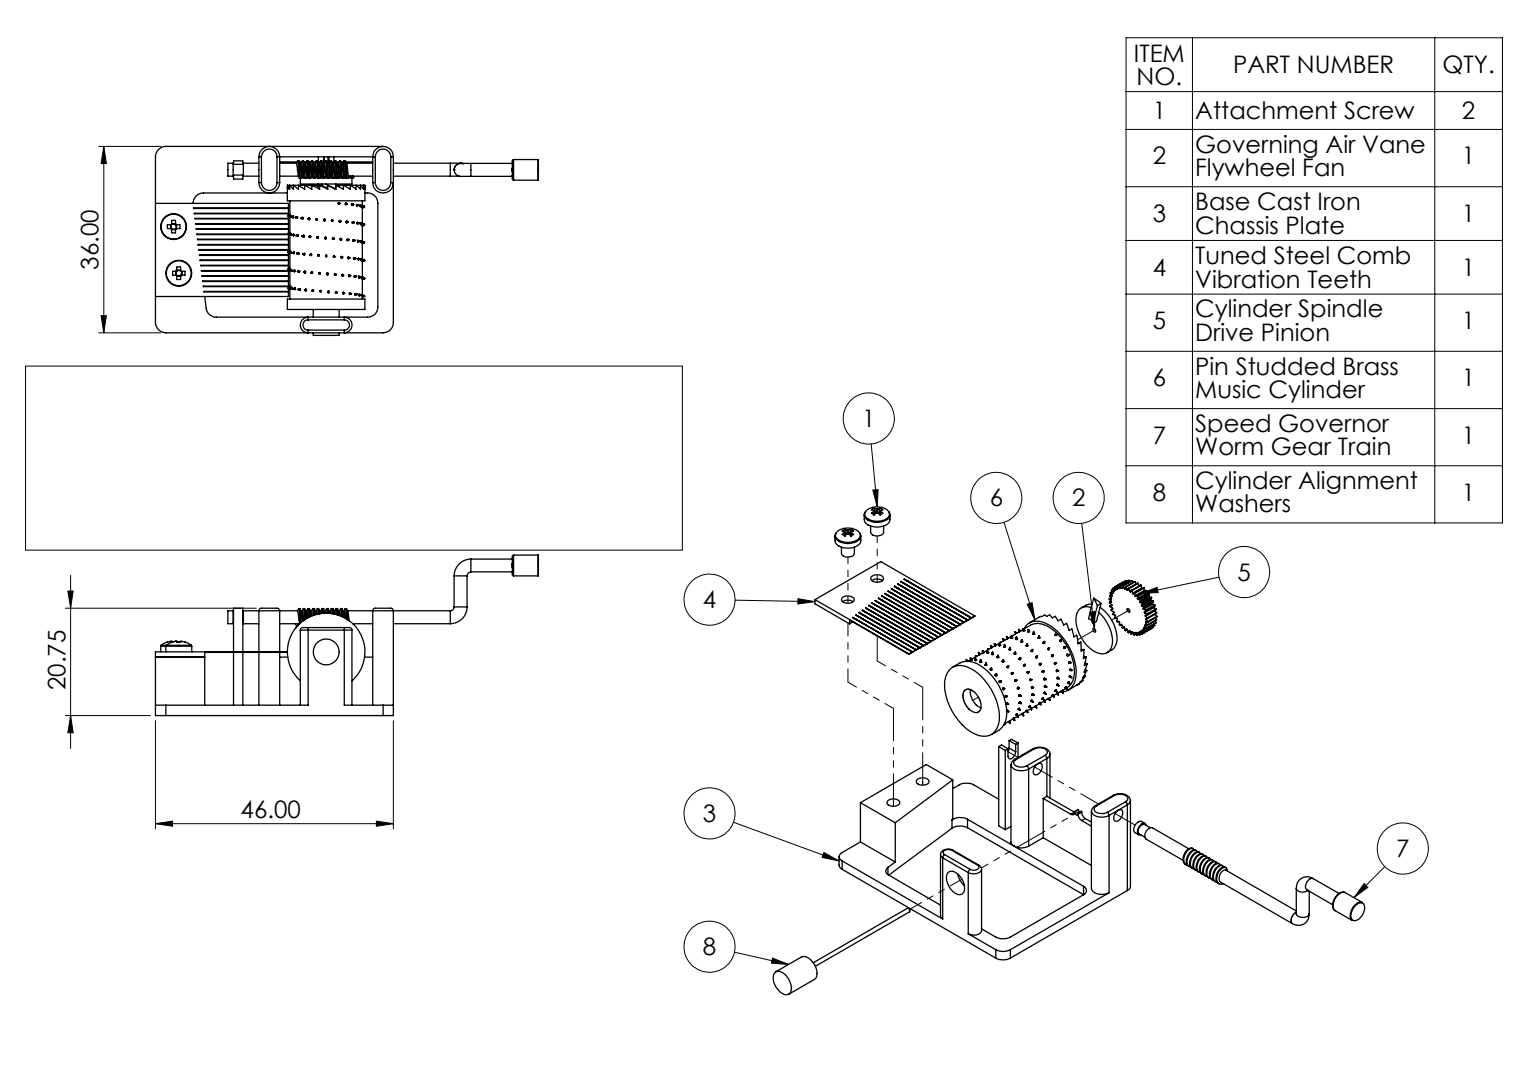
ISO-10303-21;
HEADER;
FILE_DESCRIPTION (('STEP AP214'),
    '1' );
FILE_NAME ('MAS-175',
    '2026-10-09T09:51:18',
    ( '' ),
    ( '' ),
    'SwSTEP 2.0',
    'SolidWorks 2026',
    '' );
FILE_SCHEMA (( 'AUTOMOTIVE_DESIGN' ));
ENDSEC;

DATA;
#1 = SHAPE_REPRESENTATION_RELATIONSHIP ( 'NONE' , 'NONE' ,  #34837, #17929 ) ;
#2 = ADVANCED_FACE ( 'NONE', ( #22899 ), #34188, .F. ) ;
#3 = CARTESIAN_POINT ( 'NONE',  ( -10.03625575236388201, -13.84871804469525891, 57.54850793716612856 ) ) ;
#4 = CARTESIAN_POINT ( 'NONE',  ( -11.98370840013613225, -9.620047919863830899, 54.02312124697528617 ) ) ;
#5 = ADVANCED_FACE ( 'NONE', ( #2758, #44164 ), #246, .T. ) ;
#6 = ORIENTED_EDGE ( 'NONE', *, *, #28225, .T. ) ;
#7 = EDGE_CURVE ( 'NONE', #38833, #36313, #30041, .T. ) ;
#8 = ORIENTED_EDGE ( 'NONE', *, *, #40110, .F. ) ;
#9 = CARTESIAN_POINT ( 'NONE',  ( -24.74075724160099554, -16.21284971877490122, 62.77824058731629009 ) ) ;
#10 = CARTESIAN_POINT ( 'NONE',  ( -15.47038646904106685, -21.58309222549749506, 72.34575460768671462 ) ) ;
#11 = CARTESIAN_POINT ( 'NONE',  ( -11.58081676984627073, -10.85831292256293068, 57.30083494179207548 ) ) ;
#12 = CIRCLE ( 'NONE', #29107, 1.999999999999999556 ) ;
#13 = EDGE_CURVE ( 'NONE', #13987, #23723, #5050, .T. ) ;
#14 = VERTEX_POINT ( 'NONE', #21494 ) ;
#15 = AXIS2_PLACEMENT_3D ( 'NONE', #40029, #47896, #25252 ) ;
#16 = PLANE ( 'NONE',  #21145 ) ;
#17 = B_SPLINE_CURVE_WITH_KNOTS ( 'NONE', 3,
 ( #43534, #12980, #31711, #43034, #46503, #38613, #46737, #9313, #19907, #1178 ),
 .UNSPECIFIED., .F., .F.,
 ( 4, 2, 2, 2, 4 ),
 ( 0.1272669073658292960, 0.2522669073463885137, 0.3772669073268680728, 0.5022669073073477986, 0.6272669072878274132 ),
 .UNSPECIFIED. ) ;
#18 = DIRECTION ( 'NONE',  ( 0.9939059412784551073, 0.1102314832132140626, 5.576311685107536405E-08 ) ) ;
#19 = ORIENTED_EDGE ( 'NONE', *, *, #29500, .F. ) ;
#20 = DIRECTION ( 'NONE',  ( -1.927470528863183637E-16, -1.434740771370715221E-29, 1.000000000000000000 ) ) ;
#21 = CARTESIAN_POINT ( 'NONE',  ( -10.31364510401727053, -17.03300888149450998, 57.80265138661536639 ) ) ;
#22 = DIRECTION ( 'NONE',  ( -0.7107718805962432995, -0.7034225854731134264, -7.722840056494082694E-09 ) ) ;
#23 = ORIENTED_EDGE ( 'NONE', *, *, #45455, .T. ) ;
#24 = CARTESIAN_POINT ( 'NONE',  ( -21.68606299684865135, -9.256084799238676553, 66.66150029161380530 ) ) ;
#25 = VERTEX_POINT ( 'NONE', #6474 ) ;
#26 = PLANE ( 'NONE',  #30712 ) ;
#27 = FACE_OUTER_BOUND ( 'NONE', #8967, .T. ) ;
#28 = VERTEX_POINT ( 'NONE', #28867 ) ;
#29 = CARTESIAN_POINT ( 'NONE',  ( 18.07590614458695200, 1.644079634528023526, 49.42952874619304282 ) ) ;
#30 = CARTESIAN_POINT ( 'NONE',  ( -19.85891393954322837, -21.37210614461000091, 75.49999999999994316 ) ) ;
#31 = CARTESIAN_POINT ( 'NONE',  ( -20.58659385650551599, -9.302874398569244363, 51.68646062012417985 ) ) ;
#32 = CARTESIAN_POINT ( 'NONE',  ( -20.17268404433175633, -8.371407854712250796, 70.55100341248845552 ) ) ;
#33 = EDGE_CURVE ( 'NONE', #48317, #41762, #10165, .T. ) ;
#34 = CARTESIAN_POINT ( 'NONE',  ( -10.76587051450098542, -16.97017341121004463, 57.68760522235623966 ) ) ;
#35 = DIRECTION ( 'NONE',  ( -0.000000000000000000, -1.000000000000000000, 0.000000000000000000 ) ) ;
#36 = CARTESIAN_POINT ( 'NONE',  ( -14.44705700679302574, -7.979876293330282699, 63.93978841086359211 ) ) ;
#37 = ORIENTED_EDGE ( 'NONE', *, *, #6492, .T. ) ;
#38 = CARTESIAN_POINT ( 'NONE',  ( -22.35534385541302527, -8.623186033802584305, 49.24843789510462955 ) ) ;
#39 = DIRECTION ( 'NONE',  ( -3.071710424422018668E-17, 6.404604876783312462E-16, 1.000000000000000000 ) ) ;
#40 = LINE ( 'NONE', #15026, #36087 ) ;
#41 = DIRECTION ( 'NONE',  ( -0.9942595023566571655, 0.1069955231469581908, -3.800058679842194246E-08 ) ) ;
#42 = CARTESIAN_POINT ( 'NONE',  ( -45.46395726858714426, -13.72754205882879042, 70.13000000000000966 ) ) ;
#43 = LINE ( 'NONE', #45603, #5826 ) ;
#44 = ORIENTED_EDGE ( 'NONE', *, *, #25310, .F. ) ;
#45 = ORIENTED_EDGE ( 'NONE', *, *, #29252, .T. ) ;
#46 = AXIS2_PLACEMENT_3D ( 'NONE', #24798, #28249, #13682 ) ;
#47 = CARTESIAN_POINT ( 'NONE',  ( -16.84904657224188540, -21.78683024590906925, 72.39373074617707005 ) ) ;
#48 = CARTESIAN_POINT ( 'NONE',  ( -13.27770768808251134, -9.107454094634595876, 63.90946529206384241 ) ) ;
#49 = ORIENTED_EDGE ( 'NONE', *, *, #23162, .T. ) ;
#50 = CARTESIAN_POINT ( 'NONE',  ( -24.00746423591236933, -17.19188279365308603, 73.11165851276361138 ) ) ;
#51 = CARTESIAN_POINT ( 'NONE',  ( -24.18314854330451169, -12.98801962294919932, 66.30246782466414857 ) ) ;
#52 = CARTESIAN_POINT ( 'NONE',  ( -11.64944166978149909, -18.76574910929434736, 64.81995021385422717 ) ) ;
#53 = CARTESIAN_POINT ( 'NONE',  ( -24.72694767484942702, -16.28301260341204326, 62.70833288210281609 ) ) ;
#54 = DIRECTION ( 'NONE',  ( 0.5088156898428700670, 0.8608754809899750171, 5.922709712265242817E-08 ) ) ;
#55 = CARTESIAN_POINT ( 'NONE',  ( -19.57699614054808634, -21.94144247634149281, 62.17999043330664222 ) ) ;
#56 = AXIS2_PLACEMENT_3D ( 'NONE', #16644, #27734, #1141 ) ;
#57 = CARTESIAN_POINT ( 'NONE',  ( -12.74071866071660075, -9.015263582886822391, 70.96429948631303830 ) ) ;
#58 = DIRECTION ( 'NONE',  ( 0.5088156898428700670, 0.8608754809899751281, 5.922709712265243479E-08 ) ) ;
#59 = CARTESIAN_POINT ( 'NONE',  ( -10.02934067034867915, -15.71522136325494579, 61.14450729704604015 ) ) ;
#60 = ORIENTED_EDGE ( 'NONE', *, *, #2656, .T. ) ;
#61 = CARTESIAN_POINT ( 'NONE',  ( -10.21764062494887781, -12.91954801228597915, 67.92327636273336111 ) ) ;
#62 = ADVANCED_FACE ( 'NONE', ( #10414 ), #3672, .F. ) ;
#63 = VECTOR ( 'NONE', #41726, 1000.000000000000114 ) ;
#64 = LINE ( 'NONE', #7461, #9828 ) ;
#65 = DIRECTION ( 'NONE',  ( -3.071710424422018668E-17, 6.404604876783312462E-16, 1.000000000000000000 ) ) ;
#66 = CARTESIAN_POINT ( 'NONE',  ( -21.34284385541298334, -7.587656875400150547, 49.25157356644804452 ) ) ;
#67 = CARTESIAN_POINT ( 'NONE',  ( -11.89176969907138570, -10.51836715134331079, 74.66715118432504994 ) ) ;
#68 = CARTESIAN_POINT ( 'NONE',  ( -45.92409385541305511, -17.80920654474410370, 70.50000000000000000 ) ) ;
#69 = ORIENTED_EDGE ( 'NONE', *, *, #36924, .F. ) ;
#70 = VERTEX_POINT ( 'NONE', #18679 ) ;
#71 = CARTESIAN_POINT ( 'NONE',  ( -14.25534385541304339, -8.623186033802571870, 49.24843789510467218 ) ) ;
#72 = EDGE_CURVE ( 'NONE', #44245, #17093, #1589, .T. ) ;
#73 = VERTEX_POINT ( 'NONE', #14975 ) ;
#74 = FACE_OUTER_BOUND ( 'NONE', #13777, .T. ) ;
#75 = AXIS2_PLACEMENT_3D ( 'NONE', #46607, #16288, #28114 ) ;
#76 = MANIFOLD_SOLID_BREP ( 'Stock-MAS-175-1', #12603 ) ;
#77 = CYLINDRICAL_SURFACE ( 'NONE', #4036, 0.1500000000000066835 ) ;
#78 = ADVANCED_FACE ( 'NONE', ( #20432 ), #5892, .T. ) ;
#79 = B_SPLINE_CURVE_WITH_KNOTS ( 'NONE', 1,
 ( #16390, #46203 ),
 .UNSPECIFIED., .F., .F.,
 ( 2, 2 ),
 ( 0.000000000000000000, 1.000000000000000000 ),
 .UNSPECIFIED. ) ;
#80 = AXIS2_PLACEMENT_3D ( 'NONE', #16934, #39604, #9337 ) ;
#81 = DIRECTION ( 'NONE',  ( 3.549360974555109863E-17, 1.977132801529350715E-16, 1.000000000000000000 ) ) ;
#82 = CARTESIAN_POINT ( 'NONE',  ( -18.31357640787765817, -21.80286941108919763, 68.81514702304139064 ) ) ;
#83 = EDGE_LOOP ( 'NONE', ( #31315, #30572, #42863, #38063 ) ) ;
#84 = VECTOR ( 'NONE', #15701, 1000.000000000000000 ) ;
#85 = PLANE ( 'NONE',  #90 ) ;
#86 = CARTESIAN_POINT ( 'NONE',  ( -24.16097951573440383, -12.71927508598556322, 66.51066513624088827 ) ) ;
#87 = ORIENTED_EDGE ( 'NONE', *, *, #46598, .F. ) ;
#88 = CARTESIAN_POINT ( 'NONE',  ( -22.33685117127641817, -20.40992557423668430, 62.42777465437541196 ) ) ;
#89 = EDGE_CURVE ( 'NONE', #5768, #15899, #14150, .T. ) ;
#90 = AXIS2_PLACEMENT_3D ( 'NONE', #14327, #11160, #7719 ) ;
#91 = CARTESIAN_POINT ( 'NONE',  ( -13.88293259567353743, -20.90532631576516565, 68.45625136994867432 ) ) ;
#92 = EDGE_CURVE ( 'NONE', #20698, #38947, #146, .T. ) ;
#93 = VERTEX_POINT ( 'NONE', #9602 ) ;
#94 = CARTESIAN_POINT ( 'NONE',  ( 10.57590614458695377, 0.6407533398237040823, 50.52649563099625851 ) ) ;
#95 = CARTESIAN_POINT ( 'NONE',  ( -10.02191625022346955, -15.65273779443635327, 61.15293638507743168 ) ) ;
#96 = EDGE_CURVE ( 'NONE', #20442, #47219, #874, .T. ) ;
#97 = ORIENTED_EDGE ( 'NONE', *, *, #12541, .T. ) ;
#98 = CARTESIAN_POINT ( 'NONE',  ( -10.46033444208452501, -13.68630826424936231, 57.74825279763368968 ) ) ;
#99 = LINE ( 'NONE', #37740, #35189 ) ;
#100 =( BOUNDED_CURVE ( )  B_SPLINE_CURVE ( 2, ( #3305, #14589, #15340, #3801, #41715, #30399, #23018, #10693, #7264 ),
 .UNSPECIFIED., .F., .F. ) 
 B_SPLINE_CURVE_WITH_KNOTS ( ( 3, 2, 2, 2, 3 ),
 ( 0.08333333333333348136, 0.09375000000000012490, 0.1041666666666667684, 0.1145833333333334120, 0.1250000000000000555 ),
 .UNSPECIFIED. ) 
 CURVE ( )  GEOMETRIC_REPRESENTATION_ITEM ( )  RATIONAL_B_SPLINE_CURVE ( ( 0.9999999999999988898, 0.9238795325112878487, 1.000000000000000000, 0.9238795325112867385, 1.000000000000000000, 0.9238795325112867385, 1.000000000000000000, 0.9238795325112862944, 1.000000000000000444 ) ) 
 REPRESENTATION_ITEM ( '' )  );
#101 = CARTESIAN_POINT ( 'NONE',  ( -11.81042834955647258, -10.54382735031610174, 74.45357240259568243 ) ) ;
#102 = DIRECTION ( 'NONE',  ( -0.000000000000000000, -0.000000000000000000, 1.000000000000000000 ) ) ;
#103 = EDGE_LOOP ( 'NONE', ( #13179, #38410, #7478, #14746, #26186 ) ) ;
#104 = CARTESIAN_POINT ( 'NONE',  ( -9.980660856333416930, -14.49625842079804272, 68.05788908589504160 ) ) ;
#105 = CYLINDRICAL_SURFACE ( 'NONE', #29747, 1.999999999999999556 ) ;
#106 = CARTESIAN_POINT ( 'NONE',  ( -11.75774202113761113, -19.00384077433692909, 71.83685884782747166 ) ) ;
#107 = CARTESIAN_POINT ( 'NONE',  ( -18.72484419698154667, -9.451406241145487996, 53.88362224778186516 ) ) ;
#108 = CARTESIAN_POINT ( 'NONE',  ( -16.15310590563917970, -7.468295795601643583, 60.37745339520409971 ) ) ;
#109 = CARTESIAN_POINT ( 'NONE',  ( -10.49291302059963193, -15.78914242734984263, 64.80771630040662501 ) ) ;
#110 = CARTESIAN_POINT ( 'NONE',  ( -20.49909385650551741, -8.114302828567740988, 52.18300498402516041 ) ) ;
#111 = AXIS2_PLACEMENT_3D ( 'NONE', #10985, #396, #26489 ) ;
#112 = VERTEX_POINT ( 'NONE', #24372 ) ;
#113 = CARTESIAN_POINT ( 'NONE',  ( -16.59261295876471820, -7.800382739013279831, 60.34461612587266899 ) ) ;
#114 = CARTESIAN_POINT ( 'NONE',  ( -14.54391382047218784, -7.937654553327920581, 63.97634087063163122 ) ) ;
#115 = VERTEX_POINT ( 'NONE', #13251 ) ;
#116 = CARTESIAN_POINT ( 'NONE',  ( -22.09321184435721719, -14.28490438881294189, 52.02966884056656482 ) ) ;
#117 = DIRECTION ( 'NONE',  ( 3.549360974554993999E-17, -6.371834667797928663E-18, -1.000000000000000000 ) ) ;
#118 = DIRECTION ( 'NONE',  ( 0.000000000000000000, 0.000000000000000000, 1.000000000000000000 ) ) ;
#119 =( BOUNDED_CURVE ( )  B_SPLINE_CURVE ( 3, ( #27341, #33989, #3973, #288 ),
 .UNSPECIFIED., .F., .F. ) 
 B_SPLINE_CURVE_WITH_KNOTS ( ( 4, 4 ),
 ( 0.000000000000000000, 0.4074455897393676196 ),
 .UNSPECIFIED. ) 
 CURVE ( )  GEOMETRIC_REPRESENTATION_ITEM ( )  RATIONAL_B_SPLINE_CURVE ( ( 1.000000000000000000, 0.4567392136813337444, 0.3561768502900309330, 0.6983129098260915102 ) ) 
 REPRESENTATION_ITEM ( '' )  );
#120 = ORIENTED_EDGE ( 'NONE', *, *, #48681, .F. ) ;
#121 =( BOUNDED_SURFACE ( )  B_SPLINE_SURFACE ( 3, 1, ( 
 ( #32470, #2427 ),
 ( #20663, #20424 ),
 ( #39116, #24112 ),
 ( #35421, #5884 ),
 ( #1706, #35896 ),
 ( #28292, #43320 ),
 ( #17438, #47493 ) ),
 .UNSPECIFIED., .T., .F., .F. ) 
 B_SPLINE_SURFACE_WITH_KNOTS ( ( 4, 3, 4 ),
 ( 2, 2 ),
 ( 0.000000000000000000, 0.5000000000000000000, 1.000000000000000000 ),
 ( 0.000000000000000000, 1.000000000000000000 ),
 .UNSPECIFIED. ) 
 GEOMETRIC_REPRESENTATION_ITEM ( )  RATIONAL_B_SPLINE_SURFACE ( (
 ( 1.000000000000000000, 1.000000000000000000),
 ( 0.3333333333333335369, 0.3333333333333330373),
 ( 0.3333333333333335369, 0.3333333333333330373),
 ( 1.000000000000000000, 1.000000000000000000),
 ( 0.3333333333333333703, 0.3333333333333333703),
 ( 0.3333333333333333703, 0.3333333333333333703),
 ( 1.000000000000000000, 1.000000000000000000) ) ) 
 REPRESENTATION_ITEM ( '' )  SURFACE ( )  );
#122 = DIRECTION ( 'NONE',  ( 0.06306825763707678278, -0.9980092158285026605, -2.415158932408153704E-08 ) ) ;
#123 = AXIS2_PLACEMENT_3D ( 'NONE', #20425, #35422, #737 ) ;
#124 = CARTESIAN_POINT ( 'NONE',  ( -9.424093855413051557, -25.10920654474410441, 78.99999999999998579 ) ) ;
#125 = EDGE_LOOP ( 'NONE', ( #26058, #18123, #34416, #18514, #29920 ) ) ;
#126 = CARTESIAN_POINT ( 'NONE',  ( -15.38034385650552061, -6.424090610841176385, 49.80797279389977916 ) ) ;
#127 = AXIS2_PLACEMENT_3D ( 'NONE', #27305, #34688, #22905 ) ;
#128 = CARTESIAN_POINT ( 'NONE',  ( -14.34311167289324196, -8.523215816031258996, 71.01341051612104138 ) ) ;
#129 = DIRECTION ( 'NONE',  ( 0.9687793358424823253, -0.2479245821708663811, 0.000000000000000000 ) ) ;
#130 = DIRECTION ( 'NONE',  ( -1.000000000000000000, 0.000000000000000000, 0.000000000000000000 ) ) ;
#131 = DIRECTION ( 'NONE',  ( -0.4461977533475101620, -0.8949343913984054710, 1.541409258166069499E-16 ) ) ;
#132 = AXIS2_PLACEMENT_3D ( 'NONE', #40046, #2613, #47672 ) ;
#133 =( BOUNDED_CURVE ( )  B_SPLINE_CURVE ( 3, ( #21288, #36284, #8992, #43458 ),
 .UNSPECIFIED., .F., .F. ) 
 B_SPLINE_CURVE_WITH_KNOTS ( ( 4, 4 ),
 ( 0.000000000000000000, 0.4074455897393643999 ),
 .UNSPECIFIED. ) 
 CURVE ( )  GEOMETRIC_REPRESENTATION_ITEM ( )  RATIONAL_B_SPLINE_CURVE ( ( 1.000000000000000000, 0.4567392136813379078, 0.3561768502900324873, 0.6983129098260837386 ) ) 
 REPRESENTATION_ITEM ( '' )  );
#134 = ORIENTED_EDGE ( 'NONE', *, *, #4016, .F. ) ;
#135 = ORIENTED_EDGE ( 'NONE', *, *, #41849, .T. ) ;
#136 = CARTESIAN_POINT ( 'NONE',  ( -16.53659385650551528, -6.915538690918075382, 49.31353937987644542 ) ) ;
#137 = ADVANCED_FACE ( 'NONE', ( #48154 ), #33338, .T. ) ;
#138 = B_SPLINE_CURVE_WITH_KNOTS ( 'NONE', 1,
 ( #27125, #38191 ),
 .UNSPECIFIED., .F., .F.,
 ( 2, 2 ),
 ( 0.000000000000000000, 1.000000000000000000 ),
 .UNSPECIFIED. ) ;
#139 = CARTESIAN_POINT ( 'NONE',  ( -10.44538189632046787, -14.26369805489357212, 61.02707267863189600 ) ) ;
#140 = AXIS2_PLACEMENT_3D ( 'NONE', #24664, #2235, #44833 ) ;
#141 = DIRECTION ( 'NONE',  ( -3.071710424422018668E-17, 6.404604876783312462E-16, 1.000000000000000000 ) ) ;
#142 = CARTESIAN_POINT ( 'NONE',  ( -14.45534385650551989, -7.417179338643134834, 52.18511593390279302 ) ) ;
#143 = ORIENTED_EDGE ( 'NONE', *, *, #11819, .T. ) ;
#144 = CARTESIAN_POINT ( 'NONE',  ( -15.46105799208929454, -21.99670631207736449, 72.15920124769014876 ) ) ;
#145 = AXIS2_PLACEMENT_3D ( 'NONE', #27646, #26927, #38474 ) ;
#146 = B_SPLINE_CURVE_WITH_KNOTS ( 'NONE', 3,
 ( #35431, #29443, #1718, #7046, #39128, #9108, #29205, #44244, #25744, #48389 ),
 .UNSPECIFIED., .F., .F.,
 ( 4, 2, 2, 2, 4 ),
 ( 0.000000000000000000, 0.2500000000000000000, 0.5000000000000000000, 0.7500000000000000000, 1.000000000000000000 ),
 .UNSPECIFIED. ) ;
#147 = CARTESIAN_POINT ( 'NONE',  ( -23.80321451250838649, -17.81075939459467961, 59.00378417737415049 ) ) ;
#148 = EDGE_LOOP ( 'NONE', ( #25559, #28549, #5036, #6443 ) ) ;
#149 = DIRECTION ( 'NONE',  ( 0.3478314405900310158, 0.9375570856950865561, -9.567072274253695189E-17 ) ) ;
#150 = EDGE_CURVE ( 'NONE', #31901, #23884, #35863, .T. ) ;
#151 = ORIENTED_EDGE ( 'NONE', *, *, #6962, .F. ) ;
#152 = MECHANICAL_DESIGN_GEOMETRIC_PRESENTATION_REPRESENTATION (  '', ( #21385 ), #4091 ) ;
#153 = CARTESIAN_POINT ( 'NONE',  ( -21.39967327233876304, -20.63170314183283693, 72.80974286114339122 ) ) ;
#154 = CARTESIAN_POINT ( 'NONE',  ( -24.83423444544265379, -14.03910623769390220, 73.31609816701728732 ) ) ;
#155 = EDGE_CURVE ( 'NONE', #5150, #6817, #26237, .T. ) ;
#157 = ADVANCED_FACE ( 'NONE', ( #22300 ), #19091, .T. ) ;
#156 = CARTESIAN_POINT ( 'NONE',  ( -18.50517187854146783, -19.38160480531894692, 49.52966884056656482 ) ) ;
#158 = CARTESIAN_POINT ( 'NONE',  ( -11.08846142298070880, -18.82290330472913098, 53.49999999999994316 ) ) ;
#159 = ADVANCED_FACE ( 'NONE', ( #34099 ), #4325, .T. ) ;
#160 = VECTOR ( 'NONE', #789, 1000.000000000000227 ) ;
#161 = ORIENTED_EDGE ( 'NONE', *, *, #28229, .T. ) ;
#162 = CARTESIAN_POINT ( 'NONE',  ( -10.40121522062585591, -17.29573862802152817, 61.20097198354311274 ) ) ;
#163 = CARTESIAN_POINT ( 'NONE',  ( -24.09124995986085338, -12.51712822272146042, 73.53665784698486618 ) ) ;
#164 = CARTESIAN_POINT ( 'NONE',  ( -23.56138404952065457, -11.33988834032952830, 70.19210750372964469 ) ) ;
#165 = CYLINDRICAL_SURFACE ( 'NONE', #41008, 0.1500000000000034084 ) ;
#166 = VERTEX_POINT ( 'NONE', #48638 ) ;
#167 = CARTESIAN_POINT ( 'NONE',  ( -24.72409385541305582, -14.80920654474425291, 71.08235294117645253 ) ) ;
#168 = CARTESIAN_POINT ( 'NONE',  ( -13.14998806103231566, -9.265559761403904915, 67.67942786032521951 ) ) ;
#169 = DIRECTION ( 'NONE',  ( 1.000000000000000000, -4.164305804376849172E-17, 1.614929280266638808E-16 ) ) ;
#170 = FACE_BOUND ( 'NONE', #41683, .T. ) ;
#171 = ORIENTED_EDGE ( 'NONE', *, *, #31245, .F. ) ;
#172 = DIRECTION ( 'NONE',  ( 1.000000000000000000, 1.669677910507523057E-21, 6.493791346278465266E-22 ) ) ;
#173 = CARTESIAN_POINT ( 'NONE',  ( -15.68784259522275981, -9.576290808195315307, 53.69233794759168887 ) ) ;
#174 = CARTESIAN_POINT ( 'NONE',  ( -9.939267784769082681, -14.33236412611010913, 54.27966884056655061 ) ) ;
#175 = CARTESIAN_POINT ( 'NONE',  ( -21.55884032038934350, -8.611816057827914150, 73.78624026056009200 ) ) ;
#176 = ORIENTED_EDGE ( 'NONE', *, *, #45315, .T. ) ;
#177 = CARTESIAN_POINT ( 'NONE',  ( -13.74654679279883851, -11.90422292133819582, 49.52966884056655772 ) ) ;
#178 = ORIENTED_EDGE ( 'NONE', *, *, #7182, .F. ) ;
#179 = CARTESIAN_POINT ( 'NONE',  ( -12.18170095131842068, -10.17053037870675780, 64.02914326641410980 ) ) ;
#180 = DIRECTION ( 'NONE',  ( -2.866981220435666553E-17, 1.000000000000000000, 1.190614954331866791E-16 ) ) ;
#181 = B_SPLINE_CURVE_WITH_KNOTS ( 'NONE', 1,
 ( #24932, #10158 ),
 .UNSPECIFIED., .F., .F.,
 ( 2, 2 ),
 ( 0.000000000000000000, 1.000000000000000000 ),
 .UNSPECIFIED. ) ;
#182 = LINE ( 'NONE', #415, #745 ) ;
#183 = ORIENTED_EDGE ( 'NONE', *, *, #25838, .F. ) ;
#184 = CARTESIAN_POINT ( 'NONE',  ( -45.92409385541306222, -14.20920654474410760, 70.50000000000000000 ) ) ;
#185 = ORIENTED_EDGE ( 'NONE', *, *, #14224, .F. ) ;
#186 = EDGE_CURVE ( 'NONE', #10333, #39489, #16571, .T. ) ;
#187 = ORIENTED_EDGE ( 'NONE', *, *, #3019, .F. ) ;
#188 = VERTEX_POINT ( 'NONE', #389 ) ;
#189 = CARTESIAN_POINT ( 'NONE',  ( -15.39235221195410652, -21.97689038623625635, 72.08929527613493349 ) ) ;
#190 = FACE_OUTER_BOUND ( 'NONE', #18555, .T. ) ;
#191 = CARTESIAN_POINT ( 'NONE',  ( -24.42668993457695592, -13.99045928592870780, 73.40799407547365263 ) ) ;
#192 = CARTESIAN_POINT ( 'NONE',  ( -11.32469211327616065, -18.34471187850051166, 57.95714594245092854 ) ) ;
#193 = FACE_OUTER_BOUND ( 'NONE', #16201, .T. ) ;
#194 = CARTESIAN_POINT ( 'NONE',  ( -14.55015457993596328, -8.362855509585410019, 70.87390454733632339 ) ) ;
#195 = CARTESIAN_POINT ( 'NONE',  ( -15.34465393633500518, -21.54586957516256263, 68.86120835375241711 ) ) ;
#196 = EDGE_LOOP ( 'NONE', ( #10385, #20529 ) ) ;
#197 = ORIENTED_EDGE ( 'NONE', *, *, #3825, .F. ) ;
#198 = CARTESIAN_POINT ( 'NONE',  ( -16.19792114999740562, -7.866354181730329742, 60.48556343814865954 ) ) ;
#199 = B_SPLINE_CURVE_WITH_KNOTS ( 'NONE', 3,
 ( #36213, #17003, #17258, #47556, #32053, #25388, #10127, #47073, #46828, #2496 ),
 .UNSPECIFIED., .F., .F.,
 ( 4, 2, 2, 2, 4 ),
 ( 0.000000000000000000, 0.2500000000000000000, 0.5000000000000000000, 0.7500000000000000000, 1.000000000000000000 ),
 .UNSPECIFIED. ) ;
#200 = VECTOR ( 'NONE', #37343, 1000.000000000000000 ) ;
#201 = EDGE_CURVE ( 'NONE', #20782, #44291, #26002, .T. ) ;
#202 = CARTESIAN_POINT ( 'NONE',  ( -22.54212894027171643, -20.22308674935842276, 65.88138641420671604 ) ) ;
#203 = DIRECTION ( 'NONE',  ( 1.927470528863184130E-16, 1.434740771370715221E-29, -1.000000000000000000 ) ) ;
#204 = CARTESIAN_POINT ( 'NONE',  ( -21.56183007311343758, -9.162502203718322136, 70.41516033260253948 ) ) ;
#205 = VERTEX_POINT ( 'NONE', #7298 ) ;
#206 = CARTESIAN_POINT ( 'NONE',  ( -15.09909385650551705, -8.114302828567740988, 52.18300498402516041 ) ) ;
#207 = ORIENTED_EDGE ( 'NONE', *, *, #41740, .T. ) ;
#208 = DIRECTION ( 'NONE',  ( -0.9757441136919990932, -0.2189141945955432600, 0.000000000000000000 ) ) ;
#209 = CARTESIAN_POINT ( 'NONE',  ( -13.42364920204782841, -9.064338107659910548, 49.69363550579117117 ) ) ;
#210 = DIRECTION ( 'NONE',  ( 0.2196488028684550897, 0.9755790093059856227, -7.835600157377411709E-08 ) ) ;
#211 =( BOUNDED_SURFACE ( )  B_SPLINE_SURFACE ( 3, 1, ( 
 ( #3331, #29681 ),
 ( #37286, #39375 ),
 ( #13247, #28301 ),
 ( #9599, #24612 ),
 ( #39614, #20905 ),
 ( #29932, #18842 ),
 ( #11449, #11220 ) ),
 .UNSPECIFIED., .T., .F., .F. ) 
 B_SPLINE_SURFACE_WITH_KNOTS ( ( 4, 3, 4 ),
 ( 2, 2 ),
 ( 0.000000000000000000, 0.5000000000000000000, 1.000000000000000000 ),
 ( 0.000000000000000000, 1.000000000000000000 ),
 .UNSPECIFIED. ) 
 GEOMETRIC_REPRESENTATION_ITEM ( )  RATIONAL_B_SPLINE_SURFACE ( (
 ( 1.000000000000000000, 1.000000000000000000),
 ( 0.3333333333333335369, 0.3333333333333330373),
 ( 0.3333333333333335369, 0.3333333333333330373),
 ( 1.000000000000000000, 1.000000000000000000),
 ( 0.3333333333333333703, 0.3333333333333333703),
 ( 0.3333333333333333703, 0.3333333333333333703),
 ( 1.000000000000000000, 1.000000000000000000) ) ) 
 REPRESENTATION_ITEM ( '' )  SURFACE ( )  );
#212 = ORIENTED_EDGE ( 'NONE', *, *, #4432, .T. ) ;
#213 = B_SPLINE_CURVE_WITH_KNOTS ( 'NONE', 1,
 ( #33678, #3925 ),
 .UNSPECIFIED., .F., .F.,
 ( 2, 2 ),
 ( 0.000000000000000000, 1.000000000000000000 ),
 .UNSPECIFIED. ) ;
#214 = CYLINDRICAL_SURFACE ( 'NONE', #2262, 0.1500000000000026867 ) ;
#215 = CARTESIAN_POINT ( 'NONE',  ( -10.49912617938483628, -17.55847672437320028, 64.74084113084838066 ) ) ;
#216 = EDGE_CURVE ( 'NONE', #42645, #18548, #11212, .T. ) ;
#217 = EDGE_CURVE ( 'NONE', #27248, #30011, #26822, .T. ) ;
#218 = EDGE_LOOP ( 'NONE', ( #34553, #46126, #27909, #171, #16080 ) ) ;
#219 = DIRECTION ( 'NONE',  ( -0.03181436478788690625, -0.9994937949748078365, -6.982004198809110323E-09 ) ) ;
#220 = CARTESIAN_POINT ( 'NONE',  ( -10.13411916705081950, -16.34564720852668884, 71.62467237673240561 ) ) ;
#221 = CARTESIAN_POINT ( 'NONE',  ( -9.974215857974789046, -14.86484893678357544, 74.91283499353951925 ) ) ;
#222 = ORIENTED_EDGE ( 'NONE', *, *, #28530, .T. ) ;
#223 = CARTESIAN_POINT ( 'NONE',  ( -24.67958393122153282, -16.50120980550295613, 59.26299101463538221 ) ) ;
#224 = ORIENTED_EDGE ( 'NONE', *, *, #25555, .F. ) ;
#225 = CARTESIAN_POINT ( 'NONE',  ( -10.33531725737393181, -17.10115422170377641, 57.87255955594724810 ) ) ;
#226 = EDGE_CURVE ( 'NONE', #34970, #8191, #23283, .T. ) ;
#227 = EDGE_CURVE ( 'NONE', #31196, #14322, #2991, .T. ) ;
#228 = DIRECTION ( 'NONE',  ( -0.8743548079231423520, -0.4852872034802501178, 5.778319183281970132E-08 ) ) ;
#229 = ORIENTED_EDGE ( 'NONE', *, *, #12454, .F. ) ;
#230 = CARTESIAN_POINT ( 'NONE',  ( -23.84087120742880117, -12.00869232914290841, 59.55405921996587892 ) ) ;
#231 = EDGE_CURVE ( 'NONE', #5198, #11939, #41252, .T. ) ;
#232 = CARTESIAN_POINT ( 'NONE',  ( -20.59081119662036485, -8.510278447070987795, 63.31681297810601450 ) ) ;
#233 = ORIENTED_EDGE ( 'NONE', *, *, #20231, .T. ) ;
#234 = CARTESIAN_POINT ( 'NONE',  ( -17.85728874018076340, -21.84618329174708151, 61.89007996730683203 ) ) ;
#235 = CARTESIAN_POINT ( 'NONE',  ( -22.25933006198147623, -19.87095799428289666, 65.71924198175659626 ) ) ;
#236 = LINE ( 'NONE', #3923, #40839 ) ;
#237 = ORIENTED_EDGE ( 'NONE', *, *, #40366, .T. ) ;
#238 = CARTESIAN_POINT ( 'NONE',  ( -24.03160980685186487, -17.26750534774173929, 69.41339792588560442 ) ) ;
#239 = CARTESIAN_POINT ( 'NONE',  ( -20.81693178527791943, -20.99322608020143477, 65.67634157851000509 ) ) ;
#240 = EDGE_CURVE ( 'NONE', #21614, #9195, #13538, .T. ) ;
#241 = VERTEX_POINT ( 'NONE', #4094 ) ;
#242 = ORIENTED_EDGE ( 'NONE', *, *, #46764, .F. ) ;
#243 = CARTESIAN_POINT ( 'NONE',  ( -10.49020387924836761, -15.76942919235743013, 61.26462351667871076 ) ) ;
#244 = CARTESIAN_POINT ( 'NONE',  ( -19.18034385759799321, -9.360768649639298999, 51.01397948905921709 ) ) ;
#245 = CARTESIAN_POINT ( 'NONE',  ( -19.86569447268030686, -19.73755174630646536, 54.07175714974878389 ) ) ;
#246 = PLANE ( 'NONE',  #37799 ) ;
#247 = CARTESIAN_POINT ( 'NONE',  ( -22.58034385650552167, -6.424090610841174609, 49.80797279389977916 ) ) ;
#248 = CARTESIAN_POINT ( 'NONE',  ( -24.42668993457695592, -13.99045928592870958, 73.40799407547365263 ) ) ;
#249 = CARTESIAN_POINT ( 'NONE',  ( -11.10300703817161327, -10.86615712478015539, 57.39398594787093089 ) ) ;
#250 = CARTESIAN_POINT ( 'NONE',  ( -20.50783493979771421, -8.027295371342848540, 66.96599508560271374 ) ) ;
#251 = CARTESIAN_POINT ( 'NONE',  ( -9.974485213446937948, -14.88680260109476805, 74.89804658166208640 ) ) ;
#252 = ORIENTED_EDGE ( 'NONE', *, *, #29570, .F. ) ;
#253 = B_SPLINE_CURVE_WITH_KNOTS ( 'NONE', 3,
 ( #32293, #44346, #6180, #32750, #21450, #2715, #14493, #36434, #43618, #13547 ),
 .UNSPECIFIED., .F., .F.,
 ( 4, 2, 2, 2, 4 ),
 ( 0.6272669072877669061, 0.7522669073072844048, 0.8772669073268017925, 1.002266907346319291, 1.127266907365836790 ),
 .UNSPECIFIED. ) ;
#254 = DIRECTION ( 'NONE',  ( -0.5022914217388750879, 0.8646984027090224290, 6.766381827299039861E-08 ) ) ;
#255 = VECTOR ( 'NONE', #23047, 1000.000000000000000 ) ;
#256 = CARTESIAN_POINT ( 'NONE',  ( -10.44916039635137039, -15.83526825291551177, 64.50771589744864798 ) ) ;
#257 = FACE_OUTER_BOUND ( 'NONE', #41727, .T. ) ;
#258 =( BOUNDED_SURFACE ( )  B_SPLINE_SURFACE ( 3, 1, ( 
 ( #12645, #30891 ),
 ( #19547, #27669 ),
 ( #35286, #42701 ),
 ( #8965, #19806 ),
 ( #23985, #34558 ),
 ( #34807, #16808 ),
 ( #38986, #27907 ) ),
 .UNSPECIFIED., .T., .F., .F. ) 
 B_SPLINE_SURFACE_WITH_KNOTS ( ( 4, 3, 4 ),
 ( 2, 2 ),
 ( 0.000000000000000000, 0.5000000000000000000, 1.000000000000000000 ),
 ( 0.000000000000000000, 1.000000000000000000 ),
 .UNSPECIFIED. ) 
 GEOMETRIC_REPRESENTATION_ITEM ( )  RATIONAL_B_SPLINE_SURFACE ( (
 ( 1.000000000000000000, 1.000000000000000000),
 ( 0.3333333333333335369, 0.3333333333333330373),
 ( 0.3333333333333335369, 0.3333333333333330373),
 ( 1.000000000000000000, 1.000000000000000000),
 ( 0.3333333333333333703, 0.3333333333333333703),
 ( 0.3333333333333333703, 0.3333333333333333703),
 ( 1.000000000000000000, 1.000000000000000000) ) ) 
 REPRESENTATION_ITEM ( '' )  SURFACE ( )  );
#259 = EDGE_LOOP ( 'NONE', ( #11996, #26220, #36249, #37738, #32112 ) ) ;
#260 = VERTEX_POINT ( 'NONE', #11960 ) ;
#261 = PLANE ( 'NONE',  #46906 ) ;
#262 = DIRECTION ( 'NONE',  ( 1.000000000000000000, 0.000000000000000000, 0.000000000000000000 ) ) ;
#263 = DIRECTION ( 'NONE',  ( 0.8398192074808117358, 0.5428661886195298436, 7.907900705247678986E-08 ) ) ;
#264 = FACE_OUTER_BOUND ( 'NONE', #3313, .T. ) ;
#265 = ADVANCED_FACE ( 'NONE', ( #8266 ), #28714, .T. ) ;
#266 = EDGE_LOOP ( 'NONE', ( #5129, #25117, #30541, #44712, #25689 ) ) ;
#267 =( BOUNDED_SURFACE ( )  B_SPLINE_SURFACE ( 3, 1, ( 
 ( #4799, #23276 ),
 ( #30184, #27440 ),
 ( #41983, #42225 ),
 ( #11696, #4317 ),
 ( #23767, #8256 ),
 ( #38762, #38256 ),
 ( #19824, #20056 ) ),
 .UNSPECIFIED., .T., .F., .F. ) 
 B_SPLINE_SURFACE_WITH_KNOTS ( ( 4, 3, 4 ),
 ( 2, 2 ),
 ( 0.000000000000000000, 0.5000000000000000000, 1.000000000000000000 ),
 ( 0.000000000000000000, 1.000000000000000000 ),
 .UNSPECIFIED. ) 
 GEOMETRIC_REPRESENTATION_ITEM ( )  RATIONAL_B_SPLINE_SURFACE ( (
 ( 1.000000000000000000, 1.000000000000000000),
 ( 0.3333333333333335369, 0.3333333333333330373),
 ( 0.3333333333333335369, 0.3333333333333330373),
 ( 1.000000000000000000, 1.000000000000000000),
 ( 0.3333333333333333703, 0.3333333333333333703),
 ( 0.3333333333333333703, 0.3333333333333333703),
 ( 1.000000000000000000, 1.000000000000000000) ) ) 
 REPRESENTATION_ITEM ( '' )  SURFACE ( )  );
#268 = CARTESIAN_POINT ( 'NONE',  ( -23.54782545260626136, -11.41793123268749532, 66.49502567849339130 ) ) ;
#269 = CARTESIAN_POINT ( 'NONE',  ( -14.16114181629738589, -8.110937519819053421, 67.37319822901852717 ) ) ;
#270 = EDGE_CURVE ( 'NONE', #48679, #8571, #43948, .T. ) ;
#271 = ORIENTED_EDGE ( 'NONE', *, *, #34280, .T. ) ;
#272 = CARTESIAN_POINT ( 'NONE',  ( -22.79960313759534074, -9.650943445293346912, 73.66656413195866548 ) ) ;
#273 = CARTESIAN_POINT ( 'NONE',  ( -10.88209246082447912, -17.29963176008448400, 64.92739380462948873 ) ) ;
#274 = ORIENTED_EDGE ( 'NONE', *, *, #1986, .F. ) ;
#275 = CARTESIAN_POINT ( 'NONE',  ( -17.53144753494939323, -7.808750373834428160, 67.24869371032770005 ) ) ;
#276 = ORIENTED_EDGE ( 'NONE', *, *, #38105, .F. ) ;
#277 = ADVANCED_FACE ( 'NONE', ( #22486 ), #33722, .T. ) ;
#278 = CARTESIAN_POINT ( 'NONE',  ( -22.73317970229575025, -20.03675580610048712, 72.83055794290764595 ) ) ;
#279 = CARTESIAN_POINT ( 'NONE',  ( -11.10386160987148862, -10.86480171160796893, 57.25257256893876701 ) ) ;
#280 = ORIENTED_EDGE ( 'NONE', *, *, #26061, .T. ) ;
#281 = DIRECTION ( 'NONE',  ( -3.071710424422018668E-17, 6.404604876783312462E-16, 1.000000000000000000 ) ) ;
#282 = CARTESIAN_POINT ( 'NONE',  ( -10.40830226666251157, -14.07974499963562920, 64.47983968490285633 ) ) ;
#283 = ADVANCED_FACE ( 'NONE', ( #26188 ), #36999, .T. ) ;
#284 = CARTESIAN_POINT ( 'NONE',  ( -20.98034385650551314, -6.424090610841176385, 49.80797279389978627 ) ) ;
#285 = CARTESIAN_POINT ( 'NONE',  ( -10.37840828709523322, -12.38598989307629061, 60.98508858522948373 ) ) ;
#286 = ADVANCED_FACE ( 'NONE', ( #25686 ), #14968, .F. ) ;
#287 = PLANE ( 'NONE',  #36864 ) ;
#288 = CARTESIAN_POINT ( 'NONE',  ( -10.48067290732983281, -16.03043740265091444, 67.97767830707738312 ) ) ;
#289 = DIRECTION ( 'NONE',  ( 1.224646799147353207E-16, 1.000000000000000000, -1.912410701131276611E-32 ) ) ;
#290 = ORIENTED_EDGE ( 'NONE', *, *, #4920, .T. ) ;
#291 = CARTESIAN_POINT ( 'NONE',  ( -22.18659385541302242, -7.222650657624079429, 49.61879703869474412 ) ) ;
#292 = CARTESIAN_POINT ( 'NONE',  ( -13.12613471901881113, -20.89454346209081947, 58.16154795605982031 ) ) ;
#293 = CARTESIAN_POINT ( 'NONE',  ( -23.48344415125163565, -18.41350569598871090, 73.04896097104848707 ) ) ;
#294 = CARTESIAN_POINT ( 'NONE',  ( -36.42409385541304800, -9.359200813967566646, 50.49621490985803263 ) ) ;
#295 = CARTESIAN_POINT ( 'NONE',  ( -24.20309392561631512, -13.06392267828124432, 63.11798765125330135 ) ) ;
#296 = ORIENTED_EDGE ( 'NONE', *, *, #4735, .T. ) ;
#297 = ORIENTED_EDGE ( 'NONE', *, *, #9751, .F. ) ;
#298 = CARTESIAN_POINT ( 'NONE',  ( -16.94342153774571713, -21.79279417793566154, 72.16543237156788848 ) ) ;
#299 = DIRECTION ( 'NONE',  ( 0.3636930986378153485, 0.9315188296557532777, -1.850371886801397451E-09 ) ) ;
#300 = VERTEX_POINT ( 'NONE', #7486 ) ;
#301 = CARTESIAN_POINT ( 'NONE',  ( -10.40860991809309155, -15.50898095412354571, 57.85320721669017985 ) ) ;
#302 = CARTESIAN_POINT ( 'NONE',  ( -14.96339028783852676, -21.42433367428847291, 68.72025781230657060 ) ) ;
#303 = CARTESIAN_POINT ( 'NONE',  ( -15.53265176333180619, -21.60105060138385014, 72.33103357390284316 ) ) ;
#304 = CARTESIAN_POINT ( 'NONE',  ( -17.20139284005516700, -7.812749994621428051, 70.79035839633094440 ) ) ;
#305 = EDGE_CURVE ( 'NONE', #24134, #2153, #45318, .T. ) ;
#306 = CARTESIAN_POINT ( 'NONE',  ( -21.54495561387301450, -21.01579894740183363, 72.63172296156072605 ) ) ;
#307 = FACE_OUTER_BOUND ( 'NONE', #29969, .T. ) ;
#308 = CARTESIAN_POINT ( 'NONE',  ( -24.64621740481133116, -16.83181165628401033, 53.49999999999994316 ) ) ;
#309 = DIRECTION ( 'NONE',  ( -3.071710424422018668E-17, 6.404604876783312462E-16, 1.000000000000000000 ) ) ;
#310 = FACE_OUTER_BOUND ( 'NONE', #34779, .T. ) ;
#311 = DIRECTION ( 'NONE',  ( 0.9000732436326450703, 0.4357386327795698677, -2.072980810833656879E-08 ) ) ;
#312 = CARTESIAN_POINT ( 'NONE',  ( -50.42609385541305755, -14.80920654474418008, 64.94117647058821774 ) ) ;
#313 = VERTEX_POINT ( 'NONE', #41198 ) ;
#314 = ORIENTED_EDGE ( 'NONE', *, *, #26794, .T. ) ;
#315 = CARTESIAN_POINT ( 'NONE',  ( -13.69284385541304161, -8.630756214087126565, 51.74842643355248129 ) ) ;
#316 = ORIENTED_EDGE ( 'NONE', *, *, #24449, .T. ) ;
#317 = FACE_OUTER_BOUND ( 'NONE', #17345, .T. ) ;
#318 = CIRCLE ( 'NONE', #2655, 2.000000000000002220 ) ;
#319 = CARTESIAN_POINT ( 'NONE',  ( -14.41428173599358331, -7.994163662063686893, 63.97474278339937115 ) ) ;
#320 = EDGE_CURVE ( 'NONE', #35558, #5311, #25190, .T. ) ;
#321 = CARTESIAN_POINT ( 'NONE',  ( -13.54823245630065998, -20.69819609872913801, 61.81646323537676579 ) ) ;
#322 = CARTESIAN_POINT ( 'NONE',  ( -16.10183008998876275, -22.14097689426727911, 58.47923897578370145 ) ) ;
#323 = EDGE_LOOP ( 'NONE', ( #31149, #39606, #41747, #34828, #13815, #44487, #8986, #28396, #6353, #8723, #40195, #13275, #11784, #44102 ) ) ;
#324 = CARTESIAN_POINT ( 'NONE',  ( -15.94298218261998912, -7.507746547262916792, 63.83044349608796608 ) ) ;
#325 = DIRECTION ( 'NONE',  ( -5.255974128148611414E-06, 1.684062796621483993E-06, 0.9999999999847694054 ) ) ;
#326 = ORIENTED_EDGE ( 'NONE', *, *, #4929, .T. ) ;
#327 = CARTESIAN_POINT ( 'NONE',  ( -11.49500183448702906, -10.99442376238782515, 57.22375354680192316 ) ) ;
#328 = CARTESIAN_POINT ( 'NONE',  ( -23.97105477456146261, -17.28687578273886061, 69.41339789080815592 ) ) ;
#329 = EDGE_LOOP ( 'NONE', ( #13838, #9851, #9267, #15936, #24444 ) ) ;
#330 = CARTESIAN_POINT ( 'NONE',  ( -11.12758687547136383, -10.82717111148205547, 57.40914419403284086 ) ) ;
#331 = CARTESIAN_POINT ( 'NONE',  ( -21.30368986256526043, -21.17021271237730318, 69.24105570176159574 ) ) ;
#332 = B_SPLINE_CURVE_WITH_KNOTS ( 'NONE', 3,
 ( #32504, #47759, #36419, #3183, #39890, #36180, #13765, #28808, #48006, #29048 ),
 .UNSPECIFIED., .F., .F.,
 ( 4, 2, 2, 2, 4 ),
 ( 0.1272669073658393157, 0.2522669073463362222, 0.3772669073268331008, 0.5022669073073300350, 0.6272669072878269692 ),
 .UNSPECIFIED. ) ;
#333 = CARTESIAN_POINT ( 'NONE',  ( -18.19284385541303450, -8.630756214087130118, 51.74842643355250260 ) ) ;
#334 = ORIENTED_EDGE ( 'NONE', *, *, #2116, .T. ) ;
#335 = CARTESIAN_POINT ( 'NONE',  ( -19.71243508403738076, -21.42506817177905631, 69.21865898670732520 ) ) ;
#336 = EDGE_CURVE ( 'NONE', #12470, #9257, #14096, .T. ) ;
#337 = CARTESIAN_POINT ( 'NONE',  ( -23.00442008925061899, -19.11762375203660724, 59.18410642057862248 ) ) ;
#338 = ADVANCED_FACE ( 'NONE', ( #40464 ), #45710, .T. ) ;
#339 = PLANE ( 'NONE',  #14810 ) ;
#340 = CARTESIAN_POINT ( 'NONE',  ( -10.93232766038821424, -17.55941949638709687, 68.38249893951126523 ) ) ;
#341 = ORIENTED_EDGE ( 'NONE', *, *, #46783, .F. ) ;
#342 = CARTESIAN_POINT ( 'NONE',  ( -14.78766009005058635, -21.34800739930362568, 58.45145834864037937 ) ) ;
#343 = CARTESIAN_POINT ( 'NONE',  ( 6.575906144586949331, -6.109215713985405749, 50.50605614422795497 ) ) ;
#344 = CARTESIAN_POINT ( 'NONE',  ( -23.52687218415512760, -18.35477548540580273, 69.44938804596051796 ) ) ;
#345 = CARTESIAN_POINT ( 'NONE',  ( -23.93414946104399377, -11.18647762192129314, 70.05357276016361823 ) ) ;
#346 = AXIS2_PLACEMENT_3D ( 'NONE', #48605, #22512, #26210 ) ;
#347 = EDGE_CURVE ( 'NONE', #38066, #30065, #19519, .T. ) ;
#348 = FACE_OUTER_BOUND ( 'NONE', #44342, .T. ) ;
#349 = CARTESIAN_POINT ( 'NONE',  ( -18.19284385650551528, -7.406986770994972602, 48.81910596585309747 ) ) ;
#350 = VECTOR ( 'NONE', #21836, 1000.000000000000000 ) ;
#351 = ORIENTED_EDGE ( 'NONE', *, *, #40500, .T. ) ;
#352 = CARTESIAN_POINT ( 'NONE',  ( -23.66133310609451712, -18.88359296917171903, 69.40876596050124192 ) ) ;
#353 = DIRECTION ( 'NONE',  ( 1.000000000000000000, -4.164305804376849788E-17, 1.614929280266638808E-16 ) ) ;
#354 = ORIENTED_EDGE ( 'NONE', *, *, #17755, .F. ) ;
#355 = CARTESIAN_POINT ( 'NONE',  ( -22.36289160583321944, -19.84024478656301937, 69.17417986619062731 ) ) ;
#356 = CARTESIAN_POINT ( 'NONE',  ( -24.45810293133404656, -14.28236561102681534, 73.42271650780452319 ) ) ;
#357 = CARTESIAN_POINT ( 'NONE',  ( -10.37762151648083808, -12.38827872426728050, 57.44202070861023657 ) ) ;
#358 = ADVANCED_FACE ( 'NONE', ( #45878 ), #45160, .T. ) ;
#359 = ORIENTED_EDGE ( 'NONE', *, *, #35784, .F. ) ;
#360 = ADVANCED_FACE ( 'NONE', ( #45647 ), #22994, .T. ) ;
#361 = CARTESIAN_POINT ( 'NONE',  ( -10.37534642380570027, -14.67419306300129733, 71.32782691282784526 ) ) ;
#362 = CARTESIAN_POINT ( 'NONE',  ( -10.05862335131466700, -15.92885902279982524, 64.69266873560974318 ) ) ;
#363 = CARTESIAN_POINT ( 'NONE',  ( -18.41375667457423759, -22.19335022249702050, 68.97548045702603758 ) ) ;
#364 = EDGE_LOOP ( 'NONE', ( #29959, #8982, #8125, #35145, #33682 ) ) ;
#365 = CARTESIAN_POINT ( 'NONE',  ( -15.09909385650551705, -8.114302828567740988, 52.18300498402516041 ) ) ;
#366 = CARTESIAN_POINT ( 'NONE',  ( -11.64235247690698927, -18.84330696305777764, 68.51689631558762983 ) ) ;
#367 = CARTESIAN_POINT ( 'NONE',  ( -24.80769062643263467, -15.80232089486973557, 69.71802876059763321 ) ) ;
#368 = CARTESIAN_POINT ( 'NONE',  ( -21.95692851765875631, -9.409391401937881483, 60.01611433801762985 ) ) ;
#369 = DIRECTION ( 'NONE',  ( -3.071710424422018668E-17, 6.404604876783312462E-16, 1.000000000000000000 ) ) ;
#370 = ORIENTED_EDGE ( 'NONE', *, *, #6560, .T. ) ;
#371 = EDGE_LOOP ( 'NONE', ( #15592, #28628, #42332, #39991 ) ) ;
#372 = CARTESIAN_POINT ( 'NONE',  ( -13.33034385650551812, -9.794322478646142471, 51.19202720610083901 ) ) ;
#373 = DIRECTION ( 'NONE',  ( 0.9687793358424821033, -0.2479245821708677133, 0.000000000000000000 ) ) ;
#374 = EDGE_CURVE ( 'NONE', #44110, #112, #11065, .T. ) ;
#375 = CARTESIAN_POINT ( 'NONE',  ( -16.25534385650551528, -7.417179338643134834, 52.18511593390279302 ) ) ;
#376 = CIRCLE ( 'NONE', #29497, 4.686499999999999666 ) ;
#377 = LINE ( 'NONE', #48205, #37863 ) ;
#378 = CARTESIAN_POINT ( 'NONE',  ( -10.25416474409032652, -12.78293385988982678, 67.92487701448251869 ) ) ;
#379 = AXIS2_PLACEMENT_3D ( 'NONE', #38542, #5309, #35336 ) ;
#380 = FACE_OUTER_BOUND ( 'NONE', #43337, .T. ) ;
#381 = CARTESIAN_POINT ( 'NONE',  ( -45.92409385541305511, -15.80920654474410725, 70.50000000000000000 ) ) ;
#382 =( BOUNDED_SURFACE ( )  B_SPLINE_SURFACE ( 3, 1, ( 
 ( #13535, #28583 ),
 ( #23695, #17952 ),
 ( #6413, #44567 ),
 ( #40381, #25848 ),
 ( #9867, #14250 ),
 ( #43853, #25598 ),
 ( #24883, #43609 ) ),
 .UNSPECIFIED., .T., .F., .F. ) 
 B_SPLINE_SURFACE_WITH_KNOTS ( ( 4, 3, 4 ),
 ( 2, 2 ),
 ( 0.000000000000000000, 0.5000000000000000000, 1.000000000000000000 ),
 ( 0.000000000000000000, 1.000000000000000000 ),
 .UNSPECIFIED. ) 
 GEOMETRIC_REPRESENTATION_ITEM ( )  RATIONAL_B_SPLINE_SURFACE ( (
 ( 1.000000000000000000, 1.000000000000000000),
 ( 0.3333333333333335369, 0.3333333333333330373),
 ( 0.3333333333333335369, 0.3333333333333330373),
 ( 1.000000000000000000, 1.000000000000000000),
 ( 0.3333333333333333703, 0.3333333333333333703),
 ( 0.3333333333333333703, 0.3333333333333333703),
 ( 1.000000000000000000, 1.000000000000000000) ) ) 
 REPRESENTATION_ITEM ( '' )  SURFACE ( )  );
#383 = VERTEX_POINT ( 'NONE', #19774 ) ;
#384 = CARTESIAN_POINT ( 'NONE',  ( -23.03651728895758666, -18.99332342978600252, 62.63790370423207321 ) ) ;
#385 = EDGE_CURVE ( 'NONE', #1629, #41284, #30866, .T. ) ;
#386 = ORIENTED_EDGE ( 'NONE', *, *, #34512, .T. ) ;
#387 = CARTESIAN_POINT ( 'NONE',  ( -13.33011785382929126, -9.069340661520646663, 63.92418669539090814 ) ) ;
#388 = CARTESIAN_POINT ( 'NONE',  ( -23.42532328873747005, -19.22384396101403681, 62.46911485589509994 ) ) ;
#389 = CARTESIAN_POINT ( 'NONE',  ( -19.22579631480732587, -21.57336711704104104, 58.82507384991394872 ) ) ;
#390 = CARTESIAN_POINT ( 'NONE',  ( -19.92409385541305156, -14.80920654474411080, 47.99999999999997868 ) ) ;
#391 = ORIENTED_EDGE ( 'NONE', *, *, #42461, .T. ) ;
#392 = CARTESIAN_POINT ( 'NONE',  ( -17.98584054083101691, -22.23808389992613499, 62.06031238270200845 ) ) ;
#393 = DIRECTION ( 'NONE',  ( 0.9372362738803844406, 0.3486949482324239735, -5.386914174890154601E-09 ) ) ;
#394 =( BOUNDED_CURVE ( )  B_SPLINE_CURVE ( 3, ( #3848, #18104, #7543, #37546 ),
 .UNSPECIFIED., .F., .F. ) 
 B_SPLINE_CURVE_WITH_KNOTS ( ( 4, 4 ),
 ( 0.9074455897393690629, 1.000000000000000000 ),
 .UNSPECIFIED. ) 
 CURVE ( )  GEOMETRIC_REPRESENTATION_ITEM ( )  RATIONAL_B_SPLINE_CURVE ( ( 0.6983129098260929535, 0.7760317562606982023, 0.8765941196520005141, 1.000000000000000000 ) ) 
 REPRESENTATION_ITEM ( '' )  );
#395 = CARTESIAN_POINT ( 'NONE',  ( -14.09914643654217947, -8.649277595337252933, 74.49954655170296292 ) ) ;
#396 = DIRECTION ( 'NONE',  ( -0.9000732436326450703, -0.4357386327795698677, 2.072980810273451787E-08 ) ) ;
#397 = ORIENTED_EDGE ( 'NONE', *, *, #17162, .F. ) ;
#398 = FACE_OUTER_BOUND ( 'NONE', #46859, .T. ) ;
#399 = CARTESIAN_POINT ( 'NONE',  ( -10.90759844528708911, -17.49952021360972765, 68.24721944423116327 ) ) ;
#400 =( BOUNDED_SURFACE ( )  B_SPLINE_SURFACE ( 3, 1, ( 
 ( #20895, #24356 ),
 ( #27793, #42821 ),
 ( #39365, #5650 ),
 ( #4919, #20658 ),
 ( #35890, #2171 ),
 ( #13488, #43558 ),
 ( #34933, #1199 ) ),
 .UNSPECIFIED., .T., .F., .F. ) 
 B_SPLINE_SURFACE_WITH_KNOTS ( ( 4, 3, 4 ),
 ( 2, 2 ),
 ( 0.000000000000000000, 0.5000000000000000000, 1.000000000000000000 ),
 ( 0.000000000000000000, 1.000000000000000000 ),
 .UNSPECIFIED. ) 
 GEOMETRIC_REPRESENTATION_ITEM ( )  RATIONAL_B_SPLINE_SURFACE ( (
 ( 1.000000000000000000, 1.000000000000000000),
 ( 0.3333333333333335369, 0.3333333333333330373),
 ( 0.3333333333333335369, 0.3333333333333330373),
 ( 1.000000000000000000, 1.000000000000000000),
 ( 0.3333333333333333703, 0.3333333333333333703),
 ( 0.3333333333333333703, 0.3333333333333333703),
 ( 1.000000000000000000, 1.000000000000000000) ) ) 
 REPRESENTATION_ITEM ( '' )  SURFACE ( )  );
#401 = CARTESIAN_POINT ( 'NONE',  ( -23.27571566865760033, -18.75553318983527262, 72.90801392080540211 ) ) ;
#402 = FACE_BOUND ( 'NONE', #15605, .T. ) ;
#403 = APPLICATION_PROTOCOL_DEFINITION ( 'draft international standard', 'automotive_design', 1998, #44189 ) ;
#405 = EDGE_CURVE ( 'NONE', #45877, #29512, #47050, .T. ) ;
#404 = ORIENTED_EDGE ( 'NONE', *, *, #13134, .T. ) ;
#406 = CARTESIAN_POINT ( 'NONE',  ( -10.33531692083374587, -17.10115316349580894, 57.87255846826901262 ) ) ;
#407 = CARTESIAN_POINT ( 'NONE',  ( -18.18338144371267617, -21.81849904615365432, 65.63060065626805795 ) ) ;
#408 = CARTESIAN_POINT ( 'NONE',  ( -23.11971029740161754, -18.96910916387263768, 66.23878312252503520 ) ) ;
#409 = ADVANCED_FACE ( 'NONE', ( #15316 ), #30378, .T. ) ;
#410 = ORIENTED_EDGE ( 'NONE', *, *, #41877, .F. ) ;
#411 = CARTESIAN_POINT ( 'NONE',  ( -11.64902330566212463, -10.02396254413167576, 54.27966884056655061 ) ) ;
#412 = EDGE_LOOP ( 'NONE', ( #31242, #8262, #36518, #17032, #48604 ) ) ;
#413 = DIRECTION ( 'NONE',  ( -0.9687793358424822143, 0.2479245821708672415, 0.000000000000000000 ) ) ;
#414 = CARTESIAN_POINT ( 'NONE',  ( -20.84119928492008000, -20.97572016636869918, 62.41471400470057773 ) ) ;
#415 = CARTESIAN_POINT ( 'NONE',  ( -26.42409385541305511, -6.859206544744110623, 63.99999999999998579 ) ) ;
#416 = ORIENTED_EDGE ( 'NONE', *, *, #43313, .F. ) ;
#417 =( BOUNDED_SURFACE ( )  B_SPLINE_SURFACE ( 3, 1, ( 
 ( #9732, #43708 ),
 ( #24518, #28912 ),
 ( #16610, #13866 ),
 ( #28443, #43468 ),
 ( #32380, #47398 ),
 ( #9963, #10214 ),
 ( #28194, #17083 ) ),
 .UNSPECIFIED., .T., .F., .F. ) 
 B_SPLINE_SURFACE_WITH_KNOTS ( ( 4, 3, 4 ),
 ( 2, 2 ),
 ( 0.000000000000000000, 0.5000000000000000000, 1.000000000000000000 ),
 ( 0.000000000000000000, 1.000000000000000000 ),
 .UNSPECIFIED. ) 
 GEOMETRIC_REPRESENTATION_ITEM ( )  RATIONAL_B_SPLINE_SURFACE ( (
 ( 1.000000000000000000, 1.000000000000000000),
 ( 0.3333333333333335369, 0.3333333333333330373),
 ( 0.3333333333333335369, 0.3333333333333330373),
 ( 1.000000000000000000, 1.000000000000000000),
 ( 0.3333333333333333703, 0.3333333333333333703),
 ( 0.3333333333333333703, 0.3333333333333333703),
 ( 1.000000000000000000, 1.000000000000000000) ) ) 
 REPRESENTATION_ITEM ( '' )  SURFACE ( )  );
#418 = AXIS2_PLACEMENT_3D ( 'NONE', #26156, #2536, #11134 ) ;
#419 = CARTESIAN_POINT ( 'NONE',  ( -13.17364477763805652, -9.395196358873663556, 49.41429196092195042 ) ) ;
#420 = ORIENTED_EDGE ( 'NONE', *, *, #27980, .F. ) ;
#421 = CIRCLE ( 'NONE', #10633, 5.249999999999998224 ) ;
#422 = EDGE_LOOP ( 'NONE', ( #46320, #35435, #35647 ) ) ;
#423 = EDGE_LOOP ( 'NONE', ( #39334, #48242, #40910, #3394 ) ) ;
#424 = CARTESIAN_POINT ( 'NONE',  ( -15.49416032233947504, -8.028509233753512220, 74.07985659018982005 ) ) ;
#425 = CARTESIAN_POINT ( 'NONE',  ( -22.31677934746245384, -19.81551963994498777, 69.17417984703425304 ) ) ;
#426 = CARTESIAN_POINT ( 'NONE',  ( -12.84615363328625826, -20.17103110633857455, 72.09181604382622766 ) ) ;
#427 = CARTESIAN_POINT ( 'NONE',  ( -16.65185932245351808, -21.81708442718849383, 65.51092266128213737 ) ) ;
#428 = CARTESIAN_POINT ( 'NONE',  ( -19.03659385541296345, -8.995762431863310482, 51.38120296130595221 ) ) ;
#429 = EDGE_CURVE ( 'NONE', #3477, #10747, #43455, .T. ) ;
#430 = DIRECTION ( 'NONE',  ( 2.866981220435666553E-17, -1.000000000000000000, -1.190614954331866791E-16 ) ) ;
#431 = CARTESIAN_POINT ( 'NONE',  ( -12.49710231520240988, -20.39756436883700630, 71.96800174581260023 ) ) ;
#432 = EDGE_CURVE ( 'NONE', #1919, #29759, #26919, .T. ) ;
#433 = ORIENTED_EDGE ( 'NONE', *, *, #28932, .T. ) ;
#434 = ORIENTED_EDGE ( 'NONE', *, *, #20231, .F. ) ;
#435 = CARTESIAN_POINT ( 'NONE',  ( -17.70854774853812330, -7.363889232077062807, 63.73712292196469065 ) ) ;
#436 = EDGE_CURVE ( 'NONE', #14770, #31554, #12369, .T. ) ;
#437 = ADVANCED_FACE ( 'NONE', ( #38213 ), #30235, .T. ) ;
#438 = ADVANCED_FACE ( 'NONE', ( #31329 ), #8225, .T. ) ;
#439 = B_SPLINE_CURVE_WITH_KNOTS ( 'NONE', 3,
 ( #35789, #17792, #14089, #39984, #9946, #6255, #13849, #21279, #28423, #32818 ),
 .UNSPECIFIED., .F., .F.,
 ( 4, 2, 2, 2, 4 ),
 ( 0.6272669072782633970, 0.7522669073001574391, 0.8772669073220515923, 1.002266907343945634, 1.127266907365839677 ),
 .UNSPECIFIED. ) ;
#440 = CARTESIAN_POINT ( 'NONE',  ( -11.87789744022826355, -9.834800395276692697, 64.16880944724786673 ) ) ;
#441 = CARTESIAN_POINT ( 'NONE',  ( -13.50285511730657184, -21.14374568559905399, 65.13628878216876217 ) ) ;
#442 = CARTESIAN_POINT ( 'NONE',  ( -23.70015231925135168, -18.82353928378165975, 69.47867257277708575 ) ) ;
#443 = ORIENTED_EDGE ( 'NONE', *, *, #4482, .T. ) ;
#444 = CARTESIAN_POINT ( 'NONE',  ( -15.15534385650552096, -7.417179338643134834, 52.18511593390279302 ) ) ;
#445 = VERTEX_POINT ( 'NONE', #23953 ) ;
#446 = CARTESIAN_POINT ( 'NONE',  ( -14.71758685070772366, -21.32224385381664788, 62.05089037315948275 ) ) ;
#447 = CARTESIAN_POINT ( 'NONE',  ( -16.78411710364782650, -21.83009890335197767, 68.99560651669348488 ) ) ;
#448 = DIRECTION ( 'NONE',  ( 0.6478992145799701285, -0.7617260713318518839, 1.927832152310587152E-08 ) ) ;
#449 = EDGE_LOOP ( 'NONE', ( #43040, #18031 ) ) ;
#450 = B_SPLINE_CURVE_WITH_KNOTS ( 'NONE', 1,
 ( #9421, #42674 ),
 .UNSPECIFIED., .F., .F.,
 ( 2, 2 ),
 ( 0.000000000000000000, 1.000000000000000000 ),
 .UNSPECIFIED. ) ;
#451 = DIRECTION ( 'NONE',  ( 1.927470528863119542E-16, 0.000000000000000000, -1.000000000000000000 ) ) ;
#452 = EDGE_CURVE ( 'NONE', #42348, #36826, #9530, .T. ) ;
#453 = CARTESIAN_POINT ( 'NONE',  ( -24.20884359724224311, -11.73171579724705005, 59.59740298356196320 ) ) ;
#454 = VERTEX_POINT ( 'NONE', #31574 ) ;
#455 = DIRECTION ( 'NONE',  ( 0.9904243694481096316, 0.1380563957348939774, 6.973877024228147881E-08 ) ) ;
#456 = CARTESIAN_POINT ( 'NONE',  ( -10.04844915070208344, -15.85969764522557668, 64.76417530519553623 ) ) ;
#457 = ORIENTED_EDGE ( 'NONE', *, *, #29503, .T. ) ;
#458 = FACE_OUTER_BOUND ( 'NONE', #9913, .T. ) ;
#459 = EDGE_LOOP ( 'NONE', ( #3422, #20688, #46896, #525, #3593 ) ) ;
#460 = CARTESIAN_POINT ( 'NONE',  ( -23.21283044961208830, -10.11939778159179859, 63.25681392212788268 ) ) ;
#461 = DIRECTION ( 'NONE',  ( -1.224646799147353207E-16, -1.000000000000000000, 1.912410701131276611E-32 ) ) ;
#462 = ORIENTED_EDGE ( 'NONE', *, *, #6730, .F. ) ;
#463 = DIRECTION ( 'NONE',  ( -1.404489950266683237E-08, 6.428047446179355909E-07, 0.9999999999997932765 ) ) ;
#464 = CARTESIAN_POINT ( 'NONE',  ( -24.57916482434842820, -12.73107666121563142, 69.95898344571149607 ) ) ;
#465 = CARTESIAN_POINT ( 'NONE',  ( -24.24046553926340408, -13.21446260159300934, 62.84880869836692341 ) ) ;
#466 = EDGE_CURVE ( 'NONE', #32966, #27479, #6623, .T. ) ;
#467 = VERTEX_POINT ( 'NONE', #16535 ) ;
#468 = DIRECTION ( 'NONE',  ( 0.6621635203543606574, 0.7493593746073508033, 2.316976118889566110E-08 ) ) ;
#469 = CARTESIAN_POINT ( 'NONE',  ( -22.20320178312271153, -19.92390373660361291, 65.70421731406698029 ) ) ;
#470 = CARTESIAN_POINT ( 'NONE',  ( -10.95381480682210373, -17.48044017699314523, 68.09721944380058289 ) ) ;
#471 = ORIENTED_EDGE ( 'NONE', *, *, #38149, .T. ) ;
#472 = CARTESIAN_POINT ( 'NONE',  ( -22.42594789675818845, -19.77792426076253918, 69.45945937764655298 ) ) ;
#473 = CARTESIAN_POINT ( 'NONE',  ( -21.35994700726987006, -8.956524206332462157, 70.01643677269403554 ) ) ;
#474 = EDGE_LOOP ( 'NONE', ( #18767, #45773, #10429, #4944, #46509 ) ) ;
#475 = ORIENTED_EDGE ( 'NONE', *, *, #24304, .T. ) ;
#476 = CARTESIAN_POINT ( 'NONE',  ( -23.23616409499837587, -18.79948708312782557, 65.82389430043846801 ) ) ;
#477 = CARTESIAN_POINT ( 'NONE',  ( -10.16749015965427105, -13.12235144340169235, 71.39323866028058774 ) ) ;
#478 = CARTESIAN_POINT ( 'NONE',  ( -23.00190342510993347, -19.12578814502481350, 62.76895730438863552 ) ) ;
#479 = CARTESIAN_POINT ( 'NONE',  ( -17.02409385541305298, -14.80920654474411080, 47.99999999999997868 ) ) ;
#480 = CARTESIAN_POINT ( 'NONE',  ( -22.97409385650551528, -9.792211528768504536, 50.49490371617623197 ) ) ;
#481 = CARTESIAN_POINT ( 'NONE',  ( -24.37683887807358474, -15.97618392648307584, 66.36324926629207255 ) ) ;
#482 = CARTESIAN_POINT ( 'NONE',  ( -12.45682740369385044, -20.36257741321750103, 68.45002181329043367 ) ) ;
#483 = CARTESIAN_POINT ( 'NONE',  ( -17.00835460083030881, -7.370762356853859387, 74.06744117325925458 ) ) ;
#484 = CARTESIAN_POINT ( 'NONE',  ( -19.85891393954322837, -21.37210614461000446, 56.49999999999994316 ) ) ;
#485 = AXIS2_PLACEMENT_3D ( 'NONE', #1699, #42596, #17174 ) ;
#486 = VERTEX_POINT ( 'NONE', #35972 ) ;
#487 = CARTESIAN_POINT ( 'NONE',  ( -8.424093855413060439, -6.859206544744110623, 47.99999999999998579 ) ) ;
#488 = ADVANCED_FACE ( 'NONE', ( #39448 ), #12614, .T. ) ;
#489 = ADVANCED_FACE ( 'NONE', ( #27872 ), #24911, .T. ) ;
#490 = CARTESIAN_POINT ( 'NONE',  ( -10.90759836534377492, -17.49952001658422063, 68.39721944423101263 ) ) ;
#491 = ORIENTED_EDGE ( 'NONE', *, *, #37482, .F. ) ;
#492 = ADVANCED_FACE ( 'NONE', ( #31815, #46833 ), #2013, .F. ) ;
#493 = EDGE_CURVE ( 'NONE', #23300, #44829, #34132, .T. ) ;
#494 = ORIENTED_EDGE ( 'NONE', *, *, #28708, .F. ) ;
#495 = CARTESIAN_POINT ( 'NONE',  ( -19.92081508208725182, -21.34881959396637541, 69.03314256940365112 ) ) ;
#496 = CARTESIAN_POINT ( 'NONE',  ( -11.73260704738458671, -10.00184175524024610, 67.61401452035728710 ) ) ;
#497 = DIRECTION ( 'NONE',  ( 0.04108628546905145756, 0.9991556020692450302, -4.908153721456555400E-18 ) ) ;
#498 = ORIENTED_EDGE ( 'NONE', *, *, #14731, .T. ) ;
#499 = DIRECTION ( 'NONE',  ( -3.071710424422018668E-17, 6.404604876783312462E-16, 1.000000000000000000 ) ) ;
#500 = EDGE_CURVE ( 'NONE', #11264, #34652, #47330, .T. ) ;
#501 = VERTEX_POINT ( 'NONE', #17504 ) ;
#502 = CARTESIAN_POINT ( 'NONE',  ( -17.00708426123225436, -7.821638799215111071, 74.26018273346642218 ) ) ;
#503 = CARTESIAN_POINT ( 'NONE',  ( -24.14992822999210276, -18.01341164000503525, 59.11882993461590274 ) ) ;
#504 = EDGE_LOOP ( 'NONE', ( #46695, #33574, #44849, #33318, #47655 ) ) ;
#505 = CARTESIAN_POINT ( 'NONE',  ( -11.65812116532299036, -18.87225936251257252, 64.74706785490784000 ) ) ;
#506 = AXIS2_PLACEMENT_3D ( 'NONE', #33969, #37910, #7652 ) ;
#507 = VECTOR ( 'NONE', #676, 1000.000000000000000 ) ;
#508 = VERTEX_POINT ( 'NONE', #15199 ) ;
#509 = PLANE ( 'NONE',  #15734 ) ;
#510 = CARTESIAN_POINT ( 'NONE',  ( -14.90981263331598150, -21.39562362703504306, 61.93600440604522817 ) ) ;
#511 = ORIENTED_EDGE ( 'NONE', *, *, #39173, .T. ) ;
#512 = CARTESIAN_POINT ( 'NONE',  ( -10.49862840407593367, -15.82799419795606966, 64.80771590052736997 ) ) ;
#513 = DIRECTION ( 'NONE',  ( 0.9939059412784551073, 0.1102314832132140626, 5.576311685107536405E-08 ) ) ;
#514 = CARTESIAN_POINT ( 'NONE',  ( -22.16159385650551528, -9.295667164867525756, 49.30633214617472504 ) ) ;
#515 = DIRECTION ( 'NONE',  ( 0.7437128929774846631, -0.6684991644116392573, 1.736198598216997869E-08 ) ) ;
#516 = LINE ( 'NONE', #23664, #6426 ) ;
#517 = DIRECTION ( 'NONE',  ( -0.9687793358424819923, 0.2479245821708678243, 0.000000000000000000 ) ) ;
#518 = ORIENTED_EDGE ( 'NONE', *, *, #23883, .T. ) ;
#519 = CARTESIAN_POINT ( 'NONE',  ( -8.185066236809714013, -9.969861568386987116, 54.58422952202461431 ) ) ;
#520 = CARTESIAN_POINT ( 'NONE',  ( -18.15518557434651825, -21.77104687284236917, 65.34532137711126154 ) ) ;
#521 = FACE_BOUND ( 'NONE', #21781, .T. ) ;
#522 = FACE_OUTER_BOUND ( 'NONE', #47386, .T. ) ;
#523 = CARTESIAN_POINT ( 'NONE',  ( -17.12428427367203199, -7.815570071381127804, 70.50538321838570255 ) ) ;
#524 = EDGE_LOOP ( 'NONE', ( #29055, #13582, #18581, #24516, #22203 ) ) ;
#525 = ORIENTED_EDGE ( 'NONE', *, *, #13658, .F. ) ;
#526 = DIRECTION ( 'NONE',  ( 1.770046472388780670E-07, -8.183081107261190203E-08, -0.9999999999999809042 ) ) ;
#527 = CARTESIAN_POINT ( 'NONE',  ( -19.98813031515369332, -21.37641424997302053, 72.70478737316021522 ) ) ;
#528 = ORIENTED_EDGE ( 'NONE', *, *, #23306, .F. ) ;
#529 = CARTESIAN_POINT ( 'NONE',  ( -24.72409385541305582, -14.80920654474428488, 74.99999999999998579 ) ) ;
#530 = CARTESIAN_POINT ( 'NONE',  ( -15.73904783414571362, -7.552099178812579083, 67.27860723075241367 ) ) ;
#531 = CARTESIAN_POINT ( 'NONE',  ( -10.28012408155893986, -12.69583279732615821, 64.36812482108923916 ) ) ;
#532 = CARTESIAN_POINT ( 'NONE',  ( -24.72842049104188433, -16.27552959397571897, 62.70054543384251389 ) ) ;
#533 =( BOUNDED_SURFACE ( )  B_SPLINE_SURFACE ( 3, 1, ( 
 ( #15389, #11243 ),
 ( #34355, #642 ),
 ( #3600, #25764 ),
 ( #3357, #18603 ),
 ( #48657, #29958 ),
 ( #39030, #9249 ),
 ( #1607, #15643 ) ),
 .UNSPECIFIED., .T., .F., .F. ) 
 B_SPLINE_SURFACE_WITH_KNOTS ( ( 4, 3, 4 ),
 ( 2, 2 ),
 ( 0.000000000000000000, 0.5000000000000000000, 1.000000000000000000 ),
 ( 0.000000000000000000, 1.000000000000000000 ),
 .UNSPECIFIED. ) 
 GEOMETRIC_REPRESENTATION_ITEM ( )  RATIONAL_B_SPLINE_SURFACE ( (
 ( 1.000000000000000000, 1.000000000000000000),
 ( 0.3333333333333335369, 0.3333333333333330373),
 ( 0.3333333333333335369, 0.3333333333333330373),
 ( 1.000000000000000000, 1.000000000000000000),
 ( 0.3333333333333333703, 0.3333333333333333703),
 ( 0.3333333333333333703, 0.3333333333333333703),
 ( 1.000000000000000000, 1.000000000000000000) ) ) 
 REPRESENTATION_ITEM ( '' )  SURFACE ( )  );
#534 = CARTESIAN_POINT ( 'NONE',  ( -12.04615335961045908, -19.96505441190284813, 61.53645242954323891 ) ) ;
#535 = CARTESIAN_POINT ( 'NONE',  ( -11.41043474416280823, -19.20696576352171903, 71.80969020189922958 ) ) ;
#536 = CARTESIAN_POINT ( 'NONE',  ( -13.14551704304688684, -16.75068433397604295, 49.52966884056655772 ) ) ;
#537 = CARTESIAN_POINT ( 'NONE',  ( -24.38600087812161377, -15.53966288334215307, 73.00303710413747638 ) ) ;
#538 = EDGE_CURVE ( 'NONE', #30207, #6304, #36209, .T. ) ;
#539 = CARTESIAN_POINT ( 'NONE',  ( -14.48548941065489970, -8.400516866317895293, 67.27447142263336843 ) ) ;
#540 = CARTESIAN_POINT ( 'NONE',  ( -24.17882124642622088, -12.77733483093900091, 73.54225673225543858 ) ) ;
#541 = PLANE ( 'NONE',  #23265 ) ;
#542 = CARTESIAN_POINT ( 'NONE',  ( -12.77099621783261263, -20.03938943333788814, 71.82270288656182800 ) ) ;
#543 = CARTESIAN_POINT ( 'NONE',  ( -17.42409385541300182, -14.80920654474440745, 53.27966884056655061 ) ) ;
#544 =( BOUNDED_CURVE ( )  B_SPLINE_CURVE ( 3, ( #29925, #40748, #21791, #48141 ),
 .UNSPECIFIED., .F., .F. ) 
 B_SPLINE_CURVE_WITH_KNOTS ( ( 4, 4 ),
 ( 0.000000000000000000, 0.4074455897393696180 ),
 .UNSPECIFIED. ) 
 CURVE ( )  GEOMETRIC_REPRESENTATION_ITEM ( )  RATIONAL_B_SPLINE_CURVE ( ( 1.000000000000000000, 0.4567392136813236969, 0.3561768502900272138, 0.6983129098261106060 ) ) 
 REPRESENTATION_ITEM ( '' )  );
#545 = VERTEX_POINT ( 'NONE', #33927 ) ;
#546 = VECTOR ( 'NONE', #17475, 1000.000000000000000 ) ;
#547 = ORIENTED_EDGE ( 'NONE', *, *, #3362, .T. ) ;
#548 = AXIS2_PLACEMENT_3D ( 'NONE', #12878, #27906, #42931 ) ;
#549 = CARTESIAN_POINT ( 'NONE',  ( -22.41159385650551528, -6.922745924619793101, 51.69366785382590024 ) ) ;
#550 = EDGE_CURVE ( 'NONE', #44867, #2342, #18143, .T. ) ;
#551 = ORIENTED_EDGE ( 'NONE', *, *, #1678, .F. ) ;
#552 = CARTESIAN_POINT ( 'NONE',  ( -11.71665266943325534, -18.96132379659194100, 64.90273906658698877 ) ) ;
#553 = EDGE_CURVE ( 'NONE', #43090, #13641, #7363, .T. ) ;
#554 = CARTESIAN_POINT ( 'NONE',  ( -16.53261792465593771, -21.75226837608146369, 61.82856087129801637 ) ) ;
#555 = VECTOR ( 'NONE', #30468, 1000.000000000000000 ) ;
#556 = ADVANCED_FACE ( 'NONE', ( #40403 ), #3646, .T. ) ;
#557 = CARTESIAN_POINT ( 'NONE',  ( -12.84690951644825851, -8.931012861620404308, 67.56438176077992352 ) ) ;
#558 = CARTESIAN_POINT ( 'NONE',  ( -16.15628411965152722, -22.15059256196195037, 58.47859698976697729 ) ) ;
#559 = EDGE_CURVE ( 'NONE', #47460, #43020, #7166, .T. ) ;
#560 = ORIENTED_EDGE ( 'NONE', *, *, #10649, .F. ) ;
#561 = B_SPLINE_CURVE_WITH_KNOTS ( 'NONE', 3,
 ( #45712, #8272, #26976, #30926, #4564, #8764, #34595, #879, #15881, #45938 ),
 .UNSPECIFIED., .F., .F.,
 ( 4, 2, 2, 2, 4 ),
 ( 0.6272669072877743446, 0.7522669073072931756, 0.8772669073268121176, 1.002266907346331060, 1.127266907365849891 ),
 .UNSPECIFIED. ) ;
#562 = CARTESIAN_POINT ( 'NONE',  ( -20.95714566783631483, -8.250050064981410358, 60.00271774409104353 ) ) ;
#563 = CARTESIAN_POINT ( 'NONE',  ( -17.57575749508838925, -7.360700902354934350, 63.65718735946740736 ) ) ;
#564 = EDGE_LOOP ( 'NONE', ( #27318, #12069 ) ) ;
#565 = DIRECTION ( 'NONE',  ( 0.5420872618288284928, 0.8403222004463034578, -7.592316861453148064E-08 ) ) ;
#566 = VERTEX_POINT ( 'NONE', #10386 ) ;
#567 = CARTESIAN_POINT ( 'NONE',  ( -11.14114473067313682, -10.80566704772025233, 57.32407823191172014 ) ) ;
#568 = DIRECTION ( 'NONE',  ( -0.000000000000000000, 0.000000000000000000, 1.000000000000000000 ) ) ;
#569 = CARTESIAN_POINT ( 'NONE',  ( -12.37350074511489595, -12.59798860466149861, 53.69233794759168887 ) ) ;
#570 = EDGE_LOOP ( 'NONE', ( #41024, #28488, #8043, #46149 ) ) ;
#571 = CARTESIAN_POINT ( 'NONE',  ( -19.66015584026798280, -21.44380816191627659, 69.00652708242157019 ) ) ;
#572 = CARTESIAN_POINT ( 'NONE',  ( -11.77150565662344484, -19.02841119382535950, 68.42509345399683696 ) ) ;
#573 = CARTESIAN_POINT ( 'NONE',  ( -14.56525312440409081, -21.68886035253952116, 58.36629080999882291 ) ) ;
#574 = DIRECTION ( 'NONE',  ( -1.000000000000000000, -1.669677910507523057E-21, -6.493791346278465266E-22 ) ) ;
#575 = VERTEX_POINT ( 'NONE', #221 ) ;
#576 = DIRECTION ( 'NONE',  ( -3.071710424422018668E-17, 6.404604876783312462E-16, 1.000000000000000000 ) ) ;
#577 = DIRECTION ( 'NONE',  ( 3.413470714839332458E-33, -1.190614954331866791E-16, 1.000000000000000000 ) ) ;
#578 = AXIS2_PLACEMENT_3D ( 'NONE', #35667, #10320, #47006 ) ;
#579 = FACE_OUTER_BOUND ( 'NONE', #40950, .T. ) ;
#580 = CYLINDRICAL_SURFACE ( 'NONE', #31369, 0.1499999999999984401 ) ;
#581 = DIRECTION ( 'NONE',  ( -1.000000000000000000, -2.866981220435666553E-17, -0.000000000000000000 ) ) ;
#582 = CARTESIAN_POINT ( 'NONE',  ( -21.45534385650551812, -7.417179338643134834, 52.18511593390279302 ) ) ;
#583 = ORIENTED_EDGE ( 'NONE', *, *, #25130, .F. ) ;
#584 = CARTESIAN_POINT ( 'NONE',  ( -15.11195830621016256, -21.41632612911037370, 65.40596681519618016 ) ) ;
#585 = CARTESIAN_POINT ( 'NONE',  ( -24.28035819322802880, -16.22076492358945998, 59.35005677771162880 ) ) ;
#586 = ORIENTED_EDGE ( 'NONE', *, *, #6608, .F. ) ;
#587 = CARTESIAN_POINT ( 'NONE',  ( -17.19980194945414809, -7.762775306501539241, 70.64035839668011363 ) ) ;
#588 = VECTOR ( 'NONE', #14745, 1000.000000000000114 ) ;
#589 = FACE_OUTER_BOUND ( 'NONE', #44283, .T. ) ;
#590 = DIRECTION ( 'NONE',  ( -0.6105870317843966610, -0.7919491628991827126, 6.540688078712155195E-08 ) ) ;
#591 = EDGE_CURVE ( 'NONE', #27215, #5198, #21725, .T. ) ;
#592 = ORIENTED_EDGE ( 'NONE', *, *, #8079, .F. ) ;
#593 = CARTESIAN_POINT ( 'NONE',  ( -10.37857782286507025, -14.46928323978489317, 71.62782678106509593 ) ) ;
#594 = CARTESIAN_POINT ( 'NONE',  ( -10.43972881942000086, -15.77115500203794873, 64.52243715390834211 ) ) ;
#595 = DIRECTION ( 'NONE',  ( -3.071710424422018668E-17, 6.404604876783312462E-16, 1.000000000000000000 ) ) ;
#596 = VERTEX_POINT ( 'NONE', #40174 ) ;
#597 = CARTESIAN_POINT ( 'NONE',  ( -15.49284385650551776, -7.406986770994973490, 48.81910596585309747 ) ) ;
#598 = CARTESIAN_POINT ( 'NONE',  ( -24.14981099001045095, -11.60321323961852258, 59.59580478148293992 ) ) ;
#599 = CARTESIAN_POINT ( 'NONE',  ( -17.42409385541299471, -14.80920654474435771, 49.52966884056655772 ) ) ;
#600 = DIRECTION ( 'NONE',  ( -3.071710424422018668E-17, 6.404604876783312462E-16, 1.000000000000000000 ) ) ;
#601 = CARTESIAN_POINT ( 'NONE',  ( -9.424093855413051557, -27.10920654474410796, 78.99999999999998579 ) ) ;
#602 = ORIENTED_EDGE ( 'NONE', *, *, #29857, .F. ) ;
#603 = EDGE_LOOP ( 'NONE', ( #36733, #18281 ) ) ;
#604 = CARTESIAN_POINT ( 'NONE',  ( -14.34284385650551563, -8.811426318492348031, 52.18089403414752070 ) ) ;
#605 = DIRECTION ( 'NONE',  ( -5.731567514496413899E-31, -1.020425574103664789E-16, -1.000000000000000000 ) ) ;
#606 = ADVANCED_FACE ( 'NONE', ( #47562 ), #26776, .T. ) ;
#607 = CARTESIAN_POINT ( 'NONE',  ( -10.45137630651438698, -14.19109027996143801, 61.20355913676015547 ) ) ;
#608 = LINE ( 'NONE', #7525, #26051 ) ;
#609 = EDGE_CURVE ( 'NONE', #19293, #40234, #36450, .T. ) ;
#610 = AXIS2_PLACEMENT_3D ( 'NONE', #22135, #10795, #30262 ) ;
#611 = CIRCLE ( 'NONE', #9265, 4.686499999999997890 ) ;
#612 = EDGE_CURVE ( 'NONE', #42866, #14276, #37609, .T. ) ;
#613 = CARTESIAN_POINT ( 'NONE',  ( -20.35208293893518672, -8.450992964911224092, 67.08104082230126153 ) ) ;
#614 = DIRECTION ( 'NONE',  ( -1.000000000000000000, 0.000000000000000000, 0.000000000000000000 ) ) ;
#615 =( BOUNDED_CURVE ( )  B_SPLINE_CURVE ( 3, ( #7951, #41907, #8185, #539 ),
 .UNSPECIFIED., .F., .F. ) 
 B_SPLINE_CURVE_WITH_KNOTS ( ( 4, 4 ),
 ( 0.4074455897393645665, 0.5000000000000000000 ),
 .UNSPECIFIED. ) 
 CURVE ( )  GEOMETRIC_REPRESENTATION_ITEM ( )  RATIONAL_B_SPLINE_CURVE ( ( 0.6983129098261017242, 0.7760317562606843245, 0.8765941196519773104, 0.9999999999999659162 ) ) 
 REPRESENTATION_ITEM ( '' )  );
#616 = AXIS2_PLACEMENT_3D ( 'NONE', #41938, #33542, #44666 ) ;
#617 = CYLINDRICAL_SURFACE ( 'NONE', #6832, 0.1500000000000042966 ) ;
#618 = EDGE_CURVE ( 'NONE', #14550, #43562, #17736, .T. ) ;
#619 = EDGE_LOOP ( 'NONE', ( #6254, #15796, #31967, #18011, #32295 ) ) ;
#620 = CARTESIAN_POINT ( 'NONE',  ( -9.927469056236301270, -15.37997598727726611, 54.02312124697527906 ) ) ;
#621 = AXIS2_PLACEMENT_3D ( 'NONE', #36417, #14242, #14973 ) ;
#622 = ORIENTED_EDGE ( 'NONE', *, *, #12533, .F. ) ;
#623 = CARTESIAN_POINT ( 'NONE',  ( -13.22529448846758804, -9.145569705956512863, 64.19474388871357462 ) ) ;
#624 = CARTESIAN_POINT ( 'NONE',  ( -9.975093145215874202, -14.93635225021824198, 74.98274299234972773 ) ) ;
#625 = CARTESIAN_POINT ( 'NONE',  ( -19.11145557798581152, -7.964112677450091660, 63.73089235102099792 ) ) ;
#626 = CARTESIAN_POINT ( 'NONE',  ( -18.11514229927295716, -22.22721396694290164, 65.46815266832128088 ) ) ;
#627 = ORIENTED_EDGE ( 'NONE', *, *, #4548, .T. ) ;
#628 = CARTESIAN_POINT ( 'NONE',  ( -10.78967749848787427, -12.41559940729129785, 61.21342246320382685 ) ) ;
#629 = DIRECTION ( 'NONE',  ( -2.866981220435666553E-17, 1.000000000000000000, 1.190614954331866791E-16 ) ) ;
#630 = CARTESIAN_POINT ( 'NONE',  ( -22.09908899289463591, -14.48102562737866528, 52.02966884056656482 ) ) ;
#631 = CARTESIAN_POINT ( 'NONE',  ( -19.36518065869528726, -8.031383756764064685, 59.97565108339750850 ) ) ;
#632 = ORIENTED_EDGE ( 'NONE', *, *, #1271, .F. ) ;
#633 = CARTESIAN_POINT ( 'NONE',  ( -18.30602013973305020, -21.80685202924323463, 72.69999788315199396 ) ) ;
#634 = DIRECTION ( 'NONE',  ( -1.927470528863183637E-16, -1.434740771370715221E-29, 1.000000000000000000 ) ) ;
#635 = DIRECTION ( 'NONE',  ( 0.000000000000000000, 0.000000000000000000, 1.000000000000000000 ) ) ;
#636 = DIRECTION ( 'NONE',  ( -0.3478314405900309603, -0.9375570856950864451, 0.000000000000000000 ) ) ;
#637 = ORIENTED_EDGE ( 'NONE', *, *, #2970, .F. ) ;
#638 = CARTESIAN_POINT ( 'NONE',  ( -22.15985579531568916, -19.96414753270404674, 62.46112518014844284 ) ) ;
#639 = CARTESIAN_POINT ( 'NONE',  ( -15.32718698399739132, -9.710093178977245998, 53.88362224778187226 ) ) ;
#640 = CARTESIAN_POINT ( 'NONE',  ( -12.27729947935473476, -9.991218615320081042, 60.85918086709605745 ) ) ;
#641 = AXIS2_PLACEMENT_3D ( 'NONE', #12908, #32598, #42958 ) ;
#642 = CARTESIAN_POINT ( 'NONE',  ( -15.88847107554206062, -7.518423027132939751, 63.78355628068795369 ) ) ;
#643 = ORIENTED_EDGE ( 'NONE', *, *, #45775, .F. ) ;
#644 = CARTESIAN_POINT ( 'NONE',  ( -10.53028993777715883, -16.28642212234895226, 71.73278239416407587 ) ) ;
#645 = ORIENTED_EDGE ( 'NONE', *, *, #35314, .F. ) ;
#646 = CIRCLE ( 'NONE', #21865, 5.249999999999998224 ) ;
#647 = CARTESIAN_POINT ( 'NONE',  ( -17.85555652284939043, -7.772123375420258107, 60.09532845646905486 ) ) ;
#648 = CARTESIAN_POINT ( 'NONE',  ( -22.97806213383195484, -10.54588184283626262, 63.18259140678883767 ) ) ;
#649 = EDGE_CURVE ( 'NONE', #8229, #44349, #41798, .T. ) ;
#650 = ORIENTED_EDGE ( 'NONE', *, *, #25310, .T. ) ;
#651 = VECTOR ( 'NONE', #27035, 1000.000000000000000 ) ;
#652 = CIRCLE ( 'NONE', #36779, 1.999999999999994893 ) ;
#653 = LINE ( 'NONE', #19120, #11762 ) ;
#654 = ORIENTED_EDGE ( 'NONE', *, *, #8134, .F. ) ;
#655 = ORIENTED_EDGE ( 'NONE', *, *, #42876, .F. ) ;
#656 = VERTEX_POINT ( 'NONE', #26546 ) ;
#657 = CARTESIAN_POINT ( 'NONE',  ( -17.98584054083101691, -22.23808389992613499, 62.06031238270200845 ) ) ;
#658 = VECTOR ( 'NONE', #26141, 1000.000000000000114 ) ;
#659 = LINE ( 'NONE', #18884, #6970 ) ;
#660 = CARTESIAN_POINT ( 'NONE',  ( -43.16186218120491702, -14.90920654474411577, 57.09785339366514734 ) ) ;
#661 = CARTESIAN_POINT ( 'NONE',  ( -24.13556280029956724, -12.81997495155604483, 66.52920008143310326 ) ) ;
#662 = CARTESIAN_POINT ( 'NONE',  ( -11.81594133544200709, -9.904820009267291780, 64.20631235510137458 ) ) ;
#663 = EDGE_CURVE ( 'NONE', #29482, #47620, #41570, .T. ) ;
#664 = DIRECTION ( 'NONE',  ( 0.8565259173193583431, -0.5161040137028850561, 6.301967848571307172E-08 ) ) ;
#665 = ORIENTED_EDGE ( 'NONE', *, *, #5113, .F. ) ;
#666 = ORIENTED_EDGE ( 'NONE', *, *, #47788, .F. ) ;
#667 = ADVANCED_FACE ( 'NONE', ( #34162 ), #31558, .T. ) ;
#668 = CARTESIAN_POINT ( 'NONE',  ( -12.77013062424865630, -8.927826924028671840, 54.27966884056655061 ) ) ;
#669 = DIRECTION ( 'NONE',  ( -1.000000000000000000, 0.000000000000000000, 0.000000000000000000 ) ) ;
#670 = CARTESIAN_POINT ( 'NONE',  ( -23.62338436797153918, -18.94230004192412409, 69.48027381658378943 ) ) ;
#671 = ORIENTED_EDGE ( 'NONE', *, *, #10542, .F. ) ;
#672 =( BOUNDED_CURVE ( )  B_SPLINE_CURVE ( 3, ( #30748, #35382, #4629, #16422 ),
 .UNSPECIFIED., .F., .F. ) 
 B_SPLINE_CURVE_WITH_KNOTS ( ( 4, 4 ),
 ( 0.000000000000000000, 0.4074455897393622905 ),
 .UNSPECIFIED. ) 
 CURVE ( )  GEOMETRIC_REPRESENTATION_ITEM ( )  RATIONAL_B_SPLINE_CURVE ( ( 1.000000000000000000, 0.4567392136813403503, 0.3561768502900334310, 0.6983129098260791867 ) ) 
 REPRESENTATION_ITEM ( '' )  );
#673 = CARTESIAN_POINT ( 'NONE',  ( -15.83034385650551634, -9.794322478646142471, 51.19202720610083901 ) ) ;
#674 = ORIENTED_EDGE ( 'NONE', *, *, #17450, .F. ) ;
#675 = EDGE_CURVE ( 'NONE', #38177, #26989, #12019, .T. ) ;
#676 = DIRECTION ( 'NONE',  ( -3.071710424422018668E-17, 6.404604876783312462E-16, 1.000000000000000000 ) ) ;
#677 = CARTESIAN_POINT ( 'NONE',  ( -10.47203305924008632, -16.00180800482426235, 71.53930669669551889 ) ) ;
#678 = AXIS2_PLACEMENT_3D ( 'NONE', #4820, #19589, #20074 ) ;
#680 = CARTESIAN_POINT ( 'NONE',  ( -13.43921569888383694, -8.993430976374535035, 60.58950277493168812 ) ) ;
#679 = B_SPLINE_CURVE_WITH_KNOTS ( 'NONE', 3,
 ( #24698, #25641, #33011, #47812, #14293, #21236, #32326, #29343, #28392, #40655 ),
 .UNSPECIFIED., .F., .F.,
 ( 4, 2, 2, 2, 4 ),
 ( 0.000000000000000000, 0.2500000000000000000, 0.5000000000000000000, 0.7500000000000000000, 1.000000000000000000 ),
 .UNSPECIFIED. ) ;
#681 = EDGE_CURVE ( 'NONE', #47374, #501, #32348, .T. ) ;
#682 = PRESENTATION_LAYER_ASSIGNMENT (  '', '', ( #3018 ) ) ;
#683 = ORIENTED_EDGE ( 'NONE', *, *, #38447, .F. ) ;
#684 = CARTESIAN_POINT ( 'NONE',  ( -18.50931870666621037, -21.77518001355031529, 72.28510940651260341 ) ) ;
#685 =( BOUNDED_CURVE ( )  B_SPLINE_CURVE ( 3, ( #11024, #29002, #44052, #44773 ),
 .UNSPECIFIED., .F., .F. ) 
 B_SPLINE_CURVE_WITH_KNOTS ( ( 4, 4 ),
 ( 0.4074455897393601256, 0.5000000000000000000 ),
 .UNSPECIFIED. ) 
 CURVE ( )  GEOMETRIC_REPRESENTATION_ITEM ( )  RATIONAL_B_SPLINE_CURVE ( ( 0.6983129098260726364, 0.7760317562606952047, 0.8765941196520086187, 1.000000000000023093 ) ) 
 REPRESENTATION_ITEM ( '' )  );
#686 = AXIS2_PLACEMENT_3D ( 'NONE', #14516, #18238, #33745 ) ;
#687 = AXIS2_PLACEMENT_3D ( 'NONE', #47065, #9654, #39670 ) ;
#688 = FACE_OUTER_BOUND ( 'NONE', #15519, .T. ) ;
#689 = CARTESIAN_POINT ( 'NONE',  ( -17.02409385541305298, -14.80920654474411080, 47.99999999999997868 ) ) ;
#690 = ORIENTED_EDGE ( 'NONE', *, *, #34751, .F. ) ;
#691 = AXIS2_PLACEMENT_3D ( 'NONE', #27217, #8045, #38779 ) ;
#692 = CARTESIAN_POINT ( 'NONE',  ( -24.87290000513101873, -14.67112934921935974, 62.82801050733710468 ) ) ;
#693 = ADVANCED_FACE ( 'NONE', ( #1401 ), #695, .F. ) ;
#694 = CARTESIAN_POINT ( 'NONE',  ( -22.47468696571113256, -17.02042448482726300, 53.69233794759168887 ) ) ;
#695 = PLANE ( 'NONE',  #46507 ) ;
#696 = ORIENTED_EDGE ( 'NONE', *, *, #27077, .F. ) ;
#697 = CARTESIAN_POINT ( 'NONE',  ( -11.12358174778395714, -11.75903488045733347, 71.38860871064898106 ) ) ;
#698 = EDGE_CURVE ( 'NONE', #20557, #17825, #15830, .T. ) ;
#699 =( BOUNDED_SURFACE ( )  B_SPLINE_SURFACE ( 3, 1, ( 
 ( #9049, #1648 ),
 ( #43268, #35371 ),
 ( #31689, #46714 ),
 ( #27984, #43009 ),
 ( #5601, #26605 ),
 ( #35609, #1886 ),
 ( #31927, #24558 ) ),
 .UNSPECIFIED., .T., .F., .F. ) 
 B_SPLINE_SURFACE_WITH_KNOTS ( ( 4, 3, 4 ),
 ( 2, 2 ),
 ( 0.000000000000000000, 0.5000000000000000000, 1.000000000000000000 ),
 ( 0.000000000000000000, 1.000000000000000000 ),
 .UNSPECIFIED. ) 
 GEOMETRIC_REPRESENTATION_ITEM ( )  RATIONAL_B_SPLINE_SURFACE ( (
 ( 1.000000000000000000, 1.000000000000000000),
 ( 0.3333333333333335369, 0.3333333333333330373),
 ( 0.3333333333333335369, 0.3333333333333330373),
 ( 1.000000000000000000, 1.000000000000000000),
 ( 0.3333333333333333703, 0.3333333333333333703),
 ( 0.3333333333333333703, 0.3333333333333333703),
 ( 1.000000000000000000, 1.000000000000000000) ) ) 
 REPRESENTATION_ITEM ( '' )  SURFACE ( )  );
#700 = VERTEX_POINT ( 'NONE', #42551 ) ;
#701 = CARTESIAN_POINT ( 'NONE',  ( -18.22409385759798894, -9.359200813967568422, 50.49621490985803263 ) ) ;
#702 = ORIENTED_EDGE ( 'NONE', *, *, #13629, .T. ) ;
#703 = ADVANCED_FACE ( 'NONE', ( #935 ), #12739, .T. ) ;
#704 = CARTESIAN_POINT ( 'NONE',  ( -16.59509239138002101, -21.81331869282671221, 61.64079261740195648 ) ) ;
#705 = CARTESIAN_POINT ( 'NONE',  ( -15.18259368501833784, -19.55664553709809539, 52.02966884056656482 ) ) ;
#706 = PLANE ( 'NONE',  #16311 ) ;
#707 = ORIENTED_EDGE ( 'NONE', *, *, #43794, .F. ) ;
#708 = LINE ( 'NONE', #44800, #84 ) ;
#709 = LINE ( 'NONE', #30519, #41682 ) ;
#710 = CARTESIAN_POINT ( 'NONE',  ( -24.69852204723760281, -16.41745771733451775, 59.30827817708741634 ) ) ;
#711 = ORIENTED_EDGE ( 'NONE', *, *, #23137, .T. ) ;
#712 = CARTESIAN_POINT ( 'NONE',  ( -14.97188219925329378, -8.199429090594037461, 56.84999999999995168 ) ) ;
#713 = CARTESIAN_POINT ( 'NONE',  ( -12.76547314785493192, -9.517330534081262172, 74.60450883341005124 ) ) ;
#714 = ORIENTED_EDGE ( 'NONE', *, *, #34422, .F. ) ;
#715 = ORIENTED_EDGE ( 'NONE', *, *, #7569, .F. ) ;
#716 = DIRECTION ( 'NONE',  ( 0.9687793358424819923, -0.2479245821708680464, 0.000000000000000000 ) ) ;
#717 = CARTESIAN_POINT ( 'NONE',  ( -19.34909385759798894, -8.112991634885936776, 51.74999426922421719 ) ) ;
#719 = DIRECTION ( 'NONE',  ( 0.9524241471993249997, 0.0009228828802128017121, -0.3047743298226210928 ) ) ;
#718 = AXIS2_PLACEMENT_3D ( 'NONE', #30330, #289, #34963 ) ;
#720 = CARTESIAN_POINT ( 'NONE',  ( -22.07409385650551670, -9.792211528768504536, 50.49490371617623197 ) ) ;
#721 = CARTESIAN_POINT ( 'NONE',  ( -24.72409385541305582, -14.80920654474417830, 64.04117647058822627 ) ) ;
#722 = ORIENTED_EDGE ( 'NONE', *, *, #23758, .T. ) ;
#723 = CARTESIAN_POINT ( 'NONE',  ( -11.68391713028079515, -10.70246380009546527, 71.12460117624890188 ) ) ;
#724 = CARTESIAN_POINT ( 'NONE',  ( -23.28150499554093500, -18.64225713161144782, 69.29372035757846504 ) ) ;
#725 = AXIS2_PLACEMENT_3D ( 'NONE', #31292, #46326, #12580 ) ;
#726 = VECTOR ( 'NONE', #11983, 1000.000000000000000 ) ;
#727 = CARTESIAN_POINT ( 'NONE',  ( -11.13733870171179596, -11.61806121328042174, 67.90392505421056057 ) ) ;
#728 = ORIENTED_EDGE ( 'NONE', *, *, #17278, .F. ) ;
#729 = CARTESIAN_POINT ( 'NONE',  ( -22.52972399543339677, -9.943266245822872662, 69.89689837695897268 ) ) ;
#730 = VECTOR ( 'NONE', #22079, 1000.000000000000000 ) ;
#731 = CARTESIAN_POINT ( 'NONE',  ( -10.03104929242693544, -13.88935366066504251, 57.55486709734128681 ) ) ;
#732 = CARTESIAN_POINT ( 'NONE',  ( -50.42609385541305755, -14.90920654474416907, 63.03529411764704804 ) ) ;
#733 = VERTEX_POINT ( 'NONE', #8821 ) ;
#734 = ORIENTED_EDGE ( 'NONE', *, *, #46518, .T. ) ;
#735 = EDGE_CURVE ( 'NONE', #35067, #41098, #33494, .T. ) ;
#736 = CARTESIAN_POINT ( 'NONE',  ( -20.54979492810923603, -8.489990406890694175, 63.46121512946601229 ) ) ;
#737 = DIRECTION ( 'NONE',  ( -2.866981220435666553E-17, 1.000000000000000000, 1.190614954331866791E-16 ) ) ;
#738 = CARTESIAN_POINT ( 'NONE',  ( -50.42609385541305755, -14.90920654474420104, 66.95294117647057419 ) ) ;
#739 = CARTESIAN_POINT ( 'NONE',  ( -10.16925234506895670, -13.11493237325164429, 71.40102718425720241 ) ) ;
#740 = ORIENTED_EDGE ( 'NONE', *, *, #28298, .F. ) ;
#741 = CARTESIAN_POINT ( 'NONE',  ( -23.53718313364170456, -11.39868142885006641, 69.89210781356229063 ) ) ;
#742 = CARTESIAN_POINT ( 'NONE',  ( -21.95370832667365235, -13.56094844357179774, 49.52966884056655772 ) ) ;
#743 = DIRECTION ( 'NONE',  ( 0.9687793358424819923, -0.2479245821708680464, 0.000000000000000000 ) ) ;
#744 = VERTEX_POINT ( 'NONE', #45770 ) ;
#745 = VECTOR ( 'NONE', #8958, 1000.000000000000000 ) ;
#746 = CARTESIAN_POINT ( 'NONE',  ( -12.93303430567921808, -20.17867969065821399, 72.03327057247898324 ) ) ;
#747 = CARTESIAN_POINT ( 'NONE',  ( -14.01837044221388595, -8.636059239884618322, 74.48482605064899076 ) ) ;
#748 = VERTEX_POINT ( 'NONE', #46232 ) ;
#749 = CARTESIAN_POINT ( 'NONE',  ( -12.74802523442671465, -20.09592109768945889, 65.02242199588995675 ) ) ;
#750 = AXIS2_PLACEMENT_3D ( 'NONE', #47534, #36184, #14476 ) ;
#751 = AXIS2_PLACEMENT_3D ( 'NONE', #19117, #9016, #23303 ) ;
#752 = EDGE_CURVE ( 'NONE', #21025, #27231, #29425, .T. ) ;
#753 = EDGE_LOOP ( 'NONE', ( #38139, #35733, #34548, #4648, #26737 ) ) ;
#754 = DIRECTION ( 'NONE',  ( 0.4461977533473615032, -0.8949343913984796339, 0.000000000000000000 ) ) ;
#755 = CARTESIAN_POINT ( 'NONE',  ( -11.17842666812006769, -10.74653426074781848, 57.39558607234117460 ) ) ;
#756 = EDGE_LOOP ( 'NONE', ( #42117, #32142, #13196, #23124 ) ) ;
#757 = DIRECTION ( 'NONE',  ( -1.000000000000000000, -2.866981220435666553E-17, 0.000000000000000000 ) ) ;
#758 = ADVANCED_FACE ( 'NONE', ( #8328 ), #38334, .T. ) ;
#759 = EDGE_CURVE ( 'NONE', #33339, #19087, #2389, .T. ) ;
#760 = FACE_OUTER_BOUND ( 'NONE', #17758, .T. ) ;
#761 = CARTESIAN_POINT ( 'NONE',  ( -18.50534385650551528, -8.801233750844183135, 48.81488406609782515 ) ) ;
#762 = CARTESIAN_POINT ( 'NONE',  ( -24.47161816259883338, -14.62087121170030635, 63.01296490870000611 ) ) ;
#763 = CARTESIAN_POINT ( 'NONE',  ( -10.52750029887962491, -17.62704889381915407, 68.29060234424891007 ) ) ;
#764 = CARTESIAN_POINT ( 'NONE',  ( -24.72409385541305582, -14.80920654474425291, 71.98235294117645822 ) ) ;
#765 = ORIENTED_EDGE ( 'NONE', *, *, #18837, .F. ) ;
#766 = CARTESIAN_POINT ( 'NONE',  ( -10.43360882127813838, -14.44320667503941458, 64.46091912948344316 ) ) ;
#767 = CARTESIAN_POINT ( 'NONE',  ( -16.44909385541304303, -8.112991634885936776, 51.74999426922421719 ) ) ;
#768 = CARTESIAN_POINT ( 'NONE',  ( -15.77409385541301035, -6.859212275519753099, 50.50378509014291240 ) ) ;
#769 = DIRECTION ( 'NONE',  ( 2.654446662475610288E-06, -3.134491601460476904E-06, 0.9999999999915645255 ) ) ;
#770 = CARTESIAN_POINT ( 'NONE',  ( -24.76424570620368115, -16.08454870407971882, 66.24137714576976066 ) ) ;
#772 = ORIENTED_EDGE ( 'NONE', *, *, #31833, .F. ) ;
#771 = VECTOR ( 'NONE', #3922, 1000.000000000000000 ) ;
#773 = VERTEX_POINT ( 'NONE', #35134 ) ;
#774 = CARTESIAN_POINT ( 'NONE',  ( -21.40187103850036721, -9.048701367307623755, 73.61745452359328112 ) ) ;
#775 = CARTESIAN_POINT ( 'NONE',  ( -6.424093855413058662, -6.359206544744109735, 54.49999999999999289 ) ) ;
#776 = ORIENTED_EDGE ( 'NONE', *, *, #46959, .F. ) ;
#777 = CARTESIAN_POINT ( 'NONE',  ( -20.99713037368098156, -21.34662133218488833, 62.23754514806859817 ) ) ;
#778 = CARTESIAN_POINT ( 'NONE',  ( -15.08687585379459506, -21.46369733121157708, 68.99081615631787656 ) ) ;
#779 = CARTESIAN_POINT ( 'NONE',  ( -20.98034385759799392, -9.360768649639302552, 51.01397948905921709 ) ) ;
#780 = CARTESIAN_POINT ( 'NONE',  ( -24.73909915436057716, -16.22127400844152234, 62.69990344863494869 ) ) ;
#781 = CARTESIAN_POINT ( 'NONE',  ( -24.38811233016677704, -14.09928486418781901, 73.42271532469474948 ) ) ;
#782 = CARTESIAN_POINT ( 'NONE',  ( -11.19706266256277694, -11.50303319689152914, 67.63336710488009373 ) ) ;
#783 = CARTESIAN_POINT ( 'NONE',  ( -13.96760974046062920, -8.722112190022174971, 74.39057940708781302 ) ) ;
#784 = VERTEX_POINT ( 'NONE', #9055 ) ;
#785 = CARTESIAN_POINT ( 'NONE',  ( -12.23301264461619553, -10.03852782535897958, 60.84446034103241630 ) ) ;
#786 = EDGE_CURVE ( 'NONE', #31226, #12218, #6500, .T. ) ;
#787 = CARTESIAN_POINT ( 'NONE',  ( -17.42409385541299471, -14.80920654474435594, 52.02966884056656482 ) ) ;
#788 = CARTESIAN_POINT ( 'NONE',  ( -13.71338950266841472, -20.80363499509022773, 64.98628881289567971 ) ) ;
#789 = DIRECTION ( 'NONE',  ( 0.5327540375067997269, 0.8462701315302331162, 7.203825861310633201E-08 ) ) ;
#790 = PLANE ( 'NONE',  #17368 ) ;
#791 = VECTOR ( 'NONE', #36841, 1000.000000000000000 ) ;
#792 = ORIENTED_EDGE ( 'NONE', *, *, #5799, .F. ) ;
#793 = EDGE_LOOP ( 'NONE', ( #35327, #32327, #24506, #37244, #18270 ) ) ;
#794 = CARTESIAN_POINT ( 'NONE',  ( -20.10179291524702805, -21.76144317846600629, 72.66124644823618439 ) ) ;
#795 = EDGE_LOOP ( 'NONE', ( #9092, #33098, #976, #11055, #17567 ) ) ;
#796 = CARTESIAN_POINT ( 'NONE',  ( -23.31159385541299756, -8.990409506049253707, 49.61344411288070688 ) ) ;
#797 = EDGE_CURVE ( 'NONE', #30726, #47586, #41867, .T. ) ;
#798 = CARTESIAN_POINT ( 'NONE',  ( -10.47387877723939731, -13.58059689071059495, 57.59258137113961595 ) ) ;
#799 = AXIS2_PLACEMENT_3D ( 'NONE', #38007, #22270, #37510 ) ;
#800 = CARTESIAN_POINT ( 'NONE',  ( -16.23116076413911557, -7.455249184188991407, 60.31533086125586607 ) ) ;
#801 = CARTESIAN_POINT ( 'NONE',  ( -13.38659385759799214, -7.222650657624104298, 49.61879703869476543 ) ) ;
#802 = CARTESIAN_POINT ( 'NONE',  ( -17.91716493482169525, -7.374790294242734134, 60.26716059546817661 ) ) ;
#803 = EDGE_LOOP ( 'NONE', ( #15438, #5843, #2592, #2224 ) ) ;
#804 = DIRECTION ( 'NONE',  ( -3.071710424422018668E-17, 6.404604876783312462E-16, 1.000000000000000000 ) ) ;
#805 = ORIENTED_EDGE ( 'NONE', *, *, #5345, .T. ) ;
#806 = CARTESIAN_POINT ( 'NONE',  ( -18.39951368268757648, -22.19516171751901368, 69.00010101991060196 ) ) ;
#807 = CARTESIAN_POINT ( 'NONE',  ( -13.82689732469268407, -20.87277619789260186, 68.47097268802275494 ) ) ;
#808 = ORIENTED_EDGE ( 'NONE', *, *, #15982, .F. ) ;
#809 = DIRECTION ( 'NONE',  ( 0.9687793358424821033, -0.2479245821708679909, 0.000000000000000000 ) ) ;
#810 = CARTESIAN_POINT ( 'NONE',  ( -16.78181722113097152, -22.23154757984593388, 68.73914717078854153 ) ) ;
#811 = CARTESIAN_POINT ( 'NONE',  ( -17.15134030326023051, -7.364115279526828317, 70.67531275522621570 ) ) ;
#812 = EDGE_LOOP ( 'NONE', ( #12953, #5812, #37264, #19449 ) ) ;
#813 = EDGE_CURVE ( 'NONE', #22280, #24254, #2851, .T. ) ;
#814 = CARTESIAN_POINT ( 'NONE',  ( -24.11099954625066744, -11.52470009423637620, 63.05244027053452527 ) ) ;
#815 = VECTOR ( 'NONE', #1897, 1000.000000000000000 ) ;
#816 = CIRCLE ( 'NONE', #45654, 5.249999999999998224 ) ;
#817 =( BOUNDED_CURVE ( )  B_SPLINE_CURVE ( 3, ( #15565, #572, #29890, #7247 ),
 .UNSPECIFIED., .F., .F. ) 
 B_SPLINE_CURVE_WITH_KNOTS ( ( 4, 4 ),
 ( 0.000000000000000000, 0.4074455897393677306 ),
 .UNSPECIFIED. ) 
 CURVE ( )  GEOMETRIC_REPRESENTATION_ITEM ( )  RATIONAL_B_SPLINE_CURVE ( ( 1.000000000000000000, 0.4567392136813272496, 0.3561768502900285460, 0.6983129098261039447 ) ) 
 REPRESENTATION_ITEM ( '' )  );
#818 = CARTESIAN_POINT ( 'NONE',  ( -14.52870633129714406, -21.67373273928137323, 58.32764366538068401 ) ) ;
#819 = DIRECTION ( 'NONE',  ( 1.000000000000000000, -4.164305804376849172E-17, 1.614929280266638808E-16 ) ) ;
#820 = CARTESIAN_POINT ( 'NONE',  ( -17.43659385759799108, -8.995762431863214559, 51.38120296130585274 ) ) ;
#821 = AXIS2_PLACEMENT_3D ( 'NONE', #16794, #39462, #35026 ) ;
#822 = DIRECTION ( 'NONE',  ( -3.071710424422018668E-17, 6.404604876783312462E-16, 1.000000000000000000 ) ) ;
#823 = DIRECTION ( 'NONE',  ( -0.000000000000000000, -1.000000000000000000, -0.000000000000000000 ) ) ;
#824 = EDGE_CURVE ( 'NONE', #29117, #42781, #29212, .T. ) ;
#825 = ADVANCED_FACE ( 'NONE', ( #25279 ), #2620, .T. ) ;
#826 = CYLINDRICAL_SURFACE ( 'NONE', #44109, 1.949999999999999734 ) ;
#827 = CARTESIAN_POINT ( 'NONE',  ( -19.43034385650552309, -9.794322478646142471, 51.19202720610083190 ) ) ;
#829 = EDGE_CURVE ( 'NONE', #42076, #28542, #17636, .T. ) ;
#828 = VERTEX_POINT ( 'NONE', #14155 ) ;
#830 = FACE_OUTER_BOUND ( 'NONE', #37021, .T. ) ;
#831 = DIRECTION ( 'NONE',  ( 4.924618305738831318E-06, 4.007739938527551184E-06, 0.9999999999798430128 ) ) ;
#832 = ORIENTED_EDGE ( 'NONE', *, *, #19343, .T. ) ;
#833 = DIRECTION ( 'NONE',  ( 2.846534188916127659E-06, 1.189262794724463340E-05, 0.9999999999252312533 ) ) ;
#834 = VECTOR ( 'NONE', #24049, 999.9999999999998863 ) ;
#835 = CARTESIAN_POINT ( 'NONE',  ( -21.51679988820674438, -20.55329806219026523, 72.40957539702174017 ) ) ;
#836 = ADVANCED_FACE ( 'NONE', ( #24317 ), #20622, .T. ) ;
#837 = CARTESIAN_POINT ( 'NONE',  ( -20.92409385541305511, -10.60920654474410618, 80.49999999999998579 ) ) ;
#838 = ORIENTED_EDGE ( 'NONE', *, *, #11852, .F. ) ;
#839 = CARTESIAN_POINT ( 'NONE',  ( -20.50876352152090121, -19.05741946913900620, 50.77966884056655772 ) ) ;
#840 =( BOUNDED_CURVE ( )  B_SPLINE_CURVE ( 3, ( #7888, #8613, #41856, #11814 ),
 .UNSPECIFIED., .F., .F. ) 
 B_SPLINE_CURVE_WITH_KNOTS ( ( 4, 4 ),
 ( 0.5000000000000000000, 0.9074455897393669535 ),
 .UNSPECIFIED. ) 
 CURVE ( )  GEOMETRIC_REPRESENTATION_ITEM ( )  RATIONAL_B_SPLINE_CURVE ( ( 1.000000000000006883, 0.4567392136813371306, 0.3561768502900272693, 0.6983129098260848489 ) ) 
 REPRESENTATION_ITEM ( '' )  );
#841 = CARTESIAN_POINT ( 'NONE',  ( -24.42310880397785411, -14.69177626764110300, 59.43403519634394172 ) ) ;
#842 = CARTESIAN_POINT ( 'NONE',  ( -17.97037870217379307, -19.46375863019785513, 49.52966884056656482 ) ) ;
#843 = ADVANCED_FACE ( 'NONE', ( #17390 ), #6566, .T. ) ;
#844 = ORIENTED_EDGE ( 'NONE', *, *, #40091, .F. ) ;
#845 = AXIS2_PLACEMENT_3D ( 'NONE', #36479, #32795, #13827 ) ;
#846 = FACE_OUTER_BOUND ( 'NONE', #41853, .T. ) ;
#847 = CARTESIAN_POINT ( 'NONE',  ( -24.20817551436923765, -11.73026151181330512, 59.73881638530829008 ) ) ;
#848 = CARTESIAN_POINT ( 'NONE',  ( -20.37299714182666222, -8.405577154986387356, 67.08104082189564110 ) ) ;
#849 = CARTESIAN_POINT ( 'NONE',  ( -16.87409385759798752, -6.859212275519751323, 50.50378509014259265 ) ) ;
#850 = CARTESIAN_POINT ( 'NONE',  ( -23.12753516214766591, -18.86773028979367695, 62.63941477998005780 ) ) ;
#851 = B_SPLINE_CURVE_WITH_KNOTS ( 'NONE', 1,
 ( #38087, #15187 ),
 .UNSPECIFIED., .F., .F.,
 ( 2, 2 ),
 ( 0.000000000000000000, 1.000000000000000000 ),
 .UNSPECIFIED. ) ;
#852 = ORIENTED_EDGE ( 'NONE', *, *, #26295, .F. ) ;
#853 = ORIENTED_EDGE ( 'NONE', *, *, #18315, .F. ) ;
#854 = CARTESIAN_POINT ( 'NONE',  ( -21.56784385541304516, -9.357632978295830739, 49.97845033065684106 ) ) ;
#855 = CARTESIAN_POINT ( 'NONE',  ( -19.13461862846645900, -7.969822530380906933, 63.43089260374607363 ) ) ;
#856 = CIRCLE ( 'NONE', #26795, 3.982850737850967437 ) ;
#857 = DIRECTION ( 'NONE',  ( -3.071710424422018668E-17, 6.404604876783312462E-16, 1.000000000000000000 ) ) ;
#858 = AXIS2_PLACEMENT_3D ( 'NONE', #11219, #22052, #3330 ) ;
#859 = PRODUCT ( 'Cylinder Spindle Drive Pinion', 'Cylinder Spindle Drive Pinion', '', ( #38787 ) ) ;
#860 = CARTESIAN_POINT ( 'NONE',  ( -17.93190708896392493, -21.84390349538901077, 58.29064763788917958 ) ) ;
#861 = CARTESIAN_POINT ( 'NONE',  ( -15.27269024242438533, -21.52607325516635939, 72.46064223565690554 ) ) ;
#862 = CARTESIAN_POINT ( 'NONE',  ( -10.37795889460693033, -14.56696403379599403, 68.14328054657653411 ) ) ;
#863 = AXIS2_PLACEMENT_3D ( 'NONE', #23090, #7832, #22851 ) ;
#864 = DIRECTION ( 'NONE',  ( -2.866981220435666553E-17, 1.000000000000000000, 1.190614954331866791E-16 ) ) ;
#865 = EDGE_CURVE ( 'NONE', #1563, #42690, #28247, .T. ) ;
#866 = ORIENTED_EDGE ( 'NONE', *, *, #5394, .T. ) ;
#867 = CARTESIAN_POINT ( 'NONE',  ( -21.52107272639815960, -9.068161724387254097, 66.54661176836198422 ) ) ;
#868 = CARTESIAN_POINT ( 'NONE',  ( -18.92057448382017526, -7.919863665830077615, 67.20071783788056052 ) ) ;
#869 = ORIENTED_EDGE ( 'NONE', *, *, #30060, .T. ) ;
#870 = PLANE ( 'NONE',  #23720 ) ;
#871 = DIRECTION ( 'NONE',  ( 0.6264825908887947659, -0.7794354131762691873, 3.858680029754496192E-08 ) ) ;
#872 = EDGE_LOOP ( 'NONE', ( #3030, #44945, #18541, #2230, #9303 ) ) ;
#873 = EDGE_CURVE ( 'NONE', #19668, #43006, #40632, .T. ) ;
#874 = CIRCLE ( 'NONE', #39392, 1.500000000000001332 ) ;
#875 = EDGE_LOOP ( 'NONE', ( #46633, #12055, #15072, #2979, #36505 ) ) ;
#876 = FACE_OUTER_BOUND ( 'NONE', #32788, .T. ) ;
#877 = B_SPLINE_CURVE_WITH_KNOTS ( 'NONE', 3,
 ( #3640, #3903, #18909, #33656, #30250, #45269, #11518, #7845, #22865, #4148 ),
 .UNSPECIFIED., .F., .F.,
 ( 4, 2, 2, 2, 4 ),
 ( 0.1272669073657703986, 0.2522669073462747713, 0.3772669073267791440, 0.5022669073072835166, 0.6272669072877878893 ),
 .UNSPECIFIED. ) ;
#878 = CARTESIAN_POINT ( 'NONE',  ( -21.67414471755420635, -8.689506427787394571, 70.24477150985708818 ) ) ;
#879 = CARTESIAN_POINT ( 'NONE',  ( -20.92525905000154296, -8.233149033200417577, 59.94151005296296120 ) ) ;
#880 = EDGE_LOOP ( 'NONE', ( #22050, #8932, #18939, #35498, #20588 ) ) ;
#881 = CARTESIAN_POINT ( 'NONE',  ( -10.32029913342570815, -17.05393162916765348, 57.78786302709333000 ) ) ;
#882 = CARTESIAN_POINT ( 'NONE',  ( -17.70776835051902864, -22.25388969026799657, 58.52057945155585372 ) ) ;
#883 = CARTESIAN_POINT ( 'NONE',  ( -23.84653597794508784, -18.58622903642730151, 72.87712840465626130 ) ) ;
#884 = CYLINDRICAL_SURFACE ( 'NONE', #28170, 7.000000000000000888 ) ;
#885 = CIRCLE ( 'NONE', #32357, 5.249999999999998224 ) ;
#886 = B_SPLINE_CURVE_WITH_KNOTS ( 'NONE', 3,
 ( #32581, #5996, #36496, #32358, #36018, #2778, #5527, #43684, #20547, #16819 ),
 .UNSPECIFIED., .F., .F.,
 ( 4, 2, 2, 2, 4 ),
 ( 0.000000000000000000, 0.2500000000000000000, 0.5000000000000000000, 0.7500000000000000000, 1.000000000000000000 ),
 .UNSPECIFIED. ) ;
#887 = CARTESIAN_POINT ( 'NONE',  ( -22.17083152876919527, -19.95395936491961209, 62.42542368773413131 ) ) ;
#888 = LINE ( 'NONE', #11475, #13733 ) ;
#889 = ADVANCED_FACE ( 'NONE', ( #13916 ), #6318, .T. ) ;
#890 = CARTESIAN_POINT ( 'NONE',  ( 18.51825960693462392, 3.131787348086252365, 50.70169625874538610 ) ) ;
#891 = VERTEX_POINT ( 'NONE', #28962 ) ;
#892 = CARTESIAN_POINT ( 'NONE',  ( -12.91576191806997365, -9.388722997169709927, 71.13453240065665284 ) ) ;
#893 = ADVANCED_FACE ( 'NONE', ( #21099 ), #39805, .T. ) ;
#894 = ORIENTED_EDGE ( 'NONE', *, *, #44461, .T. ) ;
#895 = DIRECTION ( 'NONE',  ( 0.7621627669932625748, -0.6473854467078884456, 3.680865982637999047E-08 ) ) ;
#896 = CARTESIAN_POINT ( 'NONE',  ( -24.72409385541305582, -14.80920654474425291, 71.08235294117645253 ) ) ;
#897 = VERTEX_POINT ( 'NONE', #43756 ) ;
#898 = CIRCLE ( 'NONE', #11896, 7.500000000000000888 ) ;
#899 = CARTESIAN_POINT ( 'NONE',  ( -10.99582121268164414, -11.91441617825094923, 74.70840195586961840 ) ) ;
#900 = CARTESIAN_POINT ( 'NONE',  ( -12.69123082366038702, -9.055659981287114135, 71.04199494340680587 ) ) ;
#901 = EDGE_LOOP ( 'NONE', ( #45786, #21346, #14320, #44685 ) ) ;
#902 = ORIENTED_EDGE ( 'NONE', *, *, #1866, .F. ) ;
#903 = ORIENTED_EDGE ( 'NONE', *, *, #44528, .F. ) ;
#904 = CARTESIAN_POINT ( 'NONE',  ( -10.39906353449755372, -15.43672942677450521, 61.45277822496478848 ) ) ;
#905 = VECTOR ( 'NONE', #30121, 1000.000000000000000 ) ;
#906 = CARTESIAN_POINT ( 'NONE',  ( -22.01784385541265365, -6.860780111193850672, 51.02154966934617164 ) ) ;
#908 = ADVANCED_FACE ( 'NONE', ( #25035 ), #21350, .T. ) ;
#907 = CARTESIAN_POINT ( 'NONE',  ( -16.59183161123116079, -7.337091670555837553, 53.76227901944321985 ) ) ;
#909 = CARTESIAN_POINT ( 'NONE',  ( -17.44602373156464026, -7.359070285474746065, 67.16006197583749326 ) ) ;
#910 = CARTESIAN_POINT ( 'NONE',  ( -10.27345486655506868, -12.71824029969684844, 64.45331411623358520 ) ) ;
#911 = CARTESIAN_POINT ( 'NONE',  ( -19.99284385541303166, -8.630756214087139000, 51.74842643355250971 ) ) ;
#912 = EDGE_LOOP ( 'NONE', ( #31979, #5220, #38589, #31849 ) ) ;
#913 = EDGE_LOOP ( 'NONE', ( #34629, #10370 ) ) ;
#914 = CARTESIAN_POINT ( 'NONE',  ( -21.88034385650551883, -6.424090610841176385, 49.80797279389977916 ) ) ;
#915 = CARTESIAN_POINT ( 'NONE',  ( -11.87343833590673192, -9.839839846620931141, 64.15197417175610894 ) ) ;
#916 = CARTESIAN_POINT ( 'NONE',  ( -21.02300714775091706, -21.33228198917356977, 62.21497154950080954 ) ) ;
#917 = FACE_OUTER_BOUND ( 'NONE', #9999, .T. ) ;
#918 = VERTEX_POINT ( 'NONE', #21585 ) ;
#919 = CARTESIAN_POINT ( 'NONE',  ( -15.49284385650551776, -7.406986770994973490, 48.81910596585309747 ) ) ;
#920 = ORIENTED_EDGE ( 'NONE', *, *, #12268, .T. ) ;
#921 = COLOUR_RGB ( '', 0.08235294, 0.09019608, 0.10196078) ;
#922 = CARTESIAN_POINT ( 'NONE',  ( -16.07504053214564976, -21.67928428602438018, 58.35755945890704766 ) ) ;
#923 = CARTESIAN_POINT ( 'NONE',  ( -19.08829560879351206, -7.958403603969639306, 63.73089209831277202 ) ) ;
#924 = AXIS2_PLACEMENT_3D ( 'NONE', #9917, #31839, #5505 ) ;
#925 = CARTESIAN_POINT ( 'NONE',  ( -24.64621740481133116, -16.83181165628401033, 54.27966884056654351 ) ) ;
#926 = ADVANCED_FACE ( 'NONE', ( #44984 ), #7796, .T. ) ;
#927 = ORIENTED_EDGE ( 'NONE', *, *, #45982, .T. ) ;
#928 = CARTESIAN_POINT ( 'NONE',  ( -14.36817892824948473, -8.455618309860652104, 67.54503025475186462 ) ) ;
#929 = CARTESIAN_POINT ( 'NONE',  ( -10.60176812795113932, -13.01736012961602817, 64.26835978638996494 ) ) ;
#930 = CARTESIAN_POINT ( 'NONE',  ( -24.17299910500858928, -11.65368927744445315, 59.64269123915968152 ) ) ;
#931 = ORIENTED_EDGE ( 'NONE', *, *, #15875, .F. ) ;
#932 = VECTOR ( 'NONE', #39496, 1000.000000000000114 ) ;
#933 = CARTESIAN_POINT ( 'NONE',  ( -13.16616306552584525, -16.76709000361798729, 52.02966884056656482 ) ) ;
#934 = CARTESIAN_POINT ( 'NONE',  ( -17.43166475307565122, -7.359124600834268115, 67.13544264266099049 ) ) ;
#935 = FACE_OUTER_BOUND ( 'NONE', #23114, .T. ) ;
#936 = VERTEX_POINT ( 'NONE', #44482 ) ;
#937 = CARTESIAN_POINT ( 'NONE',  ( -18.92057448382017526, -7.919863665830077615, 67.20071783788056052 ) ) ;
#938 = ORIENTED_EDGE ( 'NONE', *, *, #45364, .F. ) ;
#939 = CARTESIAN_POINT ( 'NONE',  ( -22.10931616815485512, -14.45671906187057765, 49.52966884056655772 ) ) ;
#940 = CARTESIAN_POINT ( 'NONE',  ( -13.08950423898529891, -12.99622877252704001, 49.52966884056655772 ) ) ;
#941 = ORIENTED_EDGE ( 'NONE', *, *, #5847, .F. ) ;
#942 = CARTESIAN_POINT ( 'NONE',  ( -16.29760782986628342, -22.17363506107604110, 61.87072849596245305 ) ) ;
#943 = CARTESIAN_POINT ( 'NONE',  ( -15.99215991861623110, -7.498114659224332179, 63.82011026836138967 ) ) ;
#944 = CARTESIAN_POINT ( 'NONE',  ( -14.21141923640507443, -8.087321911531361707, 67.42008472022612864 ) ) ;
#945 = ADVANCED_FACE ( 'NONE', ( #22813 ), #37804, .T. ) ;
#946 = VERTEX_POINT ( 'NONE', #25750 ) ;
#947 = CYLINDRICAL_SURFACE ( 'NONE', #43357, 2.000000000000001776 ) ;
#948 = ADVANCED_FACE ( 'NONE', ( #45222 ), #34106, .T. ) ;
#949 = LINE ( 'NONE', #16675, #21144 ) ;
#950 = CARTESIAN_POINT ( 'NONE',  ( -24.72409385541305582, -15.80920654474410725, 65.99999999999998579 ) ) ;
#951 = CARTESIAN_POINT ( 'NONE',  ( -17.42409385541299471, -14.80920654474435771, 49.52966884056655772 ) ) ;
#952 = ORIENTED_EDGE ( 'NONE', *, *, #23272, .T. ) ;
#953 = CARTESIAN_POINT ( 'NONE',  ( -17.42409385541299471, -14.80920654474435771, 49.52966884056655772 ) ) ;
#954 = EDGE_CURVE ( 'NONE', #6612, #48084, #29451, .T. ) ;
#955 = CARTESIAN_POINT ( 'NONE',  ( -11.39216336840796373, -18.45920852072106300, 61.29182966166492719 ) ) ;
#956 = VERTEX_POINT ( 'NONE', #29693 ) ;
#957 = ORIENTED_EDGE ( 'NONE', *, *, #17972, .F. ) ;
#958 = AXIS2_PLACEMENT_3D ( 'NONE', #45857, #23205, #45623 ) ;
#959 = FACE_BOUND ( 'NONE', #40484, .T. ) ;
#960 = LINE ( 'NONE', #19181, #25787 ) ;
#961 = EDGE_CURVE ( 'NONE', #37207, #21586, #14391, .T. ) ;
#962 = CARTESIAN_POINT ( 'NONE',  ( -12.99284385759798965, -8.630756214087126565, 51.74842643355248129 ) ) ;
#963 = CARTESIAN_POINT ( 'NONE',  ( -46.46711114793018282, -12.76354662275040219, 70.13000000000000966 ) ) ;
#964 =( BOUNDED_CURVE ( )  B_SPLINE_CURVE ( 3, ( #31982, #46997, #18156, #19569 ),
 .UNSPECIFIED., .F., .F. ) 
 B_SPLINE_CURVE_WITH_KNOTS ( ( 4, 4 ),
 ( 0.4074455897393637893, 0.5000000000000000000 ),
 .UNSPECIFIED. ) 
 CURVE ( )  GEOMETRIC_REPRESENTATION_ITEM ( )  RATIONAL_B_SPLINE_CURVE ( ( 0.6983129098261027234, 0.7760317562606876551, 0.8765941196519810852, 0.9999999999999698019 ) ) 
 REPRESENTATION_ITEM ( '' )  );
#965 = CARTESIAN_POINT ( 'NONE',  ( -12.16393509928502503, -9.533249887265045075, 57.25082014697580490 ) ) ;
#966 = CARTESIAN_POINT ( 'NONE',  ( -27.42409385541305511, -15.80920654474410725, 56.99999999999999289 ) ) ;
#967 = CARTESIAN_POINT ( 'NONE',  ( -11.39127492490111315, -11.16067319722467843, 60.69357916181100876 ) ) ;
#968 = ORIENTED_EDGE ( 'NONE', *, *, #7075, .F. ) ;
#969 = ORIENTED_EDGE ( 'NONE', *, *, #6552, .T. ) ;
#970 = DIRECTION ( 'NONE',  ( -2.866981220435666553E-17, 1.000000000000000000, 1.190614954331866791E-16 ) ) ;
#971 = CARTESIAN_POINT ( 'NONE',  ( -11.85857808612905195, -10.56289456917895642, 74.72268611605147726 ) ) ;
#972 = CARTESIAN_POINT ( 'NONE',  ( -17.22941483204795432, -7.758281381365547347, 74.05198360041919159 ) ) ;
#973 = CARTESIAN_POINT ( 'NONE',  ( -19.05639634586962572, -7.942579960324152921, 70.51501210008177623 ) ) ;
#974 = ADVANCED_FACE ( 'NONE', ( #10732 ), #37298, .T. ) ;
#975 =( BOUNDED_SURFACE ( )  B_SPLINE_SURFACE ( 3, 1, ( 
 ( #15684, #37861 ),
 ( #45763, #35130 ),
 ( #8324, #12015 ),
 ( #1395, #19394 ),
 ( #42293, #16414 ),
 ( #42050, #15927 ),
 ( #30498, #4874 ) ),
 .UNSPECIFIED., .T., .F., .F. ) 
 B_SPLINE_SURFACE_WITH_KNOTS ( ( 4, 3, 4 ),
 ( 2, 2 ),
 ( 0.000000000000000000, 0.5000000000000000000, 1.000000000000000000 ),
 ( 0.000000000000000000, 1.000000000000000000 ),
 .UNSPECIFIED. ) 
 GEOMETRIC_REPRESENTATION_ITEM ( )  RATIONAL_B_SPLINE_SURFACE ( (
 ( 1.000000000000000000, 1.000000000000000000),
 ( 0.3333333333333335369, 0.3333333333333330373),
 ( 0.3333333333333335369, 0.3333333333333330373),
 ( 1.000000000000000000, 1.000000000000000000),
 ( 0.3333333333333333703, 0.3333333333333333703),
 ( 0.3333333333333333703, 0.3333333333333333703),
 ( 1.000000000000000000, 1.000000000000000000) ) ) 
 REPRESENTATION_ITEM ( '' )  SURFACE ( )  );
#976 = ORIENTED_EDGE ( 'NONE', *, *, #26378, .F. ) ;
#977 = EDGE_CURVE ( 'NONE', #20038, #21955, #394, .T. ) ;
#978 = VERTEX_POINT ( 'NONE', #4100 ) ;
#979 = CARTESIAN_POINT ( 'NONE',  ( -22.10931616815485512, -14.45671906187057765, 49.52966884056655772 ) ) ;
#980 = FACE_OUTER_BOUND ( 'NONE', #44154, .T. ) ;
#981 = CYLINDRICAL_SURFACE ( 'NONE', #44959, 0.1499999999999991063 ) ;
#982 = DIRECTION ( 'NONE',  ( 0.000000000000000000, 0.000000000000000000, 1.000000000000000000 ) ) ;
#983 = B_SPLINE_CURVE_WITH_KNOTS ( 'NONE', 3,
 ( #47931, #10510, #28251, #25516, #40529, #21823, #43277, #9548, #5844, #20858 ),
 .UNSPECIFIED., .F., .F.,
 ( 4, 2, 2, 2, 4 ),
 ( 0.000000000000000000, 0.2500000000000000000, 0.5000000000000000000, 0.7500000000000000000, 1.000000000000000000 ),
 .UNSPECIFIED. ) ;
#984 = ADVANCED_FACE ( 'NONE', ( #19099 ), #165, .T. ) ;
#985 = ORIENTED_EDGE ( 'NONE', *, *, #33172, .T. ) ;
#986 = CARTESIAN_POINT ( 'NONE',  ( -13.11378338524245812, -9.291623327890567552, 71.03852466965894052 ) ) ;
#987 =( BOUNDED_CURVE ( )  B_SPLINE_CURVE ( 3, ( #24182, #17000, #25146, #42894 ),
 .UNSPECIFIED., .F., .F. ) 
 B_SPLINE_CURVE_WITH_KNOTS ( ( 4, 4 ),
 ( 0.5000000000000000000, 0.9074455897393701731 ),
 .UNSPECIFIED. ) 
 CURVE ( )  GEOMETRIC_REPRESENTATION_ITEM ( )  RATIONAL_B_SPLINE_CURVE ( ( 0.9999999999999765743, 0.4567392136813188119, 0.3561768502900417022, 0.6983129098261199319 ) ) 
 REPRESENTATION_ITEM ( '' )  );
#988 = CARTESIAN_POINT ( 'NONE',  ( -18.53667165497532920, -10.24437071140731170, 49.52966884056655772 ) ) ;
#989 = EDGE_LOOP ( 'NONE', ( #28713, #41829, #48612, #29103, #37851 ) ) ;
#990 = CARTESIAN_POINT ( 'NONE',  ( -14.01118748589247964, -10.49619482288619565, 54.07175714974879099 ) ) ;
#991 = CARTESIAN_POINT ( 'NONE',  ( -22.20320197231171733, -19.92390356480266433, 66.00421731406686376 ) ) ;
#992 = ORIENTED_EDGE ( 'NONE', *, *, #27097, .F. ) ;
#993 = LINE ( 'NONE', #12790, #23602 ) ;
#994 = ORIENTED_EDGE ( 'NONE', *, *, #18757, .T. ) ;
#995 = DIRECTION ( 'NONE',  ( 1.069446452691264255E-06, -1.103879811633194674E-06, 0.9999999999988189447 ) ) ;
#996 = CARTESIAN_POINT ( 'NONE',  ( -20.84119837601463487, -20.97572066283330727, 62.26471400470415318 ) ) ;
#997 = VERTEX_POINT ( 'NONE', #15378 ) ;
#998 = CARTESIAN_POINT ( 'NONE',  ( -24.85359104829803911, -14.25571788259268402, 69.76779960783916579 ) ) ;
#999 = DIRECTION ( 'NONE',  ( -1.011289380576387089E-05, 7.260693218591336108E-06, -0.9999999999225059888 ) ) ;
#1000 = CARTESIAN_POINT ( 'NONE',  ( -15.97409385650551705, -9.792211528768504536, 50.49490371617623197 ) ) ;
#1001 = CARTESIAN_POINT ( 'NONE',  ( -17.59048621110443023, -21.80850830133927687, 58.47723572191701891 ) ) ;
#1002 = CARTESIAN_POINT ( 'NONE',  ( -22.26145519751894852, -9.143288655575599222, 59.82196963377553089 ) ) ;
#1003 = CARTESIAN_POINT ( 'NONE',  ( -13.40837994833333546, -8.534074693662999422, 57.16306079917540472 ) ) ;
#1004 = ORIENTED_EDGE ( 'NONE', *, *, #35816, .F. ) ;
#1005 = CARTESIAN_POINT ( 'NONE',  ( -19.15013611399638904, -21.59351999776188080, 58.80890875055925449 ) ) ;
#1006 = CARTESIAN_POINT ( 'NONE',  ( -14.49326647312024896, -18.48150914673672673, 49.52966884056656482 ) ) ;
#1007 = CARTESIAN_POINT ( 'NONE',  ( -15.66159385541290838, -7.228003583437949686, 51.38655588712003208 ) ) ;
#1008 = EDGE_CURVE ( 'NONE', #1447, #6775, #44248, .T. ) ;
#1009 = CARTESIAN_POINT ( 'NONE',  ( -22.47245519635065492, -19.73066437834766873, 72.65872596779033188 ) ) ;
#1010 = CARTESIAN_POINT ( 'NONE',  ( -20.78261395438590853, -20.95102100293006941, 62.11471427793520661 ) ) ;
#1011 = ORIENTED_EDGE ( 'NONE', *, *, #31859, .F. ) ;
#1012 = VERTEX_POINT ( 'NONE', #18856 ) ;
#1013 = EDGE_CURVE ( 'NONE', #39358, #7816, #7643, .T. ) ;
#1014 = DIRECTION ( 'NONE',  ( 1.927470528863184130E-16, 1.434740771370715221E-29, -1.000000000000000000 ) ) ;
#1015 = FACE_OUTER_BOUND ( 'NONE', #21866, .T. ) ;
#1016 = EDGE_LOOP ( 'NONE', ( #44504, #29127 ) ) ;
#1017 = CARTESIAN_POINT ( 'NONE',  ( -10.38423141237398895, -15.23952324640539935, 57.98281521108167880 ) ) ;
#1018 = FACE_OUTER_BOUND ( 'NONE', #3445, .T. ) ;
#1019 = CARTESIAN_POINT ( 'NONE',  ( -22.27409385759798965, -6.859212275519751323, 50.50378509014259265 ) ) ;
#1020 = CARTESIAN_POINT ( 'NONE',  ( -24.73624204583532205, -16.23579025085892269, 62.69305037171274364 ) ) ;
#1021 = CARTESIAN_POINT ( 'NONE',  ( -23.08280660609100110, -10.60377317445056811, 59.61675562601556067 ) ) ;
#1022 = CARTESIAN_POINT ( 'NONE',  ( -12.22219652746809793, -10.12507141233243502, 60.78591508415431832 ) ) ;
#1023 = CARTESIAN_POINT ( 'NONE',  ( -14.09914604623946488, -8.649277798895779412, 74.19954655170327840 ) ) ;
#1024 = ORIENTED_EDGE ( 'NONE', *, *, #31564, .F. ) ;
#1025 = DIRECTION ( 'NONE',  ( -0.1240347345892086200, 1.145860353393066553E-16, -0.9922778767136676281 ) ) ;
#1026 = CARTESIAN_POINT ( 'NONE',  ( -50.42409385541304800, -27.10920654474410796, 79.99999999999998579 ) ) ;
#1027 = CARTESIAN_POINT ( 'NONE',  ( -23.05195072219661512, -10.55808160950470409, 63.48674805708738234 ) ) ;
#1028 = FACE_OUTER_BOUND ( 'NONE', #36065, .T. ) ;
#1029 = CARTESIAN_POINT ( 'NONE',  ( -12.83007325466668114, -20.09077588727113550, 72.10653676829758751 ) ) ;
#1030 = EDGE_CURVE ( 'NONE', #42456, #13644, #12331, .T. ) ;
#1032 = ORIENTED_EDGE ( 'NONE', *, *, #8638, .T. ) ;
#1031 = EDGE_CURVE ( 'NONE', #44193, #26463, #2448, .T. ) ;
#1033 = ORIENTED_EDGE ( 'NONE', *, *, #19899, .F. ) ;
#1034 = CARTESIAN_POINT ( 'NONE',  ( -20.04849592361258104, -21.35284569240296548, 72.69006679631316103 ) ) ;
#1035 = ORIENTED_EDGE ( 'NONE', *, *, #3687, .F. ) ;
#1036 = EDGE_CURVE ( 'NONE', #25854, #1499, #47567, .T. ) ;
#1037 = EDGE_CURVE ( 'NONE', #115, #47219, #27621, .T. ) ;
#1038 = EDGE_CURVE ( 'NONE', #14018, #36826, #27456, .T. ) ;
#1039 = CARTESIAN_POINT ( 'NONE',  ( -11.21695167451617792, -18.92928555840075688, 64.79061121450172323 ) ) ;
#1040 = CARTESIAN_POINT ( 'NONE',  ( -24.09512891293812586, -12.68832253202152671, 70.05777624906316703 ) ) ;
#1041 = ORIENTED_EDGE ( 'NONE', *, *, #14345, .F. ) ;
#1042 = DIRECTION ( 'NONE',  ( -5.731567514496413899E-31, -1.020425574103664789E-16, -1.000000000000000000 ) ) ;
#1043 = VECTOR ( 'NONE', #24003, 1000.000000000000000 ) ;
#1044 = EDGE_LOOP ( 'NONE', ( #8822, #28243, #26604, #26293, #18594 ) ) ;
#1045 = CARTESIAN_POINT ( 'NONE',  ( -17.77205755976807566, -21.85076284820492987, 58.69993615557697098 ) ) ;
#1046 = CARTESIAN_POINT ( 'NONE',  ( -19.17604249790256077, -21.63836284480991878, 58.53979515915469278 ) ) ;
#1047 = ORIENTED_EDGE ( 'NONE', *, *, #28049, .F. ) ;
#1048 = CARTESIAN_POINT ( 'NONE',  ( -20.11870507851999079, -21.33255209822014820, 69.09049654866474555 ) ) ;
#1049 = CARTESIAN_POINT ( 'NONE',  ( -13.38554957454228500, -8.548802447020154460, 57.11967752468037673 ) ) ;
#1050 = ORIENTED_EDGE ( 'NONE', *, *, #3461, .T. ) ;
#1051 = CARTESIAN_POINT ( 'NONE',  ( -11.89179040387956832, -10.43929601004734664, 70.96893105543333036 ) ) ;
#1052 = LINE ( 'NONE', #8439, #21248 ) ;
#1053 = CARTESIAN_POINT ( 'NONE',  ( -18.08034385541301603, -9.360768649639462424, 51.01397948905908919 ) ) ;
#1054 = ORIENTED_EDGE ( 'NONE', *, *, #36056, .T. ) ;
#1055 = CARTESIAN_POINT ( 'NONE',  ( -10.43949455435184603, -13.84896052950683476, 57.46297163929641982 ) ) ;
#1056 = ADVANCED_FACE ( 'NONE', ( #4331 ), #19586, .F. ) ;
#1057 = CARTESIAN_POINT ( 'NONE',  ( -17.76558202972499245, -21.80099470530900163, 58.40553380166819153 ) ) ;
#1058 = CARTESIAN_POINT ( 'NONE',  ( -11.54697730414119228, -10.23050705058286525, 71.10746578893807168 ) ) ;
#1059 = CARTESIAN_POINT ( 'NONE',  ( -21.35673258969865174, -10.96416394607318701, 54.07175714974879099 ) ) ;
#1060 = DIRECTION ( 'NONE',  ( -0.3478314405900308492, -0.9375570856950864451, 0.000000000000000000 ) ) ;
#1061 = CYLINDRICAL_SURFACE ( 'NONE', #12882, 0.1500000000000023259 ) ;
#1062 = DIRECTION ( 'NONE',  ( -3.071710424422018668E-17, 6.404604876783312462E-16, 1.000000000000000000 ) ) ;
#1063 = CARTESIAN_POINT ( 'NONE',  ( -24.31482341358216104, -13.31912415075585088, 59.51267924675325816 ) ) ;
#1064 = CARTESIAN_POINT ( 'NONE',  ( -22.14133254371160930, -20.05921860014851532, 69.31850691956374533 ) ) ;
#1065 = CARTESIAN_POINT ( 'NONE',  ( -14.64909385650551776, -8.104110260919579645, 48.81699501597546487 ) ) ;
#1066 = VERTEX_POINT ( 'NONE', #31148 ) ;
#1067 = EDGE_CURVE ( 'NONE', #31867, #31795, #5431, .T. ) ;
#1068 = CARTESIAN_POINT ( 'NONE',  ( -21.79028809537168243, -9.273590339475653366, 63.47681654923867711 ) ) ;
#1069 = CARTESIAN_POINT ( 'NONE',  ( -24.25171796977671335, -16.35308120058899206, 59.42332432118549690 ) ) ;
#1070 = ORIENTED_EDGE ( 'NONE', *, *, #26487, .T. ) ;
#1071 = CARTESIAN_POINT ( 'NONE',  ( -15.09544296547830022, -21.46351980780830715, 65.25596681500472585 ) ) ;
#1072 = FACE_OUTER_BOUND ( 'NONE', #12499, .T. ) ;
#1073 = CARTESIAN_POINT ( 'NONE',  ( -20.27839375093418184, -21.74978099588899028, 54.02222386812612598 ) ) ;
#1074 = ORIENTED_EDGE ( 'NONE', *, *, #35715, .T. ) ;
#1075 = CARTESIAN_POINT ( 'NONE',  ( -24.41055578522490066, -14.37307875356631648, 66.46827409029781109 ) ) ;
#1076 = CARTESIAN_POINT ( 'NONE',  ( -10.04844915070208344, -15.85969764522557668, 64.76417530519553623 ) ) ;
#1077 = DIRECTION ( 'NONE',  ( -5.731567514496413899E-31, -1.020425574103664789E-16, -1.000000000000000000 ) ) ;
#1078 = ORIENTED_EDGE ( 'NONE', *, *, #40792, .F. ) ;
#1079 = VECTOR ( 'NONE', #1783, 1000.000000000000000 ) ;
#1080 = CARTESIAN_POINT ( 'NONE',  ( -18.53556552080321751, -22.17591605216722428, 72.40015545304112266 ) ) ;
#1081 = CARTESIAN_POINT ( 'NONE',  ( -24.38910862430834570, -17.45374016378893955, 69.57486276871010489 ) ) ;
#1082 = CARTESIAN_POINT ( 'NONE',  ( -10.40245588357037043, -14.17414831712846990, 61.20349182037644198 ) ) ;
#1083 = CARTESIAN_POINT ( 'NONE',  ( -15.61945779041031201, -7.581001026129836617, 70.86635785818099009 ) ) ;
#1084 = B_SPLINE_CURVE_WITH_KNOTS ( 'NONE', 1,
 ( #15887, #15640 ),
 .UNSPECIFIED., .F., .F.,
 ( 2, 2 ),
 ( 0.000000000000000000, 1.000000000000000000 ),
 .UNSPECIFIED. ) ;
#1085 = CARTESIAN_POINT ( 'NONE',  ( -18.67409385759799179, -6.859212275519751323, 50.50378509014259265 ) ) ;
#1086 = VERTEX_POINT ( 'NONE', #42491 ) ;
#1087 = ORIENTED_EDGE ( 'NONE', *, *, #5470, .F. ) ;
#1088 = CARTESIAN_POINT ( 'NONE',  ( -20.94909385541304303, -8.112991634885936776, 51.74999426922421719 ) ) ;
#1089 = EDGE_CURVE ( 'NONE', #566, #12811, #46892, .T. ) ;
#1090 = EDGE_CURVE ( 'NONE', #31795, #26956, #3163, .T. ) ;
#1091 = CARTESIAN_POINT ( 'NONE',  ( -10.73979281777117301, -12.56761926564778875, 60.80413345197664654 ) ) ;
#1092 = CARTESIAN_POINT ( 'NONE',  ( -23.34884119489251475, -11.08117399487719545, 73.58866568711046341 ) ) ;
#1093 = EDGE_CURVE ( 'NONE', #8618, #44086, #38759, .T. ) ;
#1094 = EDGE_CURVE ( 'NONE', #2492, #18208, #561, .T. ) ;
#1095 = CARTESIAN_POINT ( 'NONE',  ( -23.14423626907140985, -18.93653154422199236, 58.88410448318015256 ) ) ;
#1096 = DIRECTION ( 'NONE',  ( 1.000000000000000000, 1.669677910507523057E-21, 6.493791346278465266E-22 ) ) ;
#1097 = DIRECTION ( 'NONE',  ( 1.000000000000000000, -1.224646799147353207E-16, 3.142942573426604379E-15 ) ) ;
#1098 = ORIENTED_EDGE ( 'NONE', *, *, #43731, .F. ) ;
#1099 =( BOUNDED_CURVE ( )  B_SPLINE_CURVE ( 3, ( #48352, #40977, #26204, #14838 ),
 .UNSPECIFIED., .F., .F. ) 
 B_SPLINE_CURVE_WITH_KNOTS ( ( 4, 4 ),
 ( 6.147240100463230661, 6.419130513895940915 ),
 .UNSPECIFIED. ) 
 CURVE ( )  GEOMETRIC_REPRESENTATION_ITEM ( )  RATIONAL_B_SPLINE_CURVE ( ( 1.000000000000000000, 0.9938491152761211866, 0.9938491152761211866, 1.000000000000000000 ) ) 
 REPRESENTATION_ITEM ( '' )  );
#1100 = FACE_OUTER_BOUND ( 'NONE', #23068, .T. ) ;
#1101 = AXIS2_PLACEMENT_3D ( 'NONE', #39404, #35686, #5686 ) ;
#1102 = ORIENTED_EDGE ( 'NONE', *, *, #46888, .F. ) ;
#1103 = CARTESIAN_POINT ( 'NONE',  ( -13.37018359880637064, -21.05987222909415735, 61.67679642377481741 ) ) ;
#1104 = CARTESIAN_POINT ( 'NONE',  ( -50.42609385541305755, -14.90920654474421170, 67.05882352941175384 ) ) ;
#1105 = VERTEX_POINT ( 'NONE', #16362 ) ;
#1106 = DIRECTION ( 'NONE',  ( 0.3124635249310678264, 0.8422251632096484641, -0.4393441931380601684 ) ) ;
#1107 = EDGE_CURVE ( 'NONE', #11974, #16121, #19840, .T. ) ;
#1108 = DIRECTION ( 'NONE',  ( -3.071710424422018668E-17, 6.404604876783312462E-16, 1.000000000000000000 ) ) ;
#1109 = CARTESIAN_POINT ( 'NONE',  ( -23.85820194903862657, -17.69173191509663567, 62.48833042115954584 ) ) ;
#1110 = ORIENTED_EDGE ( 'NONE', *, *, #21877, .F. ) ;
#1111 = CARTESIAN_POINT ( 'NONE',  ( -20.88948204121561503, -21.40431582783964970, 58.82192061885749013 ) ) ;
#1113 =( BOUNDED_CURVE ( )  B_SPLINE_CURVE ( 3, ( #40647, #6685, #32776, #6455 ),
 .UNSPECIFIED., .F., .F. ) 
 B_SPLINE_CURVE_WITH_KNOTS ( ( 4, 4 ),
 ( 0.000000000000000000, 0.4074455897393638448 ),
 .UNSPECIFIED. ) 
 CURVE ( )  GEOMETRIC_REPRESENTATION_ITEM ( )  RATIONAL_B_SPLINE_CURVE ( ( 1.000000000000000000, 0.4567392136813325787, 0.3561768502900305444, 0.6983129098260937306 ) ) 
 REPRESENTATION_ITEM ( '' )  );
#1112 = CARTESIAN_POINT ( 'NONE',  ( -10.88909980223564666, -11.23174460660519713, 64.32598909751834526 ) ) ;
#1114 = FACE_BOUND ( 'NONE', #9980, .T. ) ;
#1115 = APPLICATION_PROTOCOL_DEFINITION ( 'draft international standard', 'automotive_design', 1998, #3598 ) ;
#1116 = CARTESIAN_POINT ( 'NONE',  ( -22.05923734882601295, -20.05472318235705131, 62.53439162613685909 ) ) ;
#1117 = DIRECTION ( 'NONE',  ( -3.071710424422018668E-17, 6.404604876783312462E-16, 1.000000000000000000 ) ) ;
#1118 = LINE ( 'NONE', #16118, #43196 ) ;
#1119 = EDGE_LOOP ( 'NONE', ( #2792, #21677 ) ) ;
#1120 = CARTESIAN_POINT ( 'NONE',  ( -7.112004074929013875, -11.66554931205259749, 54.49999999999995026 ) ) ;
#1121 = EDGE_LOOP ( 'NONE', ( #5972, #21631, #1124, #13446 ) ) ;
#1122 = CARTESIAN_POINT ( 'NONE',  ( -20.08692735517319861, -21.76724714254084248, 72.54445348735094967 ) ) ;
#1123 = CARTESIAN_POINT ( 'NONE',  ( -16.79037046003568179, -22.23232723477725514, 68.81747882983158604 ) ) ;
#1124 = ORIENTED_EDGE ( 'NONE', *, *, #155, .F. ) ;
#1125 = LINE ( 'NONE', #31171, #38141 ) ;
#1126 = FACE_BOUND ( 'NONE', #38167, .T. ) ;
#1127 = ORIENTED_EDGE ( 'NONE', *, *, #22561, .T. ) ;
#1128 = EDGE_LOOP ( 'NONE', ( #17501, #1465, #32847, #25776, #7913, #11061 ) ) ;
#1129 = ORIENTED_EDGE ( 'NONE', *, *, #22650, .F. ) ;
#1130 = DIRECTION ( 'NONE',  ( -0.2189141945955536406, 0.9757441136919965397, 0.000000000000000000 ) ) ;
#1131 = FACE_OUTER_BOUND ( 'NONE', #31473, .T. ) ;
#1132 = CARTESIAN_POINT ( 'NONE',  ( -16.19909385759799036, -8.105421454601382081, 49.25000573077640098 ) ) ;
#1133 = CARTESIAN_POINT ( 'NONE',  ( -21.76676701690912807, -20.36762673175126181, 59.06443059911789106 ) ) ;
#1134 = CARTESIAN_POINT ( 'NONE',  ( -10.31379496977684340, -12.58270390103710668, 64.45491433821949556 ) ) ;
#1135 = CARTESIAN_POINT ( 'NONE',  ( -12.82148049030644366, -13.86501071932494789, 49.52966884056655772 ) ) ;
#1136 = VERTEX_POINT ( 'NONE', #42244 ) ;
#1137 = VERTEX_POINT ( 'NONE', #1109 ) ;
#1138 = AXIS2_PLACEMENT_3D ( 'NONE', #47596, #28869, #48300 ) ;
#1139 = B_SPLINE_CURVE_WITH_KNOTS ( 'NONE', 3,
 ( #28112, #43139, #5725, #9663, #31572, #46605, #12612, #20971, #42669, #35970 ),
 .UNSPECIFIED., .F., .F.,
 ( 4, 2, 2, 2, 4 ),
 ( 0.000000000000000000, 0.2500000000000000000, 0.5000000000000000000, 0.7500000000000000000, 1.000000000000000000 ),
 .UNSPECIFIED. ) ;
#1140 = EDGE_CURVE ( 'NONE', #18330, #38687, #43488, .T. ) ;
#1141 = DIRECTION ( 'NONE',  ( -0.09332174201254904433, -0.9956360040033421788, 0.000000000000000000 ) ) ;
#1142 = CARTESIAN_POINT ( 'NONE',  ( -10.51635438871963579, -15.94466521842666573, 68.26151329549378488 ) ) ;
#1143 = CARTESIAN_POINT ( 'NONE',  ( -19.60046948880987117, -21.46228020301366257, 65.76486213989072382 ) ) ;
#1144 = ORIENTED_EDGE ( 'NONE', *, *, #15305, .F. ) ;
#1145 = CARTESIAN_POINT ( 'NONE',  ( -13.80534385650551776, -8.801233750844183135, 48.81488406609782515 ) ) ;
#1146 = B_SPLINE_CURVE_WITH_KNOTS ( 'NONE', 3,
 ( #11930, #13594, #21257, #28153, #25427, #9697, #3003, #21500, #17541, #14065 ),
 .UNSPECIFIED., .F., .F.,
 ( 4, 2, 2, 2, 4 ),
 ( 0.1272669073658299899, 0.2522669073463197353, 0.3772669073268094531, 0.5022669073072967283, 0.6272669072877841145 ),
 .UNSPECIFIED. ) ;
#1148 = ORIENTED_EDGE ( 'NONE', *, *, #13070, .T. ) ;
#1147 = EDGE_CURVE ( 'NONE', #22754, #16663, #38134, .T. ) ;
#1149 = CARTESIAN_POINT ( 'NONE',  ( -13.27770768808251134, -9.107454094634597652, 63.90946529206384241 ) ) ;
#1150 = CARTESIAN_POINT ( 'NONE',  ( -12.60165769527841384, -19.96275654529059906, 61.55245915020547898 ) ) ;
#1151 = EDGE_CURVE ( 'NONE', #13240, #35848, #24263, .T. ) ;
#1152 = B_SPLINE_CURVE_WITH_KNOTS ( 'NONE', 3,
 ( #34203, #26107, #3694, #33459, #11566, #14993, #41123, #37398, #3946, #22408 ),
 .UNSPECIFIED., .F., .F.,
 ( 4, 2, 2, 2, 4 ),
 ( 0.000000000000000000, 0.2500000000000000000, 0.5000000000000000000, 0.7500000000000000000, 1.000000000000000000 ),
 .UNSPECIFIED. ) ;
#1153 = CARTESIAN_POINT ( 'NONE',  ( -18.53556552080321751, -22.17591605216722428, 72.40015545304112266 ) ) ;
#1154 = EDGE_CURVE ( 'NONE', #38392, #6133, #13214, .T. ) ;
#1155 = ORIENTED_EDGE ( 'NONE', *, *, #22793, .F. ) ;
#1156 = CARTESIAN_POINT ( 'NONE',  ( -21.06159385541298334, -7.228003583438046498, 51.38655588711993261 ) ) ;
#1157 = CARTESIAN_POINT ( 'NONE',  ( -50.42509385541305988, -6.359206544744109735, 51.54999999999998295 ) ) ;
#1158 = CARTESIAN_POINT ( 'NONE',  ( -18.15831417771707379, -22.22293841580443186, 65.49532158008852889 ) ) ;
#1159 = ORIENTED_EDGE ( 'NONE', *, *, #43377, .F. ) ;
#1160 = LINE ( 'NONE', #26797, #17877 ) ;
#1161 = CARTESIAN_POINT ( 'NONE',  ( -17.43006558257920346, -7.359130651351934560, 67.27685495689534889 ) ) ;
#1162 = CARTESIAN_POINT ( 'NONE',  ( -12.35277332135121675, -20.26681466537264242, 68.45162004874669037 ) ) ;
#1163 = ORIENTED_EDGE ( 'NONE', *, *, #43106, .T. ) ;
#1164 = CARTESIAN_POINT ( 'NONE',  ( -24.72409385541305582, -14.80920654474424225, 70.97647058823527288 ) ) ;
#1165 = VERTEX_POINT ( 'NONE', #31647 ) ;
#1166 = VECTOR ( 'NONE', #3129, 1000.000000000000114 ) ;
#1167 = CARTESIAN_POINT ( 'NONE',  ( -24.30164805153987473, -16.37256343635084477, 63.00817566860099106 ) ) ;
#1168 = VERTEX_POINT ( 'NONE', #5556 ) ;
#1169 = LINE ( 'NONE', #30984, #35251 ) ;
#1170 = DIRECTION ( 'NONE',  ( 5.539632631852608384E-05, 0.6451160323795128715, -0.7640846168443403696 ) ) ;
#1171 = AXIS2_PLACEMENT_3D ( 'NONE', #7204, #36702, #10640 ) ;
#1172 = DIRECTION ( 'NONE',  ( -0.8324837747691418155, -0.5540494244615011832, 1.585791776141941048E-16 ) ) ;
#1173 = DIRECTION ( 'NONE',  ( 0.7841839494287637935, -0.6205284308219133349, 1.653628654373097423E-16 ) ) ;
#1174 = VERTEX_POINT ( 'NONE', #40250 ) ;
#1175 = CARTESIAN_POINT ( 'NONE',  ( -9.992360566757833240, -14.28769768793135242, 64.58792641534920165 ) ) ;
#1176 = CARTESIAN_POINT ( 'NONE',  ( -20.56282556578965881, -8.552218022744439097, 63.61121530278081337 ) ) ;
#1177 = CARTESIAN_POINT ( 'NONE',  ( -20.91306683646873310, -8.226686726328479082, 59.99125248244220643 ) ) ;
#1178 = CARTESIAN_POINT ( 'NONE',  ( -23.46741973463711872, -19.16603908095663655, 62.53902270128352825 ) ) ;
#1179 = VERTEX_POINT ( 'NONE', #43465 ) ;
#1180 = CARTESIAN_POINT ( 'NONE',  ( -13.92409385541305511, -10.60920654474410618, 80.49999999999998579 ) ) ;
#1181 = DIRECTION ( 'NONE',  ( -1.000000000000000000, 0.000000000000000000, 0.000000000000000000 ) ) ;
#1182 = ORIENTED_EDGE ( 'NONE', *, *, #7623, .F. ) ;
#1183 = ORIENTED_EDGE ( 'NONE', *, *, #16284, .T. ) ;
#1184 = FACE_OUTER_BOUND ( 'NONE', #31912, .T. ) ;
#1185 = CARTESIAN_POINT ( 'NONE',  ( -10.69671328391030229, -11.60805651651419446, 71.24894240167931514 ) ) ;
#1186 = LINE ( 'NONE', #15957, #1307 ) ;
#1187 =( BOUNDED_CURVE ( )  B_SPLINE_CURVE ( 3, ( #39103, #5387, #31961, #47229 ),
 .UNSPECIFIED., .F., .F. ) 
 B_SPLINE_CURVE_WITH_KNOTS ( ( 4, 4 ),
 ( 0.000000000000000000, 0.4074455897393669535 ),
 .UNSPECIFIED. ) 
 CURVE ( )  GEOMETRIC_REPRESENTATION_ITEM ( )  RATIONAL_B_SPLINE_CURVE ( ( 1.000000000000000000, 0.4567392136813300807, 0.3561768502900296007, 0.6983129098260987266 ) ) 
 REPRESENTATION_ITEM ( '' )  );
#1188 = CARTESIAN_POINT ( 'NONE',  ( -20.27409385650551599, -9.792211528768504536, 50.49490371617623197 ) ) ;
#1189 = CARTESIAN_POINT ( 'NONE',  ( -14.27319436148695431, -8.558459998996717388, 71.02957628730779049 ) ) ;
#1190 = EDGE_CURVE ( 'NONE', #8240, #40764, #32130, .T. ) ;
#1191 = PLANE ( 'NONE',  #1559 ) ;
#1192 = CARTESIAN_POINT ( 'NONE',  ( -18.64436893707341980, -7.459652816704011258, 73.98031072975879852 ) ) ;
#1193 = CARTESIAN_POINT ( 'NONE',  ( -12.39637281836977145, -9.867031899960309715, 57.38935535270289279 ) ) ;
#1194 = EDGE_LOOP ( 'NONE', ( #42954, #43904 ) ) ;
#1195 = ORIENTED_EDGE ( 'NONE', *, *, #20298, .T. ) ;
#1196 = LINE ( 'NONE', #8854, #39902 ) ;
#1197 = CARTESIAN_POINT ( 'NONE',  ( 0.000000000000000000, 0.000000000000000000, 0.000000000000000000 ) ) ;
#1198 = CARTESIAN_POINT ( 'NONE',  ( -16.89979169948162863, -10.14008855580012636, 49.52966884056655772 ) ) ;
#1199 = CARTESIAN_POINT ( 'NONE',  ( -13.35550522631041837, -8.568183888810063209, 57.15463030501995689 ) ) ;
#1200 = CARTESIAN_POINT ( 'NONE',  ( -23.91010245674826251, -17.57297063409389537, 62.75888927877479517 ) ) ;
#1201 = AXIS2_PLACEMENT_3D ( 'NONE', #10044, #25064, #40081 ) ;
#1202 = ORIENTED_EDGE ( 'NONE', *, *, #29445, .F. ) ;
#1203 = FACE_OUTER_BOUND ( 'NONE', #17281, .T. ) ;
#1204 = AXIS2_PLACEMENT_3D ( 'NONE', #899, #11308, #33434 ) ;
#1205 = CARTESIAN_POINT ( 'NONE',  ( -23.49605051889219709, -11.22618518380361330, 73.37665428612797314 ) ) ;
#1206 = ADVANCED_FACE ( 'NONE', ( #27938 ), #17572, .T. ) ;
#1207 = CARTESIAN_POINT ( 'NONE',  ( -45.38107656289594161, -12.76354662275040219, 70.13000000000000966 ) ) ;
#1208 = CARTESIAN_POINT ( 'NONE',  ( -15.83660554694375477, -7.530134340792297820, 67.27973953361981785 ) ) ;
#1209 = EDGE_CURVE ( 'NONE', #24622, #36187, #40491, .T. ) ;
#1210 = ORIENTED_EDGE ( 'NONE', *, *, #10005, .F. ) ;
#1211 = CARTESIAN_POINT ( 'NONE',  ( -22.22370946352282672, -9.111183370010303761, 59.90666632495347699 ) ) ;
#1212 = EDGE_CURVE ( 'NONE', #47915, #46865, #47396, .T. ) ;
#1213 = CARTESIAN_POINT ( 'NONE',  ( -24.36028583763659583, -16.11466138999042030, 69.67740616536292464 ) ) ;
#1214 = VERTEX_POINT ( 'NONE', #43216 ) ;
#1215 = PLANE ( 'NONE',  #24172 ) ;
#1216 = EDGE_CURVE ( 'NONE', #24840, #28874, #3510, .T. ) ;
#1217 = CARTESIAN_POINT ( 'NONE',  ( -13.85393748347032528, -8.270264590973253505, 74.38449983516251507 ) ) ;
#1218 = EDGE_LOOP ( 'NONE', ( #25656, #20939 ) ) ;
#1219 = CARTESIAN_POINT ( 'NONE',  ( -23.68696726785515949, -18.84393668709636671, 69.49360751211669651 ) ) ;
#1220 = VERTEX_POINT ( 'NONE', #5793 ) ;
#1221 = CYLINDRICAL_SURFACE ( 'NONE', #33799, 0.1500000000000061007 ) ;
#1222 = CARTESIAN_POINT ( 'NONE',  ( -21.55884032038934350, -8.611816057827914150, 73.78624026056009200 ) ) ;
#1223 = VERTEX_POINT ( 'NONE', #13390 ) ;
#1224 = CARTESIAN_POINT ( 'NONE',  ( -24.26499744607890818, -17.75976858747020160, 62.65856309191605789 ) ) ;
#1225 = CARTESIAN_POINT ( 'NONE',  ( -10.29794926819780088, -12.63594297046838477, 64.40802751477502852 ) ) ;
#1226 = CARTESIAN_POINT ( 'NONE',  ( -18.28034385650551741, -6.424090610841176385, 49.80797279389978627 ) ) ;
#1227 = CARTESIAN_POINT ( 'NONE',  ( -11.95536787350534169, -10.43947220190359637, 70.96893134409420156 ) ) ;
#1228 =( BOUNDED_SURFACE ( )  B_SPLINE_SURFACE ( 3, 1, ( 
 ( #16012, #34743 ),
 ( #46073, #12578 ),
 ( #42386, #27354 ),
 ( #8656, #23682 ),
 ( #43101, #4964 ),
 ( #1977, #9632 ),
 ( #35692, #19973 ) ),
 .UNSPECIFIED., .T., .F., .F. ) 
 B_SPLINE_SURFACE_WITH_KNOTS ( ( 4, 3, 4 ),
 ( 2, 2 ),
 ( 0.000000000000000000, 0.5000000000000000000, 1.000000000000000000 ),
 ( 0.000000000000000000, 1.000000000000000000 ),
 .UNSPECIFIED. ) 
 GEOMETRIC_REPRESENTATION_ITEM ( )  RATIONAL_B_SPLINE_SURFACE ( (
 ( 1.000000000000000000, 1.000000000000000000),
 ( 0.3333333333333335369, 0.3333333333333330373),
 ( 0.3333333333333335369, 0.3333333333333330373),
 ( 1.000000000000000000, 1.000000000000000000),
 ( 0.3333333333333333703, 0.3333333333333333703),
 ( 0.3333333333333333703, 0.3333333333333333703),
 ( 1.000000000000000000, 1.000000000000000000) ) ) 
 REPRESENTATION_ITEM ( '' )  SURFACE ( )  );
#1229 = CARTESIAN_POINT ( 'NONE',  ( -23.85748962928175132, -11.92509172808648543, 59.49707787073156595 ) ) ;
#1230 = CARTESIAN_POINT ( 'NONE',  ( -35.42409385541304800, -8.109206544743658540, 50.50000000000030553 ) ) ;
#1231 = ORIENTED_EDGE ( 'NONE', *, *, #27331, .F. ) ;
#1232 = CARTESIAN_POINT ( 'NONE',  ( -23.89706228095030482, -17.47391663821368724, 62.66464254354016106 ) ) ;
#1233 = CARTESIAN_POINT ( 'NONE',  ( -17.13503149044196761, -7.764836982087094164, 70.77563787455143540 ) ) ;
#1234 = VECTOR ( 'NONE', #9390, 1000.000000000000114 ) ;
#1235 = DIRECTION ( 'NONE',  ( 2.842893050599252319E-07, -1.090087279701840163E-07, 0.9999999999999535927 ) ) ;
#1236 = LINE ( 'NONE', #31282, #23232 ) ;
#1237 = EDGE_LOOP ( 'NONE', ( #17891, #42021, #3568, #14310, #27860 ) ) ;
#1238 = ORIENTED_EDGE ( 'NONE', *, *, #42119, .T. ) ;
#1239 = DIRECTION ( 'NONE',  ( -0.9930145540378109148, 0.1179919296777755394, 4.526730167978063816E-08 ) ) ;
#1240 = CARTESIAN_POINT ( 'NONE',  ( -10.36108929241354382, -12.43876823780533947, 60.93820193749152025 ) ) ;
#1241 = ORIENTED_EDGE ( 'NONE', *, *, #1212, .T. ) ;
#1242 = CARTESIAN_POINT ( 'NONE',  ( -24.32752796592761158, -15.96791130369872391, 66.06324927019940674 ) ) ;
#1243 = CARTESIAN_POINT ( 'NONE',  ( -15.73882891167430564, -7.552148466825388873, 67.30040598401383534 ) ) ;
#1244 = CARTESIAN_POINT ( 'NONE',  ( -20.75918756122348441, -8.147305293919229641, 63.42626095967343502 ) ) ;
#1245 = CARTESIAN_POINT ( 'NONE',  ( -43.04835856129541583, -14.80920654474411613, 58.00588235294116402 ) ) ;
#1246 = EDGE_CURVE ( 'NONE', #12395, #24862, #28441, .T. ) ;
#1247 = CARTESIAN_POINT ( 'NONE',  ( -10.60635910294346651, -17.81289749453643978, 71.82364097624930821 ) ) ;
#1248 = DIRECTION ( 'NONE',  ( 1.000000000000000000, 0.000000000000000000, -3.652049423109068320E-16 ) ) ;
#1249 =( BOUNDED_CURVE ( )  B_SPLINE_CURVE ( 3, ( #38551, #45061, #26087, #37376 ),
 .UNSPECIFIED., .F., .F. ) 
 B_SPLINE_CURVE_WITH_KNOTS ( ( 4, 4 ),
 ( 0.000000000000000000, 0.4074455897393611248 ),
 .UNSPECIFIED. ) 
 CURVE ( )  GEOMETRIC_REPRESENTATION_ITEM ( )  RATIONAL_B_SPLINE_CURVE ( ( 1.000000000000000000, 0.4567392136813308023, 0.3561768502900298783, 0.6983129098260971723 ) ) 
 REPRESENTATION_ITEM ( '' )  );
#1250 = CARTESIAN_POINT ( 'NONE',  ( -19.41474593944376537, -21.52019035999878938, 61.99503644832097393 ) ) ;
#1251 = VERTEX_POINT ( 'NONE', #9961 ) ;
#1252 = LINE ( 'NONE', #16256, #44627 ) ;
#1253 = LINE ( 'NONE', #27121, #32144 ) ;
#1254 = CARTESIAN_POINT ( 'NONE',  ( -10.44916082259176093, -15.83527127794237543, 64.80771589743309846 ) ) ;
#1255 = CARTESIAN_POINT ( 'NONE',  ( -13.87409053989354923, -20.84236645762476314, 68.45625181054862196 ) ) ;
#1256 = CARTESIAN_POINT ( 'NONE',  ( -11.86732220369407997, -9.846751984446582284, 64.28560238571537866 ) ) ;
#1258 = ADVANCED_FACE ( 'NONE', ( #24981 ), #10468, .T. ) ;
#1257 = B_SPLINE_CURVE_WITH_KNOTS ( 'NONE', 1,
 ( #34397, #692 ),
 .UNSPECIFIED., .F., .F.,
 ( 2, 2 ),
 ( 0.000000000000000000, 1.000000000000000000 ),
 .UNSPECIFIED. ) ;
#1259 = ORIENTED_EDGE ( 'NONE', *, *, #41275, .F. ) ;
#1260 = VERTEX_POINT ( 'NONE', #26196 ) ;
#1261 = CARTESIAN_POINT ( 'NONE',  ( -21.51159385650551670, -6.922745924619793101, 51.69366785382590024 ) ) ;
#1262 = ORIENTED_EDGE ( 'NONE', *, *, #42956, .T. ) ;
#1263 = DIRECTION ( 'NONE',  ( 0.1675476790616363121, -0.9858639740050647582, 1.006000811662237932E-16 ) ) ;
#1264 = CARTESIAN_POINT ( 'NONE',  ( -10.99225178418778448, -18.56881356696312579, 57.91376274275113900 ) ) ;
#1265 = VERTEX_POINT ( 'NONE', #7739 ) ;
#1266 = DIRECTION ( 'NONE',  ( -3.071710424422018668E-17, 6.404604876783312462E-16, 1.000000000000000000 ) ) ;
#1267 = AXIS2_PLACEMENT_3D ( 'NONE', #12783, #38885, #1708 ) ;
#1268 = EDGE_CURVE ( 'NONE', #978, #24257, #7995, .T. ) ;
#1269 = DIRECTION ( 'NONE',  ( -2.866981220435666553E-17, 1.000000000000000000, 1.190614954331866791E-16 ) ) ;
#1270 = VERTEX_POINT ( 'NONE', #37243 ) ;
#1271 = EDGE_CURVE ( 'NONE', #45644, #6216, #9567, .T. ) ;
#1272 = CARTESIAN_POINT ( 'NONE',  ( -15.96549791049196543, -7.503336649694742455, 63.77672698436073517 ) ) ;
#1273 = EDGE_CURVE ( 'NONE', #48456, #39905, #41114, .T. ) ;
#1274 = CARTESIAN_POINT ( 'NONE',  ( -23.77826927976139970, -17.74977700416402726, 62.58433988291946548 ) ) ;
#1275 = ORIENTED_EDGE ( 'NONE', *, *, #35978, .T. ) ;
#1276 = CARTESIAN_POINT ( 'NONE',  ( -17.42409385541305511, -14.80920654474411080, 47.99999999999997868 ) ) ;
#1277 = CARTESIAN_POINT ( 'NONE',  ( -17.59331747086620368, -7.761237804118462869, 63.85057029381062677 ) ) ;
#1278 = ORIENTED_EDGE ( 'NONE', *, *, #12418, .F. ) ;
#1279 = CARTESIAN_POINT ( 'NONE',  ( -22.17130234749883044, -20.55096496926394778, 58.87947491310501391 ) ) ;
#1280 = CARTESIAN_POINT ( 'NONE',  ( -19.43748438392636402, -21.56872497219108098, 58.41018533341049590 ) ) ;
#1281 = ORIENTED_EDGE ( 'NONE', *, *, #13800, .T. ) ;
#1282 = CARTESIAN_POINT ( 'NONE',  ( -16.31151605585062825, -19.37404237808139484, 49.52966884056656482 ) ) ;
#1283 = CARTESIAN_POINT ( 'NONE',  ( -22.22619359738691003, -20.50513629785891823, 58.94938195453792673 ) ) ;
#1284 = EDGE_CURVE ( 'NONE', #37234, #30602, #37046, .T. ) ;
#1285 = LINE ( 'NONE', #6453, #24285 ) ;
#1286 = DIRECTION ( 'NONE',  ( 0.000000000000000000, -0.9999954153791273948, -0.003028072113819838245 ) ) ;
#1287 = DIRECTION ( 'NONE',  ( -0.000000000000000000, -1.000000000000000000, -0.000000000000000000 ) ) ;
#1288 = CARTESIAN_POINT ( 'NONE',  ( -20.50877865959810364, -8.469702366710405883, 63.60561728082600297 ) ) ;
#1289 = EDGE_CURVE ( 'NONE', #45322, #16774, #44431, .T. ) ;
#1290 = CARTESIAN_POINT ( 'NONE',  ( -14.42683419600289163, -8.428067575814653267, 67.55975083869262221 ) ) ;
#1291 = CARTESIAN_POINT ( 'NONE',  ( -13.15543723850287172, -20.91502918201612005, 58.19650074752242830 ) ) ;
#1292 = DIRECTION ( 'NONE',  ( 0.2573866790907599622, 0.9663084897829603559, 6.714855467380900338E-08 ) ) ;
#1293 = ADVANCED_FACE ( 'NONE', ( #3040 ), #14576, .T. ) ;
#1294 = EDGE_CURVE ( 'NONE', #9944, #13421, #17053, .T. ) ;
#1295 = CARTESIAN_POINT ( 'NONE',  ( -17.57409385650551314, -9.792211528768504536, 50.49490371617623197 ) ) ;
#1296 = EDGE_LOOP ( 'NONE', ( #29061, #23387 ) ) ;
#1297 = CARTESIAN_POINT ( 'NONE',  ( -15.70730708645226237, -24.91091750872855215, 53.49999999999995026 ) ) ;
#1298 = FACE_OUTER_BOUND ( 'NONE', #39040, .T. ) ;
#1299 = EDGE_LOOP ( 'NONE', ( #12670, #21956, #20899, #18516 ) ) ;
#1300 = CARTESIAN_POINT ( 'NONE',  ( -48.42409385541304800, -25.10920654474410441, 45.99999999999998579 ) ) ;
#1301 = CARTESIAN_POINT ( 'NONE',  ( -14.13242279744181573, -8.574497162196568212, 74.21426705364891063 ) ) ;
#1302 = CARTESIAN_POINT ( 'NONE',  ( -21.17484060445739757, -20.78220707328100403, 72.93935319279944451 ) ) ;
#1303 = CARTESIAN_POINT ( 'NONE',  ( -12.68381388925888587, -19.95990997655619381, 68.63657438305759229 ) ) ;
#1304 = LINE ( 'NONE', #23249, #38376 ) ;
#1305 = ORIENTED_EDGE ( 'NONE', *, *, #4285, .F. ) ;
#1306 = CARTESIAN_POINT ( 'NONE',  ( -45.92409385541306222, -14.20920654474410760, 70.50000000000000000 ) ) ;
#1307 = VECTOR ( 'NONE', #19676, 1000.000000000000000 ) ;
#1308 = CARTESIAN_POINT ( 'NONE',  ( -20.66848101912799862, -8.549761622307149977, 60.12653141481577990 ) ) ;
#1309 = CARTESIAN_POINT ( 'NONE',  ( -14.54176566789882585, -21.67913831930545854, 58.28122448549703449 ) ) ;
#1310 = ORIENTED_EDGE ( 'NONE', *, *, #609, .T. ) ;
#1311 = CARTESIAN_POINT ( 'NONE',  ( -18.56068362409587280, -22.17200289566820715, 72.48522146388405929 ) ) ;
#1312 = CARTESIAN_POINT ( 'NONE',  ( -24.56076101444288184, -12.67091080028054684, 69.95055769627768427 ) ) ;
#1313 = CARTESIAN_POINT ( 'NONE',  ( -21.71949691563504459, -8.721965781586035860, 70.26985989995344539 ) ) ;
#1314 = B_SPLINE_CURVE_WITH_KNOTS ( 'NONE', 3,
 ( #34476, #30573, #38411, #45109, #4700, #8645, #15024, #1005, #34732, #4450 ),
 .UNSPECIFIED., .F., .F.,
 ( 4, 2, 2, 2, 4 ),
 ( 0.000000000000000000, 0.2500000000000000000, 0.5000000000000000000, 0.7500000000000000000, 1.000000000000000000 ),
 .UNSPECIFIED. ) ;
#1315 = CARTESIAN_POINT ( 'NONE',  ( -46.29409385541305255, -14.20920654474410760, 70.08498674719956512 ) ) ;
#1316 = ORIENTED_EDGE ( 'NONE', *, *, #11587, .F. ) ;
#1317 = VERTEX_POINT ( 'NONE', #18540 ) ;
#1318 = CARTESIAN_POINT ( 'NONE',  ( -23.42409385541304090, -9.359200813967568422, 50.49621490985803263 ) ) ;
#1319 = EDGE_CURVE ( 'NONE', #38388, #48213, #47870, .T. ) ;
#1320 = LINE ( 'NONE', #16332, #34267 ) ;
#1321 = CARTESIAN_POINT ( 'NONE',  ( -19.02055866782680482, -21.67977764378408878, 58.61687627430667646 ) ) ;
#1322 = ADVANCED_FACE ( 'NONE', ( #14104 ), #48109, .T. ) ;
#1323 = DIRECTION ( 'NONE',  ( 0.6607190350373968180, 0.7506333037770515082, 0.000000000000000000 ) ) ;
#1324 = CARTESIAN_POINT ( 'NONE',  ( -10.21764062494887781, -12.91954801228597915, 67.92327636273336111 ) ) ;
#1325 = CARTESIAN_POINT ( 'NONE',  ( -9.985760891864103428, -14.37924521898145258, 68.04455407903930109 ) ) ;
#1326 = CARTESIAN_POINT ( 'NONE',  ( -24.23356459391621343, -17.83169477672529624, 62.65173719855710033 ) ) ;
#1327 = ORIENTED_EDGE ( 'NONE', *, *, #34215, .T. ) ;
#1328 = CARTESIAN_POINT ( 'NONE',  ( -21.95217610637629946, -9.395202297576263462, 66.80583047767832738 ) ) ;
#1329 = DIRECTION ( 'NONE',  ( -2.866981220435666553E-17, 1.000000000000000000, 1.190614954331866791E-16 ) ) ;
#1330 = CIRCLE ( 'NONE', #8449, 5.000000000000000000 ) ;
#1331 = CIRCLE ( 'NONE', #45403, 1.250000000000001110 ) ;
#1332 = ORIENTED_EDGE ( 'NONE', *, *, #40037, .F. ) ;
#1333 = CARTESIAN_POINT ( 'NONE',  ( -50.42409385541304800, -25.10920654474410441, 79.99999999999998579 ) ) ;
#1334 = DIRECTION ( 'NONE',  ( -0.2479245821708770392, -0.9687793358424796608, -2.626836608334273943E-18 ) ) ;
#1335 = ORIENTED_EDGE ( 'NONE', *, *, #12126, .T. ) ;
#1336 = CARTESIAN_POINT ( 'NONE',  ( -10.90759852523040330, -17.49952041063523467, 68.09721944423131390 ) ) ;
#1337 = DIRECTION ( 'NONE',  ( -0.9687793358424822143, 0.2479245821708672415, 0.000000000000000000 ) ) ;
#1338 = VECTOR ( 'NONE', #13076, 1000.000000000000000 ) ;
#1339 = DIRECTION ( 'NONE',  ( -0.04108628546905146450, -0.9991556020692451412, 1.019563928860402566E-16 ) ) ;
#1340 = CARTESIAN_POINT ( 'NONE',  ( -24.46752114747617313, -17.23684389422572849, 72.99061869212614795 ) ) ;
#1341 = ORIENTED_EDGE ( 'NONE', *, *, #15090, .T. ) ;
#1342 = FACE_OUTER_BOUND ( 'NONE', #17900, .T. ) ;
#1343 = CARTESIAN_POINT ( 'NONE',  ( -20.54031095723443556, -8.042250736733803862, 66.93104081865082833 ) ) ;
#1344 = CARTESIAN_POINT ( 'NONE',  ( -10.92380316157302467, -11.16921865325121388, 64.25607897268513113 ) ) ;
#1345 = ADVANCED_FACE ( 'NONE', ( #6990 ), #22113, .T. ) ;
#1346 = DIRECTION ( 'NONE',  ( 0.9294853595766541243, 0.3688590060343629462, 0.000000000000000000 ) ) ;
#1347 = APPLICATION_PROTOCOL_DEFINITION ( 'draft international standard', 'automotive_design', 1998, #46687 ) ;
#1348 = B_SPLINE_CURVE_WITH_KNOTS ( 'NONE', 3,
 ( #18275, #25673, #13843, #13610, #33280, #2554, #47612, #7228, #6726, #32583 ),
 .UNSPECIFIED., .F., .F.,
 ( 4, 2, 2, 2, 4 ),
 ( 0.000000000000000000, 0.2500000000000000000, 0.5000000000000000000, 0.7500000000000000000, 1.000000000000000000 ),
 .UNSPECIFIED. ) ;
#1349 = EDGE_CURVE ( 'NONE', #33983, #40074, #17412, .T. ) ;
#1350 = ADVANCED_FACE ( 'NONE', ( #23234 ), #45656, .F. ) ;
#1351 = CARTESIAN_POINT ( 'NONE',  ( -12.91230480768039790, -16.07689808402359688, 49.52966884056655772 ) ) ;
#1352 = CARTESIAN_POINT ( 'NONE',  ( -14.21975182572090901, -8.525335417369671376, 67.25975088330713447 ) ) ;
#1353 = LINE ( 'NONE', #27468, #17228 ) ;
#1354 = ORIENTED_EDGE ( 'NONE', *, *, #2508, .T. ) ;
#1355 = DIRECTION ( 'NONE',  ( 0.8788484374452886216, -0.3260506722428096471, 0.3483050145059451985 ) ) ;
#1356 = VERTEX_POINT ( 'NONE', #45397 ) ;
#1357 = CARTESIAN_POINT ( 'NONE',  ( -11.21157628577468657, -11.58358644131346082, 67.61864608155907774 ) ) ;
#1358 = CARTESIAN_POINT ( 'NONE',  ( -14.80624607021532135, -8.317144234858641738, 60.31996281969095719 ) ) ;
#1359 = ORIENTED_EDGE ( 'NONE', *, *, #45101, .T. ) ;
#1360 = CARTESIAN_POINT ( 'NONE',  ( -23.89200480383413350, -11.11192299349349533, 70.07706151945906470 ) ) ;
#1361 = EDGE_CURVE ( 'NONE', #18903, #14963, #11138, .T. ) ;
#1362 = FACE_BOUND ( 'NONE', #14356, .T. ) ;
#1363 = EDGE_LOOP ( 'NONE', ( #16129, #27063 ) ) ;
#1364 = ORIENTED_EDGE ( 'NONE', *, *, #30212, .F. ) ;
#1365 = VERTEX_POINT ( 'NONE', #1059 ) ;
#1366 = CARTESIAN_POINT ( 'NONE',  ( -10.02210521578421520, -15.65432817399831045, 61.29434977362033976 ) ) ;
#1367 = FACE_OUTER_BOUND ( 'NONE', #6278, .T. ) ;
#1368 =( BOUNDED_SURFACE ( )  B_SPLINE_SURFACE ( 3, 1, ( 
 ( #11356, #10627 ),
 ( #29339, #10866 ),
 ( #41388, #7191 ),
 ( #6689, #36689 ),
 ( #22198, #7680 ),
 ( #15025, #14045 ),
 ( #37185, #18481 ) ),
 .UNSPECIFIED., .T., .F., .F. ) 
 B_SPLINE_SURFACE_WITH_KNOTS ( ( 4, 3, 4 ),
 ( 2, 2 ),
 ( 0.000000000000000000, 0.5000000000000000000, 1.000000000000000000 ),
 ( 0.000000000000000000, 1.000000000000000000 ),
 .UNSPECIFIED. ) 
 GEOMETRIC_REPRESENTATION_ITEM ( )  RATIONAL_B_SPLINE_SURFACE ( (
 ( 1.000000000000000000, 1.000000000000000000),
 ( 0.3333333333333335369, 0.3333333333333330373),
 ( 0.3333333333333335369, 0.3333333333333330373),
 ( 1.000000000000000000, 1.000000000000000000),
 ( 0.3333333333333333703, 0.3333333333333333703),
 ( 0.3333333333333333703, 0.3333333333333333703),
 ( 1.000000000000000000, 1.000000000000000000) ) ) 
 REPRESENTATION_ITEM ( '' )  SURFACE ( )  );
#1369 = CARTESIAN_POINT ( 'NONE',  ( -21.30260081908322078, -8.981780046862946065, 73.60128699524366880 ) ) ;
#1370 = CARTESIAN_POINT ( 'NONE',  ( -10.29339667142563819, -12.65123896477911103, 64.52482037846105811 ) ) ;
#1371 = CARTESIAN_POINT ( 'NONE',  ( -29.92409385541305156, -6.859206544744110623, 52.99999999999997158 ) ) ;
#1372 = VECTOR ( 'NONE', #42277, 1000.000000000000000 ) ;
#1373 = VECTOR ( 'NONE', #12491, 1000.000000000000000 ) ;
#1374 = VERTEX_POINT ( 'NONE', #19527 ) ;
#1375 = ORIENTED_EDGE ( 'NONE', *, *, #8206, .T. ) ;
#1376 = CARTESIAN_POINT ( 'NONE',  ( -21.03659385650551528, -6.915538690918074494, 49.31353937987644542 ) ) ;
#1377 = ADVANCED_FACE ( 'NONE', ( #37744 ), #4039, .F. ) ;
#1378 = CARTESIAN_POINT ( 'NONE',  ( -22.73618463404748624, -20.03370227938794912, 69.28762739622011679 ) ) ;
#1379 = CARTESIAN_POINT ( 'NONE',  ( -21.13453391143521287, -20.81317186429504673, 62.27038425631170782 ) ) ;
#1380 = AXIS2_PLACEMENT_3D ( 'NONE', #46005, #19661, #23351 ) ;
#1381 = DIRECTION ( 'NONE',  ( -3.413470714839332458E-33, 1.190614954331866791E-16, -1.000000000000000000 ) ) ;
#1382 =( BOUNDED_CURVE ( )  B_SPLINE_CURVE ( 3, ( #26147, #36954, #36698, #41158 ),
 .UNSPECIFIED., .F., .F. ) 
 B_SPLINE_CURVE_WITH_KNOTS ( ( 4, 4 ),
 ( 1.570796326794896780, 1.780235837034217283 ),
 .UNSPECIFIED. ) 
 CURVE ( )  GEOMETRIC_REPRESENTATION_ITEM ( )  RATIONAL_B_SPLINE_CURVE ( ( 1.000000000000000000, 0.9963479302455154896, 0.9963479302455154896, 1.000000000000000000 ) ) 
 REPRESENTATION_ITEM ( '' )  );
#1383 = CARTESIAN_POINT ( 'NONE',  ( -20.86784385650551954, -6.428312510596451368, 51.20221977374900035 ) ) ;
#1384 =( BOUNDED_CURVE ( )  B_SPLINE_CURVE ( 3, ( #40696, #6976, #39986, #29140 ),
 .UNSPECIFIED., .F., .F. ) 
 B_SPLINE_CURVE_WITH_KNOTS ( ( 4, 4 ),
 ( 0.4074455897393629566, 0.5000000000000000000 ),
 .UNSPECIFIED. ) 
 CURVE ( )  GEOMETRIC_REPRESENTATION_ITEM ( )  RATIONAL_B_SPLINE_CURVE ( ( 0.6983129098260889567, 0.7760317562606786623, 0.8765941196519776435, 0.9999999999999744649 ) ) 
 REPRESENTATION_ITEM ( '' )  );
#1385 = VECTOR ( 'NONE', #24930, 1000.000000000000227 ) ;
#1386 = ORIENTED_EDGE ( 'NONE', *, *, #25635, .F. ) ;
#1387 = CARTESIAN_POINT ( 'NONE',  ( -14.72722737765066725, -21.75407789377580059, 61.81413171700139486 ) ) ;
#1388 = CARTESIAN_POINT ( 'NONE',  ( -12.00744322407076226, -19.92521668911118482, 61.58333889064303435 ) ) ;
#1389 = DIRECTION ( 'NONE',  ( -1.198821490631147214E-05, 1.588017923320057101E-05, -0.9999999998020512315 ) ) ;
#1390 = ORIENTED_EDGE ( 'NONE', *, *, #13785, .F. ) ;
#1391 = CARTESIAN_POINT ( 'NONE',  ( -20.83659385541298548, -8.995762431863285613, 51.38120296130592379 ) ) ;
#1392 =( BOUNDED_CURVE ( )  B_SPLINE_CURVE ( 3, ( #29079, #29560, #17975, #40635 ),
 .UNSPECIFIED., .F., .F. ) 
 B_SPLINE_CURVE_WITH_KNOTS ( ( 4, 4 ),
 ( 0.000000000000000000, 0.4074455897393638448 ),
 .UNSPECIFIED. ) 
 CURVE ( )  GEOMETRIC_REPRESENTATION_ITEM ( )  RATIONAL_B_SPLINE_CURVE ( ( 1.000000000000000000, 0.4567392136813337444, 0.3561768502900309330, 0.6983129098260915102 ) ) 
 REPRESENTATION_ITEM ( '' )  );
#1393 = CARTESIAN_POINT ( 'NONE',  ( -22.75144419618436586, -9.600271701911582412, 73.59505825258622735 ) ) ;
#1394 = CARTESIAN_POINT ( 'NONE',  ( -16.36862302632751209, -10.24310716135927812, 49.52966884056655772 ) ) ;
#1395 = CARTESIAN_POINT ( 'NONE',  ( -12.45873566688478107, -9.804017486950373339, 57.10407583662104258 ) ) ;
#1396 = ORIENTED_EDGE ( 'NONE', *, *, #19094, .T. ) ;
#1397 = VECTOR ( 'NONE', #15816, 1000.000000000000114 ) ;
#1398 = CARTESIAN_POINT ( 'NONE',  ( -10.43905172760979028, -15.29054532034250968, 57.67865882576857928 ) ) ;
#1399 = B_SPLINE_CURVE_WITH_KNOTS ( 'NONE', 1,
 ( #10508, #44486 ),
 .UNSPECIFIED., .F., .F.,
 ( 2, 2 ),
 ( 0.000000000000000000, 1.000000000000000000 ),
 .UNSPECIFIED. ) ;
#1400 = CARTESIAN_POINT ( 'NONE',  ( -17.42409385541299471, -14.80920654474435771, 49.52966884056655772 ) ) ;
#1401 = FACE_OUTER_BOUND ( 'NONE', #33780, .T. ) ;
#1402 = ORIENTED_EDGE ( 'NONE', *, *, #48076, .F. ) ;
#1403 = CARTESIAN_POINT ( 'NONE',  ( -10.40245588357037043, -14.17414831712846990, 61.20349182037644198 ) ) ;
#1404 = VECTOR ( 'NONE', #1062, 1000.000000000000000 ) ;
#1405 = VECTOR ( 'NONE', #20685, 1000.000000000000114 ) ;
#1406 = VERTEX_POINT ( 'NONE', #42678 ) ;
#1407 = CARTESIAN_POINT ( 'NONE',  ( -19.15875595501757545, -7.563798684503558967, 63.56942691188406513 ) ) ;
#1408 = CARTESIAN_POINT ( 'NONE',  ( -16.36003348549149550, -21.72797215718117414, 61.75568179790091961 ) ) ;
#1409 = B_SPLINE_CURVE_WITH_KNOTS ( 'NONE', 3,
 ( #19579, #27449, #16355, #8039, #38033, #31387, #42236, #8264, #34336, #624 ),
 .UNSPECIFIED., .F., .F.,
 ( 4, 2, 2, 2, 4 ),
 ( 0.1272669073658067862, 0.2522669073462858735, 0.3772669073267650441, 0.5022669073072441037, 0.6272669072877232743 ),
 .UNSPECIFIED. ) ;
#1410 = VERTEX_POINT ( 'NONE', #34789 ) ;
#1411 = ADVANCED_FACE ( 'NONE', ( #41942 ), #27138, .T. ) ;
#1412 = CARTESIAN_POINT ( 'NONE',  ( -16.43749525924751964, -22.19434601430465293, 61.86912739712975906 ) ) ;
#1413 = CARTESIAN_POINT ( 'NONE',  ( -24.25757938109993717, -13.28409109838451663, 62.94337370252653585 ) ) ;
#1414 = DIRECTION ( 'NONE',  ( -3.071710424422018668E-17, 6.404604876783312462E-16, 1.000000000000000000 ) ) ;
#1415 = ORIENTED_EDGE ( 'NONE', *, *, #28603, .T. ) ;
#1416 = CARTESIAN_POINT ( 'NONE',  ( -11.06939607882469190, -17.86905163984256006, 71.45229597776977926 ) ) ;
#1417 = AXIS2_PLACEMENT_3D ( 'NONE', #25171, #21234, #33249 ) ;
#1418 = CARTESIAN_POINT ( 'NONE',  ( -4.924093855413050669, -6.859206544744110623, 47.99999999999998579 ) ) ;
#1419 = CARTESIAN_POINT ( 'NONE',  ( -10.46944733747312917, -15.96661384539355133, 67.99239968927004441 ) ) ;
#1420 = VERTEX_POINT ( 'NONE', #4273 ) ;
#1421 = CARTESIAN_POINT ( 'NONE',  ( -23.38410589725464916, -10.33907962427212190, 59.71708035543083071 ) ) ;
#1422 = ADVANCED_FACE ( 'NONE', ( #42435 ), #30630, .T. ) ;
#1423 = EDGE_CURVE ( 'NONE', #36239, #45570, #4083, .T. ) ;
#1424 = CYLINDRICAL_SURFACE ( 'NONE', #27500, 0.5000000000000004441 ) ;
#1425 = ORIENTED_EDGE ( 'NONE', *, *, #13096, .T. ) ;
#1426 = ORIENTED_EDGE ( 'NONE', *, *, #7501, .T. ) ;
#1427 = ADVANCED_FACE ( 'NONE', ( #30872 ), #32174, .T. ) ;
#1428 = CARTESIAN_POINT ( 'NONE',  ( -27.42409385541305511, -25.10920654474410441, 63.99999999999998579 ) ) ;
#1429 = CARTESIAN_POINT ( 'NONE',  ( -19.85889901765038346, -21.37233916515964438, 69.21353063550283480 ) ) ;
#1430 = PLANE ( 'NONE',  #34332 ) ;
#1431 = CARTESIAN_POINT ( 'NONE',  ( -18.24909385650551741, -8.104110260919579645, 48.81699501597546487 ) ) ;
#1432 = EDGE_CURVE ( 'NONE', #39290, #30479, #14258, .T. ) ;
#1433 = CARTESIAN_POINT ( 'NONE',  ( -18.75025350711597483, -7.885019284943789231, 70.37068061249377138 ) ) ;
#1434 = CARTESIAN_POINT ( 'NONE',  ( -23.55661029900229053, -18.29303667177271464, 72.64879359478229048 ) ) ;
#1435 = LINE ( 'NONE', #31729, #4314 ) ;
#1436 = CARTESIAN_POINT ( 'NONE',  ( -11.19706266256277694, -11.50303319689152914, 67.63336710488009373 ) ) ;
#1437 = VERTEX_POINT ( 'NONE', #28614 ) ;
#1438 = ORIENTED_EDGE ( 'NONE', *, *, #37978, .T. ) ;
#1439 = DIRECTION ( 'NONE',  ( -0.9959323210854038599, 0.09010444948746665350, 2.601165157765156148E-08 ) ) ;
#1440 = ADVANCED_FACE ( 'NONE', ( #20254 ), #9182, .T. ) ;
#1441 = DIRECTION ( 'NONE',  ( 0.000000000000000000, 0.000000000000000000, 1.000000000000000000 ) ) ;
#1442 = CARTESIAN_POINT ( 'NONE',  ( -22.02472224376031562, -20.08502103662938865, 58.95546057814475205 ) ) ;
#1443 = CARTESIAN_POINT ( 'NONE',  ( -6.424093855413058662, -6.859206544744110623, 52.99999999999998579 ) ) ;
#1444 = CARTESIAN_POINT ( 'NONE',  ( -18.69688219364054049, -7.467975623574482746, 70.48412626434020467 ) ) ;
#1445 = VECTOR ( 'NONE', #43605, 1000.000000000000000 ) ;
#1446 = AXIS2_PLACEMENT_3D ( 'NONE', #48714, #34408, #463 ) ;
#1447 = VERTEX_POINT ( 'NONE', #24199 ) ;
#1448 = CARTESIAN_POINT ( 'NONE',  ( -12.23301264461619553, -10.03852782535897958, 60.84446034103241630 ) ) ;
#1449 = CARTESIAN_POINT ( 'NONE',  ( -23.78758865751629514, -10.93498413477609255, 73.40547355347567304 ) ) ;
#1450 = CARTESIAN_POINT ( 'NONE',  ( -45.92409385541306222, -13.70421070448076861, 68.24000000000000909 ) ) ;
#1451 = CARTESIAN_POINT ( 'NONE',  ( -13.88719209496301943, -21.36615830865247645, 72.11881843497792488 ) ) ;
#1452 = AXIS2_PLACEMENT_3D ( 'NONE', #39269, #42964, #17079 ) ;
#1453 = ORIENTED_EDGE ( 'NONE', *, *, #1885, .F. ) ;
#1454 = CARTESIAN_POINT ( 'NONE',  ( -24.44689184067228638, -14.18710713894228093, 69.93803194250310185 ) ) ;
#1455 = LINE ( 'NONE', #16465, #14102 ) ;
#1456 = EDGE_LOOP ( 'NONE', ( #20244, #40710 ) ) ;
#1457 = CARTESIAN_POINT ( 'NONE',  ( -22.62555253132729050, -20.14304347834919540, 69.33564472231955733 ) ) ;
#1458 = CARTESIAN_POINT ( 'NONE',  ( -13.91686182480500200, -8.236299899141551251, 74.31459327626868117 ) ) ;
#1459 = EDGE_CURVE ( 'NONE', #35558, #25977, #35780, .T. ) ;
#1460 = VERTEX_POINT ( 'NONE', #47088 ) ;
#1461 = CARTESIAN_POINT ( 'NONE',  ( -10.49786169981450712, -13.78684623552789290, 57.67654978352396000 ) ) ;
#1462 = ORIENTED_EDGE ( 'NONE', *, *, #34088, .F. ) ;
#1463 = CARTESIAN_POINT ( 'NONE',  ( -17.15534385759799108, -8.623186033802570094, 49.24843789510466507 ) ) ;
#1464 = CARTESIAN_POINT ( 'NONE',  ( -10.42407743915653562, -14.83384553516632032, 71.40070817709548123 ) ) ;
#1465 = ORIENTED_EDGE ( 'NONE', *, *, #36181, .F. ) ;
#1466 = CARTESIAN_POINT ( 'NONE',  ( -10.70566809389435647, -16.94585225683366048, 57.68760548748759476 ) ) ;
#1467 = ADVANCED_FACE ( 'NONE', ( #5493 ), #1787, .T. ) ;
#1468 = CARTESIAN_POINT ( 'NONE',  ( -21.79028809537168243, -9.273590339475653366, 63.47681654923867711 ) ) ;
#1469 = CARTESIAN_POINT ( 'NONE',  ( -16.64909385650551599, -8.104110260919579645, 48.81699501597546487 ) ) ;
#1470 = AXIS2_PLACEMENT_3D ( 'NONE', #1230, #23414, #38667 ) ;
#1471 = ORIENTED_EDGE ( 'NONE', *, *, #41370, .T. ) ;
#1472 = DIRECTION ( 'NONE',  ( 0.000000000000000000, 0.000000000000000000, 1.000000000000000000 ) ) ;
#1473 =( BOUNDED_CURVE ( )  B_SPLINE_CURVE ( 3, ( #20747, #32073, #35025, #24694 ),
 .UNSPECIFIED., .F., .F. ) 
 B_SPLINE_CURVE_WITH_KNOTS ( ( 4, 4 ),
 ( 0.5000000000000000000, 0.9074455897393608472 ),
 .UNSPECIFIED. ) 
 CURVE ( )  GEOMETRIC_REPRESENTATION_ITEM ( )  RATIONAL_B_SPLINE_CURVE ( ( 0.9999999999999960032, 0.4567392136813388515, 0.3561768502900354849, 0.6983129098260817402 ) ) 
 REPRESENTATION_ITEM ( '' )  );
#1474 = AXIS2_PLACEMENT_3D ( 'NONE', #30595, #38435, #12586 ) ;
#1475 = CARTESIAN_POINT ( 'NONE',  ( -24.10630238842451689, -12.71861100898961361, 73.35298647045775056 ) ) ;
#1476 = CARTESIAN_POINT ( 'NONE',  ( -14.73375663737576247, -21.75657035701089370, 61.75105113489106401 ) ) ;
#1477 = ORIENTED_EDGE ( 'NONE', *, *, #13657, .F. ) ;
#1478 = CARTESIAN_POINT ( 'NONE',  ( -23.89140331848801679, -17.48778192296385470, 62.70034397296751649 ) ) ;
#1479 = AXIS2_PLACEMENT_3D ( 'NONE', #19965, #27346, #5685 ) ;
#1480 = AXIS2_PLACEMENT_3D ( 'NONE', #39435, #35962, #6664 ) ;
#1481 = CARTESIAN_POINT ( 'NONE',  ( -11.42962537269896117, -10.38539323336976494, 74.62380298385740218 ) ) ;
#1482 = DIRECTION ( 'NONE',  ( 0.9687793358424821033, -0.2479245821708677133, 0.000000000000000000 ) ) ;
#1483 = CARTESIAN_POINT ( 'NONE',  ( -20.52907107024056188, -8.037074714175183487, 66.88080459870857908 ) ) ;
#1484 = CARTESIAN_POINT ( 'NONE',  ( -24.77597654615908240, -16.01465712210608316, 66.25599054112966257 ) ) ;
#1485 = ORIENTED_EDGE ( 'NONE', *, *, #10961, .T. ) ;
#1486 = ORIENTED_EDGE ( 'NONE', *, *, #25832, .T. ) ;
#1487 = EDGE_CURVE ( 'NONE', #15891, #24038, #38965, .T. ) ;
#1488 = CARTESIAN_POINT ( 'NONE',  ( -21.36950980536903444, -9.026885639815656504, 73.60128804931920854 ) ) ;
#1489 = CARTESIAN_POINT ( 'NONE',  ( -24.29232374648589854, -16.16102685949518403, 62.89328677060923667 ) ) ;
#1490 = ORIENTED_EDGE ( 'NONE', *, *, #35013, .F. ) ;
#1491 = CARTESIAN_POINT ( 'NONE',  ( -15.04196850781542594, -10.13074752191075234, 52.02966884056656482 ) ) ;
#1492 = CARTESIAN_POINT ( 'NONE',  ( -21.94242186726961208, -9.397052521110282441, 60.00699132926281010 ) ) ;
#1493 = VECTOR ( 'NONE', #7923, 1000.000000000000000 ) ;
#1494 = CARTESIAN_POINT ( 'NONE',  ( -10.27146132483092522, -12.72493829394020892, 64.39023348442692907 ) ) ;
#1495 = EDGE_CURVE ( 'NONE', #25885, #2066, #44599, .T. ) ;
#1496 = CARTESIAN_POINT ( 'NONE',  ( -23.82727386091907462, -11.00084565854733043, 73.54006079994626077 ) ) ;
#1497 = CARTESIAN_POINT ( 'NONE',  ( -11.01197672498280866, -17.74032467813711378, 71.85246142747085685 ) ) ;
#1498 = CARTESIAN_POINT ( 'NONE',  ( -16.27008412796014625, -7.904986034540439022, 60.20028479263386600 ) ) ;
#1499 = VERTEX_POINT ( 'NONE', #23961 ) ;
#1500 = ADVANCED_FACE ( 'NONE', ( #20981 ), #32543, .T. ) ;
#1501 = CARTESIAN_POINT ( 'NONE',  ( -16.43513463834741728, -22.19403045546258468, 65.41219756188628764 ) ) ;
#1502 = CARTESIAN_POINT ( 'NONE',  ( -19.30978178441422699, -7.601027468210772575, 63.61744607541091767 ) ) ;
#1503 = CARTESIAN_POINT ( 'NONE',  ( -24.34502428176253019, -17.56683243011407924, 66.12852677468319484 ) ) ;
#1504 = CARTESIAN_POINT ( 'NONE',  ( -19.85890256509918572, -21.37233786973231275, 68.95612130754568625 ) ) ;
#1505 = CARTESIAN_POINT ( 'NONE',  ( -12.72909380574049187, -20.00294183919138291, 71.87823903238121659 ) ) ;
#1506 = EDGE_CURVE ( 'NONE', #21704, #39406, #13569, .T. ) ;
#1507 = B_SPLINE_CURVE_WITH_KNOTS ( 'NONE', 3,
 ( #9863, #43104, #32276, #5696, #5922, #46803, #28080, #16977, #1749, #12581 ),
 .UNSPECIFIED., .F., .F.,
 ( 4, 2, 2, 2, 4 ),
 ( 0.000000000000000000, 0.2500000000000000000, 0.5000000000000000000, 0.7500000000000000000, 1.000000000000000000 ),
 .UNSPECIFIED. ) ;
#1508 = ORIENTED_EDGE ( 'NONE', *, *, #17222, .F. ) ;
#1509 = VERTEX_POINT ( 'NONE', #6205 ) ;
#1510 = VERTEX_POINT ( 'NONE', #35983 ) ;
#1511 = B_SPLINE_CURVE_WITH_KNOTS ( 'NONE', 1,
 ( #39387, #24131 ),
 .UNSPECIFIED., .F., .F.,
 ( 2, 2 ),
 ( 0.000000000000000000, 1.000000000000000000 ),
 .UNSPECIFIED. ) ;
#1512 = CARTESIAN_POINT ( 'NONE',  ( -24.47066272824306665, -14.57993217219608795, 62.99824437345093031 ) ) ;
#1513 = CARTESIAN_POINT ( 'NONE',  ( -19.98813031515369332, -21.37641424997302053, 72.70478737316020101 ) ) ;
#1514 = ORIENTED_EDGE ( 'NONE', *, *, #11665, .T. ) ;
#1515 = AXIS2_PLACEMENT_3D ( 'NONE', #48179, #29470, #40541 ) ;
#1516 = CIRCLE ( 'NONE', #751, 5.249999999999998224 ) ;
#1517 = CARTESIAN_POINT ( 'NONE',  ( -22.23733845922741637, -19.96043711175405733, 66.00421731380802726 ) ) ;
#1518 = CARTESIAN_POINT ( 'NONE',  ( -23.65624057141237202, -11.51332318074561911, 66.72214514605293800 ) ) ;
#1519 = ORIENTED_EDGE ( 'NONE', *, *, #553, .F. ) ;
#1520 = CARTESIAN_POINT ( 'NONE',  ( -10.63483715323753565, -17.87674169505483235, 71.75213630217804450 ) ) ;
#1521 = CIRCLE ( 'NONE', #10982, 4.686499999999998778 ) ;
#1522 = CARTESIAN_POINT ( 'NONE',  ( -23.17996796428253603, -10.73203099773195568, 59.69383679455673075 ) ) ;
#1523 = ORIENTED_EDGE ( 'NONE', *, *, #46433, .T. ) ;
#1524 =( BOUNDED_CURVE ( )  B_SPLINE_CURVE ( 3, ( #46875, #31367, #46397, #42710 ),
 .UNSPECIFIED., .F., .F. ) 
 B_SPLINE_CURVE_WITH_KNOTS ( ( 4, 4 ),
 ( 2.926239601924445180E-15, 0.1359452067163722244 ),
 .UNSPECIFIED. ) 
 CURVE ( )  GEOMETRIC_REPRESENTATION_ITEM ( )  RATIONAL_B_SPLINE_CURVE ( ( 1.000000000000000000, 0.9984605012767909793, 0.9984605012767909793, 1.000000000000000000 ) ) 
 REPRESENTATION_ITEM ( '' )  );
#1525 = DIRECTION ( 'NONE',  ( 0.9687793358424821033, -0.2479245821708680464, 0.000000000000000000 ) ) ;
#1526 = EDGE_CURVE ( 'NONE', #35369, #1693, #24644, .T. ) ;
#1527 = CARTESIAN_POINT ( 'NONE',  ( -10.13628521134413774, -13.26287664204559391, 74.78543499488121427 ) ) ;
#1528 = ORIENTED_EDGE ( 'NONE', *, *, #27294, .F. ) ;
#1529 = CARTESIAN_POINT ( 'NONE',  ( -16.02724665508026192, -7.491242618400526077, 63.78515750052793010 ) ) ;
#1530 = CARTESIAN_POINT ( 'NONE',  ( -19.17604249790256077, -21.63836284480991878, 58.53979515915469278 ) ) ;
#1531 = VERTEX_POINT ( 'NONE', #39455 ) ;
#1532 = CARTESIAN_POINT ( 'NONE',  ( -24.24515474721203745, -17.80517362172114559, 62.57386731182483430 ) ) ;
#1533 = CARTESIAN_POINT ( 'NONE',  ( -9.979603215878100286, -14.52052451035377345, 68.04295550616701860 ) ) ;
#1534 = CARTESIAN_POINT ( 'NONE',  ( -19.49109506855409180, -21.54969648977046148, 62.28031529404344013 ) ) ;
#1535 = CARTESIAN_POINT ( 'NONE',  ( -15.45014681279580238, -8.041036458835323586, 74.37425853534905684 ) ) ;
#1536 = CARTESIAN_POINT ( 'NONE',  ( -21.24554520941113367, -21.20453976546471608, 65.76949229983627276 ) ) ;
#1537 = CARTESIAN_POINT ( 'NONE',  ( -20.52513369171654745, -21.08626508430529611, 58.71645414705509580 ) ) ;
#1538 = VERTEX_POINT ( 'NONE', #2021 ) ;
#1540 =( BOUNDED_SURFACE ( )  B_SPLINE_SURFACE ( 3, 1, ( 
 ( #28727, #2623 ),
 ( #39139, #5422 ),
 ( #36344, #4945 ),
 ( #36099, #998 ),
 ( #2381, #17394 ),
 ( #12313, #43760 ),
 ( #46301, #10014 ) ),
 .UNSPECIFIED., .T., .F., .F. ) 
 B_SPLINE_SURFACE_WITH_KNOTS ( ( 4, 3, 4 ),
 ( 2, 2 ),
 ( 0.000000000000000000, 0.5000000000000000000, 1.000000000000000000 ),
 ( 0.000000000000000000, 1.000000000000000000 ),
 .UNSPECIFIED. ) 
 GEOMETRIC_REPRESENTATION_ITEM ( )  RATIONAL_B_SPLINE_SURFACE ( (
 ( 1.000000000000000000, 1.000000000000000000),
 ( 0.3333333333333335369, 0.3333333333333330373),
 ( 0.3333333333333335369, 0.3333333333333330373),
 ( 1.000000000000000000, 1.000000000000000000),
 ( 0.3333333333333333703, 0.3333333333333333703),
 ( 0.3333333333333333703, 0.3333333333333333703),
 ( 1.000000000000000000, 1.000000000000000000) ) ) 
 REPRESENTATION_ITEM ( '' )  SURFACE ( )  );
#1539 = DIRECTION ( 'NONE',  ( -0.6380325334150318550, 0.7700094066334490783, 0.000000000000000000 ) ) ;
#1541 = CARTESIAN_POINT ( 'NONE',  ( -28.42409385541305511, -6.859206544744110623, 47.99999999999997868 ) ) ;
#1542 = CARTESIAN_POINT ( 'NONE',  ( -16.23116076413911557, -7.455249184188991407, 60.31533086125586607 ) ) ;
#1543 = DIRECTION ( 'NONE',  ( -9.637352644315596475E-17, 0.000000000000000000, -1.000000000000000000 ) ) ;
#1544 = CARTESIAN_POINT ( 'NONE',  ( -22.07022430586338402, -11.86582892075562334, 54.07175714974878389 ) ) ;
#1545 = CARTESIAN_POINT ( 'NONE',  ( -15.38034385650552061, -6.424090610841176385, 49.80797279389978627 ) ) ;
#1546 = ORIENTED_EDGE ( 'NONE', *, *, #18949, .F. ) ;
#1547 = ADVANCED_FACE ( 'NONE', ( #5737 ), #42910, .T. ) ;
#1548 = VECTOR ( 'NONE', #1329, 1000.000000000000000 ) ;
#1549 = CARTESIAN_POINT ( 'NONE',  ( -17.90106345612152694, -14.65920654474411045, 47.99999999999998579 ) ) ;
#1550 = CARTESIAN_POINT ( 'NONE',  ( -11.01935386438909426, -11.00369580034137229, 60.87896987096186763 ) ) ;
#1551 = ORIENTED_EDGE ( 'NONE', *, *, #20178, .T. ) ;
#1552 = CARTESIAN_POINT ( 'NONE',  ( -33.52409385541305653, -8.109206544744111511, 51.54999999999998295 ) ) ;
#1553 = DIRECTION ( 'NONE',  ( 0.2189141945955469237, -0.9757441136919980940, 0.000000000000000000 ) ) ;
#1554 = CARTESIAN_POINT ( 'NONE',  ( -17.98584164848810474, -22.23808382151284491, 62.06031347038508983 ) ) ;
#1555 = CARTESIAN_POINT ( 'NONE',  ( -45.46395726858714426, -13.72754205882879042, 70.87000000000000455 ) ) ;
#1556 = CARTESIAN_POINT ( 'NONE',  ( -16.94046182855944949, -22.24350478419641419, 72.26568972578677119 ) ) ;
#1557 = ORIENTED_EDGE ( 'NONE', *, *, #33788, .T. ) ;
#1558 = CARTESIAN_POINT ( 'NONE',  ( -23.73600443614001776, -11.78168025344282555, 63.23601694537735085 ) ) ;
#1559 = AXIS2_PLACEMENT_3D ( 'NONE', #31240, #24098, #39593 ) ;
#1560 = CARTESIAN_POINT ( 'NONE',  ( -16.26183941974026581, -7.855670460422400581, 60.35028478908645155 ) ) ;
#1561 = EDGE_CURVE ( 'NONE', #1863, #1410, #13329, .T. ) ;
#1562 = CYLINDRICAL_SURFACE ( 'NONE', #14930, 0.1499999999999990508 ) ;
#1563 = VERTEX_POINT ( 'NONE', #43644 ) ;
#1564 = DIRECTION ( 'NONE',  ( -3.071710424422018668E-17, 6.404604876783312462E-16, 1.000000000000000000 ) ) ;
#1565 = EDGE_CURVE ( 'NONE', #24279, #997, #4665, .T. ) ;
#1566 = CARTESIAN_POINT ( 'NONE',  ( -23.48885089983262020, -11.31111638938591568, 73.43363640969468520 ) ) ;
#1567 = CARTESIAN_POINT ( 'NONE',  ( -10.39693166811831304, -15.37990016280386740, 57.58264896457095006 ) ) ;
#1568 = CARTESIAN_POINT ( 'NONE',  ( -15.62222905942472018, -7.993050613273783966, 70.89517703929612935 ) ) ;
#1569 = CARTESIAN_POINT ( 'NONE',  ( -10.73729132840935740, -12.73729855581346371, 64.55219560051592964 ) ) ;
#1570 = EDGE_LOOP ( 'NONE', ( #22090, #16579, #22831, #22061 ) ) ;
#1571 = VERTEX_POINT ( 'NONE', #21228 ) ;
#1572 = CARTESIAN_POINT ( 'NONE',  ( -22.91784385541304303, -6.860780111191487229, 51.02154966934377001 ) ) ;
#1573 = CARTESIAN_POINT ( 'NONE',  ( -22.98291842025556164, -9.849094896122194243, 70.20516821032623511 ) ) ;
#1574 = CARTESIAN_POINT ( 'NONE',  ( -13.26872317195175199, -21.05283485551296607, 54.27966884056655061 ) ) ;
#1575 = EDGE_CURVE ( 'NONE', #17990, #7797, #36227, .T. ) ;
#1576 = ADVANCED_FACE ( 'NONE', ( #3229 ), #6684, .T. ) ;
#1577 = CARTESIAN_POINT ( 'NONE',  ( -14.23618716594424960, -8.577114723333041368, 71.02957618500911963 ) ) ;
#1578 = EDGE_CURVE ( 'NONE', #46443, #1741, #15049, .T. ) ;
#1579 = DIRECTION ( 'NONE',  ( -3.652049423109068320E-16, 1.190614954331866791E-16, -1.000000000000000000 ) ) ;
#1580 = B_SPLINE_CURVE_WITH_KNOTS ( 'NONE', 3,
 ( #11793, #26560, #45784, #18930, #12032, #3658, #27044, #30272, #15702, #8340 ),
 .UNSPECIFIED., .F., .F.,
 ( 4, 2, 2, 2, 4 ),
 ( 0.000000000000000000, 0.2500000000000000000, 0.5000000000000000000, 0.7500000000000000000, 1.000000000000000000 ),
 .UNSPECIFIED. ) ;
#1581 = AXIS2_PLACEMENT_3D ( 'NONE', #30557, #11835, #11343 ) ;
#1582 = FACE_OUTER_BOUND ( 'NONE', #1299, .T. ) ;
#1583 = CIRCLE ( 'NONE', #36959, 1.999999999999999556 ) ;
#1584 = CARTESIAN_POINT ( 'NONE',  ( -18.18338144371267617, -21.81849904615365432, 65.63060065626805795 ) ) ;
#1585 = ORIENTED_EDGE ( 'NONE', *, *, #46453, .F. ) ;
#1586 = CARTESIAN_POINT ( 'NONE',  ( -23.94599579101543796, -17.50730996363388314, 59.15945600998260545 ) ) ;
#1587 = VECTOR ( 'NONE', #20656, 1000.000000000000000 ) ;
#1588 = DIRECTION ( 'NONE',  ( 6.493791346278465266E-22, 1.084253996632606248E-42, -1.000000000000000000 ) ) ;
#1590 = VERTEX_POINT ( 'NONE', #47801 ) ;
#1589 =( BOUNDED_CURVE ( )  B_SPLINE_CURVE ( 3, ( #26328, #41341, #26575, #7634 ),
 .UNSPECIFIED., .F., .F. ) 
 B_SPLINE_CURVE_WITH_KNOTS ( ( 4, 4 ),
 ( 0.4074455897393671755, 0.5000000000000000000 ),
 .UNSPECIFIED. ) 
 CURVE ( )  GEOMETRIC_REPRESENTATION_ITEM ( )  RATIONAL_B_SPLINE_CURVE ( ( 0.6983129098261091627, 0.7760317562607096376, 0.8765941196520059542, 0.9999999999999961142 ) ) 
 REPRESENTATION_ITEM ( '' )  );
#1591 = DIRECTION ( 'NONE',  ( 0.9858639740050647582, 0.1675476790616363121, 8.494556375077916271E-17 ) ) ;
#1592 = CARTESIAN_POINT ( 'NONE',  ( -11.30598245021123560, -18.31969919398564528, 61.57711092061642688 ) ) ;
#1593 = ORIENTED_EDGE ( 'NONE', *, *, #25907, .F. ) ;
#1594 = CARTESIAN_POINT ( 'NONE',  ( -35.42409385541304800, -8.109206544743658540, 50.50000000000030553 ) ) ;
#1595 = PLANE ( 'NONE',  #42242 ) ;
#1596 = AXIS2_PLACEMENT_3D ( 'NONE', #28882, #21509, #13601 ) ;
#1597 = LINE ( 'NONE', #38043, #29795 ) ;
#1598 = CARTESIAN_POINT ( 'NONE',  ( -24.47217469005601131, -14.64471752244405067, 62.71296487297676947 ) ) ;
#1599 = EDGE_LOOP ( 'NONE', ( #1789, #47994, #48137, #2642, #27619 ) ) ;
#1600 = B_SPLINE_CURVE_WITH_KNOTS ( 'NONE', 1,
 ( #12862, #38970 ),
 .UNSPECIFIED., .F., .F.,
 ( 2, 2 ),
 ( 0.000000000000000000, 1.000000000000000000 ),
 .UNSPECIFIED. ) ;
#1601 = CARTESIAN_POINT ( 'NONE',  ( -18.53714847821261458, -22.17566945187693506, 72.54156883610106377 ) ) ;
#1602 = CARTESIAN_POINT ( 'NONE',  ( -24.37683822056718697, -15.97618770311995462, 66.06324926631656069 ) ) ;
#1603 = CARTESIAN_POINT ( 'NONE',  ( -16.45566506110110438, -21.79267588865899086, 62.04095995016087528 ) ) ;
#1604 = FACE_BOUND ( 'NONE', #24485, .T. ) ;
#1605 = CYLINDRICAL_SURFACE ( 'NONE', #36816, 1.999999999999999556 ) ;
#1606 = CARTESIAN_POINT ( 'NONE',  ( -17.50157081909136991, -7.358860168393607459, 67.20694839074946003 ) ) ;
#1607 = CARTESIAN_POINT ( 'NONE',  ( -16.00544582274271477, -7.903112417841744453, 63.95538887075813506 ) ) ;
#1608 = EDGE_LOOP ( 'NONE', ( #37377, #5794, #41248, #33507 ) ) ;
#1609 = FACE_OUTER_BOUND ( 'NONE', #22444, .T. ) ;
#1610 = ORIENTED_EDGE ( 'NONE', *, *, #4998, .T. ) ;
#1611 = CARTESIAN_POINT ( 'NONE',  ( -11.45656716003344933, -19.26928393672501727, 71.73039932227760573 ) ) ;
#1612 = CARTESIAN_POINT ( 'NONE',  ( -13.30358910455570332, -20.46953808992088852, 58.27480040995169475 ) ) ;
#1613 = ORIENTED_EDGE ( 'NONE', *, *, #20351, .F. ) ;
#1614 = CARTESIAN_POINT ( 'NONE',  ( -16.84865286310842336, -21.83598151670433296, 68.98088545748413480 ) ) ;
#1615 = CARTESIAN_POINT ( 'NONE',  ( -12.75166747855125493, -9.006326174502946813, 71.01071880285634563 ) ) ;
#1616 = EDGE_CURVE ( 'NONE', #42061, #46061, #37166, .T. ) ;
#1617 = ORIENTED_EDGE ( 'NONE', *, *, #34829, .T. ) ;
#1618 = ORIENTED_EDGE ( 'NONE', *, *, #4581, .F. ) ;
#1619 = ORIENTED_EDGE ( 'NONE', *, *, #3036, .F. ) ;
#1620 = EDGE_CURVE ( 'NONE', #2135, #40793, #37425, .T. ) ;
#1622 = CARTESIAN_POINT ( 'NONE',  ( -17.98657259272421172, -21.83703102787368167, 62.16063850355641307 ) ) ;
#1621 = VECTOR ( 'NONE', #33239, 1000.000000000000000 ) ;
#1623 = CARTESIAN_POINT ( 'NONE',  ( -24.43362379028604536, -14.05489247495133753, 73.12271507725591846 ) ) ;
#1624 = CARTESIAN_POINT ( 'NONE',  ( -21.33694466872984918, -9.004932385753821933, 73.90128753631783809 ) ) ;
#1625 = CARTESIAN_POINT ( 'NONE',  ( -11.85383375607109713, -9.861995938241047810, 64.12940074489686992 ) ) ;
#1626 = CARTESIAN_POINT ( 'NONE',  ( -42.18144679658952612, -14.80920654474417830, 64.94117647058821774 ) ) ;
#1627 = CIRCLE ( 'NONE', #22876, 4.686499999999998778 ) ;
#1628 = VERTEX_POINT ( 'NONE', #29831 ) ;
#1629 = VERTEX_POINT ( 'NONE', #17744 ) ;
#1630 = CYLINDRICAL_SURFACE ( 'NONE', #47769, 2.000000000000001332 ) ;
#1631 = DIRECTION ( 'NONE',  ( -0.5263399769092093061, 0.8502742079512979334, 7.678741024442198749E-08 ) ) ;
#1632 = CARTESIAN_POINT ( 'NONE',  ( -20.89788161767221197, -20.94431024770144489, 62.39999296070408974 ) ) ;
#1633 = CIRCLE ( 'NONE', #34671, 1.250000000000001110 ) ;
#1634 = CARTESIAN_POINT ( 'NONE',  ( -12.64995486802317082, -19.99670083032576429, 68.33657438322859434 ) ) ;
#1635 = CARTESIAN_POINT ( 'NONE',  ( -21.82409385650551670, -6.426201560718813433, 50.50509628382439331 ) ) ;
#1636 = ADVANCED_FACE ( 'NONE', ( #2977 ), #48524, .T. ) ;
#1637 = ORIENTED_EDGE ( 'NONE', *, *, #35530, .F. ) ;
#1638 = ADVANCED_FACE ( 'NONE', ( #48045 ), #14760, .T. ) ;
#1639 = ADVANCED_FACE ( 'NONE', ( #25163 ), #32775, .T. ) ;
#1640 = CARTESIAN_POINT ( 'NONE',  ( -23.02753126890070590, -10.61360989481728367, 59.90203474228974301 ) ) ;
#1641 = EDGE_CURVE ( 'NONE', #46610, #24230, #44142, .T. ) ;
#1642 = CARTESIAN_POINT ( 'NONE',  ( -23.83043773139749888, -11.86620498678314384, 59.78235732590889739 ) ) ;
#1643 = AXIS2_PLACEMENT_3D ( 'NONE', #40956, #37235, #2793 ) ;
#1644 = CARTESIAN_POINT ( 'NONE',  ( -12.43502697965553416, -19.72161038572663472, 64.97747870948867899 ) ) ;
#1645 = VERTEX_POINT ( 'NONE', #44857 ) ;
#1646 = CARTESIAN_POINT ( 'NONE',  ( -11.68335550665270794, -18.81469308649876737, 68.21689631955439381 ) ) ;
#1647 = VECTOR ( 'NONE', #12531, 1000.000000000000000 ) ;
#1648 = CARTESIAN_POINT ( 'NONE',  ( -9.974456290884534226, -14.72748455880875795, 71.51278017970571454 ) ) ;
#1649 = CARTESIAN_POINT ( 'NONE',  ( -21.40283924303304985, -8.989053705293313712, 73.60688577834839919 ) ) ;
#1650 = CARTESIAN_POINT ( 'NONE',  ( -14.40787616456130493, -7.996955972674248514, 63.91166111565177488 ) ) ;
#1651 = CIRCLE ( 'NONE', #4022, 7.500000000000002665 ) ;
#1652 = EDGE_LOOP ( 'NONE', ( #23167, #224 ) ) ;
#1653 = CARTESIAN_POINT ( 'NONE',  ( -14.30855566557790404, -8.484641631233271752, 70.74429704309763167 ) ) ;
#1654 = CARTESIAN_POINT ( 'NONE',  ( -24.82316860084702981, -15.68024280754056576, 73.14270404762098110 ) ) ;
#1655 = DIRECTION ( 'NONE',  ( 0.000000000000000000, -0.9999954153791272837, -0.003028072113821676185 ) ) ;
#1656 = VERTEX_POINT ( 'NONE', #25402 ) ;
#1657 = CARTESIAN_POINT ( 'NONE',  ( -10.00731251637046881, -14.10555026099538978, 61.10316585833331260 ) ) ;
#1658 = AXIS2_PLACEMENT_3D ( 'NONE', #41245, #48147, #22290 ) ;
#1659 = ORIENTED_EDGE ( 'NONE', *, *, #39608, .F. ) ;
#1660 = CARTESIAN_POINT ( 'NONE',  ( -19.16569461048236889, -7.565509106446075549, 63.55276450808027278 ) ) ;
#1661 = PLANE ( 'NONE',  #32724 ) ;
#1662 = VERTEX_POINT ( 'NONE', #29574 ) ;
#1663 = DIRECTION ( 'NONE',  ( -0.1539336739619741878, -0.9880811829098681276, -6.607022904161600477E-08 ) ) ;
#1665 = ADVANCED_FACE ( 'NONE', ( #7187 ), #10860, .T. ) ;
#1664 = CARTESIAN_POINT ( 'NONE',  ( -10.42492065060444872, -12.25670954885047692, 57.58503240040955262 ) ) ;
#1666 = CARTESIAN_POINT ( 'NONE',  ( -13.18362886651731358, -8.683667069837246899, 60.62445550483372614 ) ) ;
#1667 = PLANE ( 'NONE',  #25087 ) ;
#1668 = EDGE_LOOP ( 'NONE', ( #31560, #32124, #35953, #44439 ) ) ;
#1669 = FACE_OUTER_BOUND ( 'NONE', #19095, .T. ) ;
#1670 = AXIS2_PLACEMENT_3D ( 'NONE', #43867, #36919, #25140 ) ;
#1671 = UNCERTAINTY_MEASURE_WITH_UNIT (LENGTH_MEASURE( 1.000000000000000082E-05 ), #47548, 'distance_accuracy_value', 'NONE');
#1672 =( BOUNDED_CURVE ( )  B_SPLINE_CURVE ( 3, ( #30031, #34181, #23127, #7627 ),
 .UNSPECIFIED., .F., .F. ) 
 B_SPLINE_CURVE_WITH_KNOTS ( ( 4, 4 ),
 ( 0.5000000000000000000, 0.9074455897393662873 ),
 .UNSPECIFIED. ) 
 CURVE ( )  GEOMETRIC_REPRESENTATION_ITEM ( )  RATIONAL_B_SPLINE_CURVE ( ( 1.000000000000003553, 0.4567392136813320791, 0.3561768502900277689, 0.6983129098260943968 ) ) 
 REPRESENTATION_ITEM ( '' )  );
#1673 = CARTESIAN_POINT ( 'NONE',  ( -20.48427295952909688, -21.16374346551129548, 59.05963865090804887 ) ) ;
#1674 = CARTESIAN_POINT ( 'NONE',  ( -10.44503168371052837, -15.82779754136115002, 68.39256704124431963 ) ) ;
#1675 = ORIENTED_EDGE ( 'NONE', *, *, #18667, .F. ) ;
#1676 = CARTESIAN_POINT ( 'NONE',  ( -16.20274916913749408, -7.857711080649619539, 67.28440454693885897 ) ) ;
#1677 = CARTESIAN_POINT ( 'NONE',  ( -36.42409385541304800, -6.859212275519750435, 50.50378509014258555 ) ) ;
#1678 = EDGE_CURVE ( 'NONE', #36016, #25288, #21372, .T. ) ;
#1680 = ORIENTED_EDGE ( 'NONE', *, *, #28119, .F. ) ;
#1679 = VECTOR ( 'NONE', #28191, 1000.000000000000000 ) ;
#1681 = ORIENTED_EDGE ( 'NONE', *, *, #24884, .T. ) ;
#1682 = DIRECTION ( 'NONE',  ( -0.09332174201254901658, -0.9956360040033421788, 0.000000000000000000 ) ) ;
#1683 = EDGE_CURVE ( 'NONE', #6741, #11159, #44202, .T. ) ;
#1684 = DIRECTION ( 'NONE',  ( -2.866981220435666553E-17, 1.000000000000000000, 1.190614954331866791E-16 ) ) ;
#1685 = CARTESIAN_POINT ( 'NONE',  ( -19.03659385650551528, -6.915538690918074494, 49.31353937987644542 ) ) ;
#1686 = DIRECTION ( 'NONE',  ( -0.8201047403141396019, 0.5722134347551370848, 7.883065731424289661E-08 ) ) ;
#1687 =( BOUNDED_CURVE ( )  B_SPLINE_CURVE ( 2, ( #33353, #28309, #5415, #43074, #20434, #7049, #13020, #31754, #1720 ),
 .UNSPECIFIED., .F., .F. ) 
 B_SPLINE_CURVE_WITH_KNOTS ( ( 3, 2, 2, 2, 3 ),
 ( 0.000000000000000000, 0.01041666666666664007, 0.02083333333333328014, 0.03124999999999992020, 0.04166666666666656027 ),
 .UNSPECIFIED. ) 
 CURVE ( )  GEOMETRIC_REPRESENTATION_ITEM ( )  RATIONAL_B_SPLINE_CURVE ( ( 1.000000000000000000, 0.9238795325112867385, 1.000000000000000000, 0.9238795325112867385, 1.000000000000000000, 0.9238795325112867385, 1.000000000000000000, 0.9238795325112875156, 0.9999999999999992228 ) ) 
 REPRESENTATION_ITEM ( '' )  );
#1688 = CARTESIAN_POINT ( 'NONE',  ( -20.03282965983824226, -21.84088468745754597, 53.89198173725360874 ) ) ;
#1689 = CARTESIAN_POINT ( 'NONE',  ( -18.63772371551852913, -7.458595371860563539, 73.96347537936300398 ) ) ;
#1690 =( BOUNDED_SURFACE ( )  B_SPLINE_SURFACE ( 3, 1, ( 
 ( #31567, #12129 ),
 ( #24434, #8928 ),
 ( #12843, #32051 ),
 ( #1046, #27146 ),
 ( #31809, #23947 ),
 ( #38949, #16530 ),
 ( #28107, #46601 ) ),
 .UNSPECIFIED., .T., .F., .F. ) 
 B_SPLINE_SURFACE_WITH_KNOTS ( ( 4, 3, 4 ),
 ( 2, 2 ),
 ( 0.000000000000000000, 0.5000000000000000000, 1.000000000000000000 ),
 ( 0.000000000000000000, 1.000000000000000000 ),
 .UNSPECIFIED. ) 
 GEOMETRIC_REPRESENTATION_ITEM ( )  RATIONAL_B_SPLINE_SURFACE ( (
 ( 1.000000000000000000, 1.000000000000000000),
 ( 0.3333333333333335369, 0.3333333333333330373),
 ( 0.3333333333333335369, 0.3333333333333330373),
 ( 1.000000000000000000, 1.000000000000000000),
 ( 0.3333333333333333703, 0.3333333333333333703),
 ( 0.3333333333333333703, 0.3333333333333333703),
 ( 1.000000000000000000, 1.000000000000000000) ) ) 
 REPRESENTATION_ITEM ( '' )  SURFACE ( )  );
#1691 = FACE_OUTER_BOUND ( 'NONE', #46233, .T. ) ;
#1692 = VERTEX_POINT ( 'NONE', #18728 ) ;
#1693 = VERTEX_POINT ( 'NONE', #10623 ) ;
#1695 = FACE_OUTER_BOUND ( 'NONE', #989, .T. ) ;
#1694 = AXIS2_PLACEMENT_3D ( 'NONE', #37655, #18697, #48252 ) ;
#1696 =( NAMED_UNIT ( * ) SI_UNIT ( $, .STERADIAN. ) SOLID_ANGLE_UNIT ( ) );
#1697 = CARTESIAN_POINT ( 'NONE',  ( -36.42409385541304800, -6.859212275519750435, 50.50378509014258555 ) ) ;
#1698 = CARTESIAN_POINT ( 'NONE',  ( -19.81157080418587313, -21.44583120317290081, 65.34997476282926243 ) ) ;
#1699 = CARTESIAN_POINT ( 'NONE',  ( -17.42409385541299471, -14.80920654474435594, 52.02966884056656482 ) ) ;
#1700 = CARTESIAN_POINT ( 'NONE',  ( -11.10553262954647380, -11.79631758389720986, 71.08860856935916672 ) ) ;
#1701 = B_SPLINE_CURVE_WITH_KNOTS ( 'NONE', 3,
 ( #20000, #8923, #5221, #12838, #46822, #42165, #13066, #42415, #31076, #34769 ),
 .UNSPECIFIED., .F., .F.,
 ( 4, 2, 2, 2, 4 ),
 ( 0.000000000000000000, 0.2500000000000000000, 0.5000000000000000000, 0.7500000000000000000, 1.000000000000000000 ),
 .UNSPECIFIED. ) ;
#1702 =( BOUNDED_CURVE ( )  B_SPLINE_CURVE ( 2, ( #32253, #28315, #5669, #24857, #13978, #43581, #20918, #21413, #46778 ),
 .UNSPECIFIED., .F., .F. ) 
 B_SPLINE_CURVE_WITH_KNOTS ( ( 3, 2, 2, 2, 3 ),
 ( 0.7083333333333332593, 0.7187499999999998890, 0.7291666666666665186, 0.7395833333333333703, 0.7500000000000000000 ),
 .UNSPECIFIED. ) 
 CURVE ( )  GEOMETRIC_REPRESENTATION_ITEM ( )  RATIONAL_B_SPLINE_CURVE ( ( 1.000000000000000888, 0.9238795325112859613, 1.000000000000000000, 0.9238795325112867385, 1.000000000000000000, 0.9238795325112867385, 1.000000000000000000, 0.9238795325112867385, 1.000000000000000000 ) ) 
 REPRESENTATION_ITEM ( '' )  );
#1703 = ORIENTED_EDGE ( 'NONE', *, *, #4007, .T. ) ;
#1704 = EDGE_CURVE ( 'NONE', #3004, #2922, #3547, .T. ) ;
#1705 = EDGE_CURVE ( 'NONE', #16276, #23858, #39886, .T. ) ;
#1706 = CARTESIAN_POINT ( 'NONE',  ( -19.67573413203048460, -21.49838315979392789, 72.54911470401957274 ) ) ;
#1707 = DIRECTION ( 'NONE',  ( 0.000000000000000000, 1.000000000000000000, 0.000000000000000000 ) ) ;
#1708 = DIRECTION ( 'NONE',  ( 0.9687793358424819923, -0.2479245821708680464, 0.000000000000000000 ) ) ;
#1709 = AXIS2_PLACEMENT_3D ( 'NONE', #47970, #2666, #17905 ) ;
#1710 = VERTEX_POINT ( 'NONE', #41638 ) ;
#1711 = CARTESIAN_POINT ( 'NONE',  ( -10.55459683810411775, -16.15489166977095437, 68.20441073976071777 ) ) ;
#1712 = EDGE_CURVE ( 'NONE', #28108, #14347, #13600, .T. ) ;
#1713 = EDGE_CURVE ( 'NONE', #32365, #12722, #516, .T. ) ;
#1714 = DIRECTION ( 'NONE',  ( 0.9687793358424819923, -0.2479245821708680464, 0.000000000000000000 ) ) ;
#1715 = AXIS2_PLACEMENT_3D ( 'NONE', #16235, #38165, #8642 ) ;
#1716 = EDGE_CURVE ( 'NONE', #43657, #11090, #15757, .T. ) ;
#1717 = B_SPLINE_CURVE_WITH_KNOTS ( 'NONE', 1,
 ( #29535, #22159 ),
 .UNSPECIFIED., .F., .F.,
 ( 2, 2 ),
 ( 0.000000000000000000, 1.000000000000000000 ),
 .UNSPECIFIED. ) ;
#1718 = CARTESIAN_POINT ( 'NONE',  ( -24.42364818358896272, -14.92042579261047131, 59.25916823501875541 ) ) ;
#1719 = FACE_OUTER_BOUND ( 'NONE', #11856, .T. ) ;
#1720 = CARTESIAN_POINT ( 'NONE',  ( -22.27409385759798965, -6.859212275519751323, 50.50378509014259265 ) ) ;
#1721 = ORIENTED_EDGE ( 'NONE', *, *, #16188, .T. ) ;
#1722 = CARTESIAN_POINT ( 'NONE',  ( -20.30948038729556515, -7.940514767581826838, 70.42817259598375301 ) ) ;
#1723 = ORIENTED_EDGE ( 'NONE', *, *, #13237, .T. ) ;
#1724 = CARTESIAN_POINT ( 'NONE',  ( -19.19606154404358378, -7.572994735369867669, 63.63078005410717708 ) ) ;
#1725 = CARTESIAN_POINT ( 'NONE',  ( -18.66311988809301425, -7.868636481342422329, 70.65595886192740238 ) ) ;
#1726 = EDGE_LOOP ( 'NONE', ( #16385, #30504, #28035, #30614 ) ) ;
#1727 = DIRECTION ( 'NONE',  ( 1.000000000000000000, 2.866981220435666553E-17, 0.000000000000000000 ) ) ;
#1728 = EDGE_CURVE ( 'NONE', #2748, #17620, #30813, .T. ) ;
#1729 = CARTESIAN_POINT ( 'NONE',  ( -16.31159385650551386, -6.922745924619793101, 51.69366785382590024 ) ) ;
#1730 = AXIS2_PLACEMENT_3D ( 'NONE', #10893, #311, #44637 ) ;
#1731 = VERTEX_POINT ( 'NONE', #41886 ) ;
#1732 = CARTESIAN_POINT ( 'NONE',  ( -24.43107140960042756, -14.03117428492017105, 73.42271492810181144 ) ) ;
#1733 = CARTESIAN_POINT ( 'NONE',  ( -24.10630227758727173, -12.71861067290860703, 73.43152628679671068 ) ) ;
#1734 = CARTESIAN_POINT ( 'NONE',  ( -13.62541112515491903, -8.865852518713435160, 60.53130564717850604 ) ) ;
#1735 = ORIENTED_EDGE ( 'NONE', *, *, #9269, .T. ) ;
#1736 = CARTESIAN_POINT ( 'NONE',  ( -23.89679824780917627, -17.47455792287359344, 62.58247085085636030 ) ) ;
#1737 = CARTESIAN_POINT ( 'NONE',  ( -10.42394424466950476, -17.36098423042032124, 64.81394647623933736 ) ) ;
#1738 = CARTESIAN_POINT ( 'NONE',  ( -7.924093855413094190, -6.859206544744110623, 64.00000000000002842 ) ) ;
#1739 = CARTESIAN_POINT ( 'NONE',  ( -23.44980453451080749, -18.46889374286061525, 73.06368236440982855 ) ) ;
#1740 = DIRECTION ( 'NONE',  ( -3.071710424422018668E-17, 6.404604876783312462E-16, 1.000000000000000000 ) ) ;
#1741 = VERTEX_POINT ( 'NONE', #34729 ) ;
#1742 = ORIENTED_EDGE ( 'NONE', *, *, #4645, .T. ) ;
#1743 = CARTESIAN_POINT ( 'NONE',  ( -23.81024829756716343, -18.64597716098235836, 72.94863620959463901 ) ) ;
#1744 = FACE_OUTER_BOUND ( 'NONE', #26665, .T. ) ;
#1745 = ORIENTED_EDGE ( 'NONE', *, *, #45560, .T. ) ;
#1746 = CARTESIAN_POINT ( 'NONE',  ( -24.33988733120284564, -15.89210004164691092, 66.34859510278248251 ) ) ;
#1747 = CARTESIAN_POINT ( 'NONE',  ( -10.66703363856100317, -12.79807828486586629, 64.26836111018113229 ) ) ;
#1748 = CARTESIAN_POINT ( 'NONE',  ( -18.16784385759799392, -9.357632978295830739, 49.97845033065684106 ) ) ;
#1749 = CARTESIAN_POINT ( 'NONE',  ( -10.42512903781134881, -14.93652116780334893, 75.09778865157521466 ) ) ;
#1750 = DIRECTION ( 'NONE',  ( -3.071710424422018668E-17, 6.404604876783312462E-16, 1.000000000000000000 ) ) ;
#1751 = CARTESIAN_POINT ( 'NONE',  ( -19.23866403772855449, -21.62168293227472660, 58.67507384656568092 ) ) ;
#1752 = VERTEX_POINT ( 'NONE', #34962 ) ;
#1753 = CARTESIAN_POINT ( 'NONE',  ( -16.64495962069230117, -22.21910613783234822, 65.33909019606271329 ) ) ;
#1754 = CARTESIAN_POINT ( 'NONE',  ( -10.42334091404133645, -15.64104667191196185, 61.33789045260130024 ) ) ;
#1755 = CARTESIAN_POINT ( 'NONE',  ( 18.46573386768564973, 0.6652513346184721899, 50.77657095919170871 ) ) ;
#1756 = CARTESIAN_POINT ( 'NONE',  ( -22.79960237261627398, -9.650942640399760464, 73.66656521964461035 ) ) ;
#1757 = DIRECTION ( 'NONE',  ( 0.9687793358424821033, -0.2479245821708679909, 0.000000000000000000 ) ) ;
#1758 = EDGE_CURVE ( 'NONE', #11201, #12343, #4218, .T. ) ;
#1759 = EDGE_LOOP ( 'NONE', ( #35753, #14719 ) ) ;
#1760 = ORIENTED_EDGE ( 'NONE', *, *, #5934, .F. ) ;
#1761 = ORIENTED_EDGE ( 'NONE', *, *, #21839, .T. ) ;
#1762 = EDGE_CURVE ( 'NONE', #9814, #25893, #21566, .T. ) ;
#1763 = CARTESIAN_POINT ( 'NONE',  ( -17.63706249495991685, -7.362172851917661909, 63.80702937774674410 ) ) ;
#1764 = FACE_OUTER_BOUND ( 'NONE', #6246, .T. ) ;
#1765 = CARTESIAN_POINT ( 'NONE',  ( -21.70346447568910264, -9.269547348209590254, 63.26441786439349357 ) ) ;
#1766 = ORIENTED_EDGE ( 'NONE', *, *, #35518, .F. ) ;
#1767 = CARTESIAN_POINT ( 'NONE',  ( -21.63336539757928634, -9.153348366551478321, 66.94677872351418557 ) ) ;
#1768 = EDGE_CURVE ( 'NONE', #9708, #19538, #43282, .T. ) ;
#1769 = LINE ( 'NONE', #1518, #6831 ) ;
#1770 = ORIENTED_EDGE ( 'NONE', *, *, #47997, .F. ) ;
#1771 = EDGE_CURVE ( 'NONE', #4886, #36512, #119, .T. ) ;
#1772 =( BOUNDED_SURFACE ( )  B_SPLINE_SURFACE ( 3, 1, ( 
 ( #43639, #33236 ),
 ( #28843, #17509 ),
 ( #2733, #3224 ),
 ( #2506, #9901 ),
 ( #17741, #44598 ),
 ( #29086, #25878 ),
 ( #40892, #10139 ) ),
 .UNSPECIFIED., .T., .F., .F. ) 
 B_SPLINE_SURFACE_WITH_KNOTS ( ( 4, 3, 4 ),
 ( 2, 2 ),
 ( 0.000000000000000000, 0.5000000000000000000, 1.000000000000000000 ),
 ( 0.000000000000000000, 1.000000000000000000 ),
 .UNSPECIFIED. ) 
 GEOMETRIC_REPRESENTATION_ITEM ( )  RATIONAL_B_SPLINE_SURFACE ( (
 ( 1.000000000000000000, 1.000000000000000000),
 ( 0.3333333333333335369, 0.3333333333333330373),
 ( 0.3333333333333335369, 0.3333333333333330373),
 ( 1.000000000000000000, 1.000000000000000000),
 ( 0.3333333333333333703, 0.3333333333333333703),
 ( 0.3333333333333333703, 0.3333333333333333703),
 ( 1.000000000000000000, 1.000000000000000000) ) ) 
 REPRESENTATION_ITEM ( '' )  SURFACE ( )  );
#1773 = CARTESIAN_POINT ( 'NONE',  ( -23.83833621072449560, -17.61232891644574394, 62.47360984984814536 ) ) ;
#1774 = EDGE_CURVE ( 'NONE', #32600, #15426, #22965, .T. ) ;
#1775 = ORIENTED_EDGE ( 'NONE', *, *, #19161, .T. ) ;
#1776 = CARTESIAN_POINT ( 'NONE',  ( -10.81118781404325446, -12.51348630141821339, 57.61392014802877526 ) ) ;
#1777 = ORIENTED_EDGE ( 'NONE', *, *, #43793, .T. ) ;
#1778 = CARTESIAN_POINT ( 'NONE',  ( -10.55941254297143672, -13.20321188299672066, 71.50828559427667130 ) ) ;
#1779 = VERTEX_POINT ( 'NONE', #45340 ) ;
#1780 = CARTESIAN_POINT ( 'NONE',  ( -15.88847107554206062, -7.518423027132939751, 63.78355628068795369 ) ) ;
#1781 = CARTESIAN_POINT ( 'NONE',  ( -13.43921569888383694, -8.993430976374535035, 60.58950277493168812 ) ) ;
#1782 = ORIENTED_EDGE ( 'NONE', *, *, #41587, .T. ) ;
#1783 = DIRECTION ( 'NONE',  ( -3.549360974554993999E-17, 6.371834667797928663E-18, 1.000000000000000000 ) ) ;
#1784 = CARTESIAN_POINT ( 'NONE',  ( -14.62732312719877115, -7.904084895095371266, 60.51985068470025908 ) ) ;
#1785 = CARTESIAN_POINT ( 'NONE',  ( -17.42409385541299471, -14.80920654474434883, 62.02966884056656482 ) ) ;
#1786 = CARTESIAN_POINT ( 'NONE',  ( -12.64995486802316904, -19.99670083032576429, 68.33657438322859434 ) ) ;
#1787 = CYLINDRICAL_SURFACE ( 'NONE', #19009, 1.500000000000001332 ) ;
#1788 = CARTESIAN_POINT ( 'NONE',  ( -11.93522140360746242, -14.45952210441258501, 53.49899999999994549 ) ) ;
#1789 = ORIENTED_EDGE ( 'NONE', *, *, #26530, .F. ) ;
#1790 = CARTESIAN_POINT ( 'NONE',  ( -17.55070634552562581, -7.810229109950414639, 63.55057029484540010 ) ) ;
#1791 = CARTESIAN_POINT ( 'NONE',  ( -11.88868080670210503, -19.09397054066711164, 71.87788967464850032 ) ) ;
#1792 = CARTESIAN_POINT ( 'NONE',  ( -14.09463846823036981, -8.088735815341543400, 54.27966884056655061 ) ) ;
#1793 = CARTESIAN_POINT ( 'NONE',  ( -14.39716994511728387, -8.437976179034702540, 63.78978877716816243 ) ) ;
#1794 = CARTESIAN_POINT ( 'NONE',  ( -16.34301583228449317, -10.23680828416977384, 52.02966884056656482 ) ) ;
#1795 = CARTESIAN_POINT ( 'NONE',  ( -17.51784385650551812, -9.790100578890868377, 49.79778022625163203 ) ) ;
#1796 = ORIENTED_EDGE ( 'NONE', *, *, #30506, .T. ) ;
#1797 = CARTESIAN_POINT ( 'NONE',  ( -21.06702863216100141, -20.84540773593991148, 65.86981821684420879 ) ) ;
#1798 = CARTESIAN_POINT ( 'NONE',  ( -24.43827367352892210, -15.52193379869737377, 73.28831629023289906 ) ) ;
#1799 = ORIENTED_EDGE ( 'NONE', *, *, #28644, .T. ) ;
#1800 = CARTESIAN_POINT ( 'NONE',  ( -11.33476804054750531, -19.10151225439055978, 68.40184904730287485 ) ) ;
#1801 = DIRECTION ( 'NONE',  ( -7.357566627711770083E-06, -1.068273751865974396E-05, 0.9999999999158726283 ) ) ;
#1802 = CARTESIAN_POINT ( 'NONE',  ( -22.93054552543627977, -10.40195957496224644, 66.95671006072360854 ) ) ;
#1803 = CARTESIAN_POINT ( 'NONE',  ( -19.36518065869528726, -8.031383756764064685, 59.97565108339750850 ) ) ;
#1804 = CARTESIAN_POINT ( 'NONE',  ( -15.47038452772150841, -21.58309165278561537, 72.04575460769355288 ) ) ;
#1805 = ORIENTED_EDGE ( 'NONE', *, *, #45521, .F. ) ;
#1806 = CARTESIAN_POINT ( 'NONE',  ( -12.09877737032034872, -9.599088377814357642, 57.21122801541561387 ) ) ;
#1807 = CARTESIAN_POINT ( 'NONE',  ( -17.01596658974409593, -7.370308080546169371, 74.07522964315150205 ) ) ;
#1808 = FACE_OUTER_BOUND ( 'NONE', #20776, .T. ) ;
#1809 = ORIENTED_EDGE ( 'NONE', *, *, #35759, .T. ) ;
#1810 = CARTESIAN_POINT ( 'NONE',  ( -17.26457240846633567, -7.760713630915982542, 70.50507891880883449 ) ) ;
#1811 = CARTESIAN_POINT ( 'NONE',  ( -13.24838165316469052, -8.639299380175261334, 60.61763066408384759 ) ) ;
#1812 = CARTESIAN_POINT ( 'NONE',  ( -10.40277073914389661, -15.44443991871667343, 57.56792809063193772 ) ) ;
#1813 = ADVANCED_FACE ( 'NONE', ( #42371 ), #18634, .T. ) ;
#1814 = CARTESIAN_POINT ( 'NONE',  ( -15.88442554950127139, -7.926310505211968227, 71.02478706424572863 ) ) ;
#1815 = PLANE ( 'NONE',  #25993 ) ;
#1816 = ORIENTED_EDGE ( 'NONE', *, *, #47084, .T. ) ;
#1817 = ORIENTED_EDGE ( 'NONE', *, *, #39548, .T. ) ;
#1818 = B_SPLINE_CURVE_WITH_KNOTS ( 'NONE', 1,
 ( #2349, #36311 ),
 .UNSPECIFIED., .F., .F.,
 ( 2, 2 ),
 ( 0.000000000000000000, 1.000000000000000000 ),
 .UNSPECIFIED. ) ;
#1819 = CARTESIAN_POINT ( 'NONE',  ( -20.61159385541304445, -8.990409506049200417, 49.61344411288074951 ) ) ;
#1820 = CARTESIAN_POINT ( 'NONE',  ( -21.23484681875272528, -20.74088929683185611, 69.33978048267414351 ) ) ;
#1821 = CIRCLE ( 'NONE', #18313, 1.249999999999999334 ) ;
#1822 = CARTESIAN_POINT ( 'NONE',  ( -14.09489777434381530, -8.144396602184544420, 70.92295928270578997 ) ) ;
#1823 =( BOUNDED_CURVE ( )  B_SPLINE_CURVE ( 3, ( #46798, #9378, #24397, #5690 ),
 .UNSPECIFIED., .F., .F. ) 
 B_SPLINE_CURVE_WITH_KNOTS ( ( 4, 4 ),
 ( 0.000000000000000000, 0.4074455897393636228 ),
 .UNSPECIFIED. ) 
 CURVE ( )  GEOMETRIC_REPRESENTATION_ITEM ( )  RATIONAL_B_SPLINE_CURVE ( ( 1.000000000000000000, 0.4567392136813388515, 0.3561768502900328204, 0.6983129098260818513 ) ) 
 REPRESENTATION_ITEM ( '' )  );
#1824 = CARTESIAN_POINT ( 'NONE',  ( -11.59906938467913484, -10.16455840884576389, 71.22539037155303276 ) ) ;
#1825 = DIRECTION ( 'NONE',  ( -3.071710424422018668E-17, 6.404604876783312462E-16, 1.000000000000000000 ) ) ;
#1826 = CARTESIAN_POINT ( 'NONE',  ( -24.34216731694079527, -17.57390378916213436, 66.13631411268475802 ) ) ;
#1827 = ORIENTED_EDGE ( 'NONE', *, *, #39300, .T. ) ;
#1828 = EDGE_CURVE ( 'NONE', #30777, #24975, #38778, .T. ) ;
#1829 = CARTESIAN_POINT ( 'NONE',  ( -14.33701861991839976, -19.05567172067550530, 49.52966884056656482 ) ) ;
#1830 = DIRECTION ( 'NONE',  ( 8.478320013641884810E-07, -8.009068454735622942E-06, 0.9999999999675679430 ) ) ;
#1831 = EDGE_CURVE ( 'NONE', #7816, #31055, #36783, .T. ) ;
#1832 = ORIENTED_EDGE ( 'NONE', *, *, #10446, .F. ) ;
#1833 = CARTESIAN_POINT ( 'NONE',  ( -23.89081516821958218, -17.62458393556817171, 58.88889748697027926 ) ) ;
#1834 =( BOUNDED_CURVE ( )  B_SPLINE_CURVE ( 3, ( #35321, #46422, #13630, #28670 ),
 .UNSPECIFIED., .F., .F. ) 
 B_SPLINE_CURVE_WITH_KNOTS ( ( 4, 4 ),
 ( 0.9074455897393596260, 1.000000000000000000 ),
 .UNSPECIFIED. ) 
 CURVE ( )  GEOMETRIC_REPRESENTATION_ITEM ( )  RATIONAL_B_SPLINE_CURVE ( ( 0.6983129098260900669, 0.7760317562606956487, 0.8765941196519989598, 1.000000000000000000 ) ) 
 REPRESENTATION_ITEM ( '' )  );
#1835 = CARTESIAN_POINT ( 'NONE',  ( -24.87417962317557496, -14.80849170857717567, 59.42795673386487465 ) ) ;
#1836 = VERTEX_POINT ( 'NONE', #39874 ) ;
#1837 = EDGE_CURVE ( 'NONE', #44556, #19371, #43833, .T. ) ;
#1838 = CARTESIAN_POINT ( 'NONE',  ( -20.92409385541305511, -10.10920654474410618, 79.49999999999998579 ) ) ;
#1839 = CARTESIAN_POINT ( 'NONE',  ( -12.21605502382481490, -19.48707594822949218, 58.21065790830979125 ) ) ;
#1840 = ORIENTED_EDGE ( 'NONE', *, *, #42876, .T. ) ;
#1841 = CARTESIAN_POINT ( 'NONE',  ( -17.66159697976433307, -21.85550285805611637, 58.42025434932890704 ) ) ;
#1842 = DIRECTION ( 'NONE',  ( -3.071710424422018668E-17, 6.404604876783312462E-16, 1.000000000000000000 ) ) ;
#1843 = EDGE_CURVE ( 'NONE', #40764, #24808, #28001, .T. ) ;
#1844 = CARTESIAN_POINT ( 'NONE',  ( -15.43182990062313564, -8.046249867383863830, 74.36513541778452918 ) ) ;
#1845 = CARTESIAN_POINT ( 'NONE',  ( -11.09366621811533093, -17.79679521274233167, 71.67604308249768508 ) ) ;
#1846 = VERTEX_POINT ( 'NONE', #13267 ) ;
#1847 = CYLINDRICAL_SURFACE ( 'NONE', #44106, 0.1500000000000072387 ) ;
#1848 = DIRECTION ( 'NONE',  ( 1.000000000000000000, 0.000000000000000000, 0.000000000000000000 ) ) ;
#1849 = ADVANCED_FACE ( 'NONE', ( #6148 ), #39783, .T. ) ;
#1850 = CARTESIAN_POINT ( 'NONE',  ( -12.37908165583508158, -20.29102667443158126, 68.48657438459629532 ) ) ;
#1851 = PLANE ( 'NONE',  #30540 ) ;
#1852 = CARTESIAN_POINT ( 'NONE',  ( -19.28352822169459202, -22.07505156356299381, 54.27966884056655061 ) ) ;
#1853 = CARTESIAN_POINT ( 'NONE',  ( -21.99178464560338497, -9.439038884874848989, 59.87171213140518944 ) ) ;
#1854 = AXIS2_PLACEMENT_3D ( 'NONE', #26248, #169, #29697 ) ;
#1855 = DIRECTION ( 'NONE',  ( -0.000000000000000000, -0.000000000000000000, -1.000000000000000000 ) ) ;
#1856 = ORIENTED_EDGE ( 'NONE', *, *, #41314, .F. ) ;
#1857 = CARTESIAN_POINT ( 'NONE',  ( -14.49326647312024896, -18.48150914673672673, 49.52966884056656482 ) ) ;
#1858 = DIRECTION ( 'NONE',  ( 0.09332174201254166135, 0.9956360040033429559, 0.000000000000000000 ) ) ;
#1859 = DIRECTION ( 'NONE',  ( -3.071710424422018668E-17, 6.404604876783312462E-16, 1.000000000000000000 ) ) ;
#1860 = ORIENTED_EDGE ( 'NONE', *, *, #23584, .T. ) ;
#1861 = ORIENTED_EDGE ( 'NONE', *, *, #24474, .T. ) ;
#1862 = VERTEX_POINT ( 'NONE', #9618 ) ;
#1863 = VERTEX_POINT ( 'NONE', #35927 ) ;
#1864 = CARTESIAN_POINT ( 'NONE',  ( -21.29196722032537537, -20.70380199363842877, 72.53918572867779346 ) ) ;
#1865 = CARTESIAN_POINT ( 'NONE',  ( -23.78500256881436314, -11.88707711785523635, 59.48235732566631384 ) ) ;
#1866 = EDGE_CURVE ( 'NONE', #34062, #1531, #36887, .T. ) ;
#1867 = FACE_OUTER_BOUND ( 'NONE', #22414, .T. ) ;
#1868 = CARTESIAN_POINT ( 'NONE',  ( -14.37682202087475680, -19.38786730597467667, 53.49999999999995026 ) ) ;
#1869 = CARTESIAN_POINT ( 'NONE',  ( -13.35650607536230261, -9.112225995665673040, 60.66623508672251575 ) ) ;
#1870 = ORIENTED_EDGE ( 'NONE', *, *, #11942, .T. ) ;
#1871 = ORIENTED_EDGE ( 'NONE', *, *, #38515, .F. ) ;
#1872 = CARTESIAN_POINT ( 'NONE',  ( -21.59909385650551528, -8.114302828567740988, 52.18300498402516041 ) ) ;
#1873 = CARTESIAN_POINT ( 'NONE',  ( -21.65613231742964473, -20.94137680209911423, 72.63791026777079196 ) ) ;
#1874 = CARTESIAN_POINT ( 'NONE',  ( -16.50258162057404832, -20.23145840177225452, 53.49899999999994549 ) ) ;
#1875 = CARTESIAN_POINT ( 'NONE',  ( -10.37818533259200748, -17.22973363664382873, 61.27247698181179913 ) ) ;
#1876 = CARTESIAN_POINT ( 'NONE',  ( -21.71159385650551599, -6.922745924619793101, 51.69366785382590024 ) ) ;
#1877 = EDGE_CURVE ( 'NONE', #46048, #31463, #48255, .T. ) ;
#1878 = ORIENTED_EDGE ( 'NONE', *, *, #30425, .T. ) ;
#1879 = LINE ( 'NONE', #1149, #36667 ) ;
#1880 = FACE_OUTER_BOUND ( 'NONE', #39765, .T. ) ;
#1881 = VECTOR ( 'NONE', #25166, 1000.000000000000000 ) ;
#1882 = CYLINDRICAL_SURFACE ( 'NONE', #14989, 0.1500000000000043521 ) ;
#1883 = ORIENTED_EDGE ( 'NONE', *, *, #19647, .F. ) ;
#1884 = CARTESIAN_POINT ( 'NONE',  ( -11.66088473761816324, -18.78248764865968568, 68.21689682892682072 ) ) ;
#1885 = EDGE_CURVE ( 'NONE', #48035, #16853, #9368, .T. ) ;
#1886 = CARTESIAN_POINT ( 'NONE',  ( -9.975558569371616002, -14.65758674969880104, 71.58428599250275681 ) ) ;
#1887 = CARTESIAN_POINT ( 'NONE',  ( -10.43128225812950305, -13.88506779950195202, 61.01001469056328119 ) ) ;
#1888 = CYLINDRICAL_SURFACE ( 'NONE', #42878, 2.000000000000003553 ) ;
#1889 = EDGE_CURVE ( 'NONE', #47208, #6712, #40360, .T. ) ;
#1890 = ORIENTED_EDGE ( 'NONE', *, *, #37328, .T. ) ;
#1891 = B_SPLINE_CURVE_WITH_KNOTS ( 'NONE', 3,
 ( #14049, #36693, #2988, #37691, #18738, #30091, #41892, #295, #22951, #26630 ),
 .UNSPECIFIED., .F., .F.,
 ( 4, 2, 2, 2, 4 ),
 ( 0.000000000000000000, 0.2500000000000000000, 0.5000000000000000000, 0.7500000000000000000, 1.000000000000000000 ),
 .UNSPECIFIED. ) ;
#1892 = DIRECTION ( 'NONE',  ( 1.000000000000000000, 2.866981220435666553E-17, 0.000000000000000000 ) ) ;
#1893 = EDGE_CURVE ( 'NONE', #11361, #36726, #22032, .T. ) ;
#1894 = CARTESIAN_POINT ( 'NONE',  ( -11.74434772961222961, -10.63247619797795629, 74.73325195789129793 ) ) ;
#1895 = CARTESIAN_POINT ( 'NONE',  ( -18.11396590982544197, -21.77512906430638040, 65.64532159443497505 ) ) ;
#1896 = EDGE_LOOP ( 'NONE', ( #20916, #20589 ) ) ;
#1897 = DIRECTION ( 'NONE',  ( 3.413470714839332458E-33, -1.190614954331866791E-16, 1.000000000000000000 ) ) ;
#1898 = ORIENTED_EDGE ( 'NONE', *, *, #25020, .T. ) ;
#1899 = CARTESIAN_POINT ( 'NONE',  ( -9.975583804105555785, -14.65598652642324673, 71.44287259100559595 ) ) ;
#1900 = CARTESIAN_POINT ( 'NONE',  ( -16.26649175736496744, -21.71412290693840319, 61.98398093021437916 ) ) ;
#1901 = ORIENTED_EDGE ( 'NONE', *, *, #25081, .T. ) ;
#1902 = CARTESIAN_POINT ( 'NONE',  ( -10.31364544024427410, -17.03300993871772562, 57.80265247535063367 ) ) ;
#1903 = CARTESIAN_POINT ( 'NONE',  ( -21.91034545428830782, -20.18261758176410936, 58.76442899736473180 ) ) ;
#1904 = CARTESIAN_POINT ( 'NONE',  ( -23.44980260057078070, -18.46889688393208573, 72.76368236443251192 ) ) ;
#1905 = VERTEX_POINT ( 'NONE', #43832 ) ;
#1906 = CARTESIAN_POINT ( 'NONE',  ( -9.996749499990320587, -14.22650194697012260, 64.54950375361089243 ) ) ;
#1907 = CARTESIAN_POINT ( 'NONE',  ( -20.66696855643225561, -21.06909979829504209, 58.94475164909855636 ) ) ;
#1909 = ADVANCED_FACE ( 'NONE', ( #18179 ), #38192, .T. ) ;
#1908 = CARTESIAN_POINT ( 'NONE',  ( -15.28303595616968913, -7.672713470548185200, 74.19330299898706471 ) ) ;
#1910 = ORIENTED_EDGE ( 'NONE', *, *, #27558, .F. ) ;
#1911 = CARTESIAN_POINT ( 'NONE',  ( -15.67484944857656082, -7.976566202440097619, 67.02518389757648265 ) ) ;
#1912 = EDGE_CURVE ( 'NONE', #25645, #15953, #40864, .T. ) ;
#1913 = VECTOR ( 'NONE', #46444, 1000.000000000000227 ) ;
#1914 = LINE ( 'NONE', #31953, #16475 ) ;
#1915 = EDGE_CURVE ( 'NONE', #40821, #18743, #40128, .T. ) ;
#1916 = EDGE_CURVE ( 'NONE', #45934, #39678, #17693, .T. ) ;
#1917 = VECTOR ( 'NONE', #12087, 1000.000000000000000 ) ;
#1918 = VERTEX_POINT ( 'NONE', #13985 ) ;
#1919 = VERTEX_POINT ( 'NONE', #2920 ) ;
#1920 = CARTESIAN_POINT ( 'NONE',  ( -14.88579407610268035, -21.33278181836255882, 58.27504001164205505 ) ) ;
#1921 = PLANE ( 'NONE',  #3674 ) ;
#1922 = CARTESIAN_POINT ( 'NONE',  ( -24.87384330133638599, -14.87999890626018384, 59.35804801245023299 ) ) ;
#1923 = CARTESIAN_POINT ( 'NONE',  ( -18.13659385650551670, -6.915538690918074494, 49.31353937987644542 ) ) ;
#1924 = DIRECTION ( 'NONE',  ( -7.357566627711770083E-06, -1.068273751865974396E-05, 0.9999999999158726283 ) ) ;
#1925 = CARTESIAN_POINT ( 'NONE',  ( -19.78726556874234888, -21.93198837902608744, 53.76173960638111993 ) ) ;
#1926 = CARTESIAN_POINT ( 'NONE',  ( -13.14998806103231566, -9.265559761403904915, 67.67942786032521951 ) ) ;
#1927 = CARTESIAN_POINT ( 'NONE',  ( -10.79572441526863180, -11.40795732096215254, 67.80359905390240272 ) ) ;
#1928 = ORIENTED_EDGE ( 'NONE', *, *, #8269, .F. ) ;
#1929 = ORIENTED_EDGE ( 'NONE', *, *, #16604, .T. ) ;
#1930 = CARTESIAN_POINT ( 'NONE',  ( -10.61641629527463770, -11.78277212779517136, 74.74335553404092991 ) ) ;
#1931 = CARTESIAN_POINT ( 'NONE',  ( -21.94216005978649875, -20.15605564530504878, 59.06442870682581514 ) ) ;
#1932 = CARTESIAN_POINT ( 'NONE',  ( -20.60942684424193416, -21.09890871138989965, 58.65947248567252359 ) ) ;
#1933 = CARTESIAN_POINT ( 'NONE',  ( -22.37742512587845312, -19.75764156297556795, 72.75473533163390982 ) ) ;
#1934 = PLANE ( 'NONE',  #7963 ) ;
#1935 = ORIENTED_EDGE ( 'NONE', *, *, #21287, .T. ) ;
#1936 = B_SPLINE_CURVE_WITH_KNOTS ( 'NONE', 3,
 ( #23055, #45715, #19843, #34843, #42002, #16110, #12437, #8275, #23291, #882 ),
 .UNSPECIFIED., .F., .F.,
 ( 4, 2, 2, 2, 4 ),
 ( 0.6272669072877771201, 0.7522669073072866253, 0.8772669073267960194, 1.002266907346305524, 1.127266907365815030 ),
 .UNSPECIFIED. ) ;
#1937 = EDGE_CURVE ( 'NONE', #47219, #16341, #7128, .T. ) ;
#1938 = CARTESIAN_POINT ( 'NONE',  ( -14.96634385547669055, -21.36368446393953846, 61.63600446054231696 ) ) ;
#1939 = PRESENTATION_STYLE_ASSIGNMENT (( #10308 ) ) ;
#1940 = CYLINDRICAL_SURFACE ( 'NONE', #27644, 1.249999999999998668 ) ;
#1941 = CARTESIAN_POINT ( 'NONE',  ( -24.07704370891653767, -17.14264987453632827, 72.89808101046212130 ) ) ;
#1942 = VERTEX_POINT ( 'NONE', #33426 ) ;
#1943 = CARTESIAN_POINT ( 'NONE',  ( -11.86838291625971742, -9.845553222893467904, 64.14418898700822069 ) ) ;
#1944 = VECTOR ( 'NONE', #14922, 1000.000000000000000 ) ;
#1945 = CARTESIAN_POINT ( 'NONE',  ( -43.28566308618228931, -14.90920654474410512, 56.10744615384614065 ) ) ;
#1946 = CARTESIAN_POINT ( 'NONE',  ( 10.57590614458695377, 1.890747609047609190, 50.53028072113853142 ) ) ;
#1947 = AXIS2_PLACEMENT_3D ( 'NONE', #16013, #22706, #31057 ) ;
#1948 = CARTESIAN_POINT ( 'NONE',  ( -18.65633333895540602, -7.917218528759340401, 73.91234765977904431 ) ) ;
#1949 = CARTESIAN_POINT ( 'NONE',  ( -16.77572482835368817, -7.785357162821431309, 73.96018178516708019 ) ) ;
#1950 =( BOUNDED_SURFACE ( )  B_SPLINE_SURFACE ( 1, 2, ( 
 ( #27373, #35892, #12115, #19260, #8675, #8915, #4480, #19990, #42406, #34262, #549, #38696, #8193, #42159, #8422, #23448, #38443, #46339, #4733, #23704, #13491, #42655, #4980, #34995, #2174, #28536, #1261, #39605, #24607, #17177, #32229, #47244, #43560, #14675, #14199, #40099, #28766, #7096, #36612, #3146, #44054, #17436, #2893, #32924, #21858, #6114, #29741, #10305, #36379, #24838, #25550, #39847, #2662, #21143, #32467, #36140, #33163, #2425, #13722, #48439, #48201, #47491, #29255, #40812, #44776, #43801, #25797, #10056, #25078, #10777, #6361, #21394, #17668, #44290, #32693, #47718, #22114, #17899, #18150, #25322, #13957, #47965, #10543, #36854, #29005, #40333, #6605, #21626, #37104, #40563, #14431, #6842, #29491, #3384, #44521, #18395, #33400, #26532, #33647, #29990, #4142, #26784, #34386, #45263, #27017, #7348, #33913, #19140, #11507, #11760, #12003, #18902, #45502, #22855, #34147, #4364, #3892, #45024, #19380, #11275, #26048, #23323, #41803, #37850, #38319, #4607, #8085, #673, #19627, #34638, #30962, #41552, #41067, #919, #22594, #7836, #37589, #22346, #23093, #444, #206, #3631, #37345, #14933, #18635, #15419, #8311, #15181, #11028, #38085, #48691, #30244, #15674, #30488, #30728, #45754, #42039, #15917, #26287, #41300, #7589, #24057, #24549, #1145, #24301, #42533, #9274, #39306, #46468, #27499, #39053, #31429, #28224, #38572, #42283, #4862, #19878, #31919, #34876 ),
 ( #43257, #9040, #5590, #16400, #16151, #5340, #20355, #42999, #27256, #35835, #12720, #8803, #9526, #23821, #20603, #35116, #31193, #39544, #27737, #35601, #42769, #35364, #46216, #12471, #1635, #12948, #1876, #16647, #13177, #8548, #20108, #31679, #46703, #27974, #46934, #5100, #16878, #5825, #20837, #2117, #38821, #1383, #17115, #45979, #12236, #23575, #17837, #43990, #10714, #25730, #29193, #40504, #44460, #40749, #3326, #17604, #13428, #7029, #43741, #28943, #9991, #43500, #32865, #10247, #40038, #24783, #9763, #36077, #39784, #25261, #29429, #21331, #44233, #47902, #25488, #47430, #32167, #22048, #33097, #36320, #2360, #2832, #37041, #47182, #21569, #40279, #14135, #10486, #25017, #48143, #13660, #6545, #14372, #6302, #28477, #6782, #3078, #32410, #21793, #36548, #6050, #21081, #36788, #17370, #2605, #28704, #32638, #47659, #18083, #13900, #25984, #4311, #19078, #10964, #30181, #45439, #19319, #48376, #11693, #22286, #33336, #48628, #7774, #375, #44961, #15359, #45199, #7527, #11443, #41239, #33581, #22791, #34323, #26469, #18835, #8025, #41005, #37784, #18571, #4080, #34086, #22529, #3567, #33843, #37523, #26718, #44709, #14609, #7284, #37279, #41481, #3824, #14864, #11216, #29926, #142, #26225, #30423, #15122, #41736, #23037, #18329, #38022, #29673, #25899, #21960, #25647, #18003, #10877, #21717, #21490, #40912, #39952, #33499, #2754, #44383, #33019, #47589, #7203 ) ),
 .UNSPECIFIED., .F., .F., .F. ) 
 B_SPLINE_SURFACE_WITH_KNOTS ( ( 2, 2 ),
 ( 3, 2, 2, 2, 2, 2, 2, 2, 2, 2, 2, 2, 2, 2, 2, 2, 2, 2, 2, 2, 2, 2, 2, 2, 2, 2, 2, 2, 2, 2, 2, 2, 2, 2, 2, 2, 2, 2, 2, 2, 2, 2, 2, 2, 2, 2, 2, 2, 2, 2, 2, 2, 2, 2, 2, 2, 2, 2, 2, 2, 2, 2, 2, 2, 2, 2, 2, 2, 2, 2, 2, 2, 2, 2, 2, 2, 2, 2, 2, 2, 2, 2, 2, 2, 2, 2, 2, 2, 2, 3 ),
 ( 0.000000000000000000, 1.000000000000000000 ),
 ( 0.000000000000000000, 0.01041666666666666609, 0.02083333333333333218, 0.03125000000000000000, 0.04166666666666666435, 0.05208333333333333565, 0.06250000000000000000, 0.07291666666666667129, 0.08333333333333332871, 0.09375000000000000000, 0.1041666666666666713, 0.1145833333333333287, 0.1250000000000000000, 0.1354166666666666574, 0.1458333333333333426, 0.1562500000000000000, 0.1666666666666666574, 0.1770833333333333426, 0.1875000000000000000, 0.1979166666666666574, 0.2083333333333333426, 0.2187500000000000000, 0.2291666666666666574, 0.2395833333333333426, 0.2500000000000000000, 0.2604166666666666852, 0.2708333333333333148, 0.2812500000000000000, 0.2916666666666666852, 0.3020833333333333148, 0.3125000000000000000, 0.3229166666666666852, 0.3333333333333333148, 0.3437500000000000000, 0.3541666666666666852, 0.3645833333333333148, 0.3750000000000000000, 0.3854166666666666852, 0.3958333333333333148, 0.4062500000000000000, 0.4166666666666666852, 0.4270833333333333148, 0.4375000000000000000, 0.4479166666666666852, 0.4583333333333333148, 0.4687500000000000000, 0.4791666666666666852, 0.4895833333333333148, 0.5000000000000000000, 0.5104166666666666297, 0.5208333333333333703, 0.5312500000000000000, 0.5416666666666666297, 0.5520833333333333703, 0.5625000000000000000, 0.5729166666666666297, 0.5833333333333333703, 0.5937500000000000000, 0.6041666666666666297, 0.6145833333333333703, 0.6250000000000000000, 0.6354166666666666297, 0.6458333333333333703, 0.6562500000000000000, 0.6666666666666666297, 0.6770833333333333703, 0.6875000000000000000, 0.6979166666666666297, 0.7083333333333333703, 0.7187500000000000000, 0.7291666666666666297, 0.7395833333333333703, 0.7500000000000000000, 0.7604166666666666297, 0.7708333333333333703, 0.7812500000000000000, 0.7916666666666666297, 0.8020833333333333703, 0.8125000000000000000, 0.8229166666666666297, 0.8333333333333333703, 0.8437500000000000000, 0.8541666666666666297, 0.8645833333333333703, 0.8750000000000000000, 0.8854166666666666297, 0.8958333333333333703, 0.9062500000000000000, 0.9166666666666666297, 0.9259051122687710356 ),
 .UNSPECIFIED. ) 
 GEOMETRIC_REPRESENTATION_ITEM ( )  RATIONAL_B_SPLINE_SURFACE ( (
 ( 1.000000000000000000, 0.9238795325112867385, 1.000000000000000000, 0.9238795325112867385, 1.000000000000000000, 0.9238795325112867385, 1.000000000000000000, 0.9238795325112867385, 1.000000000000000000, 0.9238795325112867385, 1.000000000000000000, 0.9238795325112867385, 1.000000000000000000, 0.9238795325112867385, 1.000000000000000000, 0.9238795325112867385, 1.000000000000000000, 0.9238795325112867385, 1.000000000000000000, 0.9238795325112867385, 1.000000000000000000, 0.9238795325112867385, 1.000000000000000000, 0.9238795325112867385, 1.000000000000000000, 0.9238795325112867385, 1.000000000000000000, 0.9238795325112867385, 1.000000000000000000, 0.9238795325112867385, 1.000000000000000000, 0.9238795325112867385, 1.000000000000000000, 0.9238795325112867385, 1.000000000000000000, 0.9238795325112867385, 1.000000000000000000, 0.9238795325112867385, 1.000000000000000000, 0.9238795325112867385, 1.000000000000000000, 0.9238795325112867385, 1.000000000000000000, 0.9238795325112867385, 1.000000000000000000, 0.9238795325112867385, 1.000000000000000000, 0.9238795325112867385, 1.000000000000000000, 0.9238795325112867385, 1.000000000000000000, 0.9238795325112867385, 1.000000000000000000, 0.9238795325112867385, 1.000000000000000000, 0.9238795325112867385, 1.000000000000000000, 0.9238795325112867385, 1.000000000000000000, 0.9238795325112867385, 1.000000000000000000, 0.9238795325112867385, 1.000000000000000000, 0.9238795325112867385, 1.000000000000000000, 0.9238795325112867385, 1.000000000000000000, 0.9238795325112867385, 1.000000000000000000, 0.9238795325112867385, 1.000000000000000000, 0.9238795325112867385, 1.000000000000000000, 0.9238795325112867385, 1.000000000000000000, 0.9238795325112867385, 1.000000000000000000, 0.9238795325112867385, 1.000000000000000000, 0.9238795325112867385, 1.000000000000000000, 0.9238795325112867385, 1.000000000000000000, 0.9238795325112867385, 1.000000000000000000, 0.9238795325112867385, 1.000000000000000000, 0.9238795325112867385, 1.000000000000000000, 0.9238795325112867385, 1.000000000000000000, 0.9238795325112867385, 1.000000000000000000, 0.9238795325112867385, 1.000000000000000000, 0.9238795325112867385, 1.000000000000000000, 0.9238795325112867385, 1.000000000000000000, 0.9238795325112867385, 1.000000000000000000, 0.9238795325112867385, 1.000000000000000000, 0.9238795325112867385, 1.000000000000000000, 0.9238795325112867385, 1.000000000000000000, 0.9238795325112867385, 1.000000000000000000, 0.9238795325112867385, 1.000000000000000000, 0.9238795325112867385, 1.000000000000000000, 0.9238795325112867385, 1.000000000000000000, 0.9238795325112867385, 1.000000000000000000, 0.9238795325112867385, 1.000000000000000000, 0.9238795325112867385, 1.000000000000000000, 0.9238795325112867385, 1.000000000000000000, 0.9238795325112867385, 1.000000000000000000, 0.9238795325112867385, 1.000000000000000000, 0.9238795325112867385, 1.000000000000000000, 0.9238795325112867385, 1.000000000000000000, 0.9238795325112867385, 1.000000000000000000, 0.9238795325112867385, 1.000000000000000000, 0.9238795325112867385, 1.000000000000000000, 0.9238795325112867385, 1.000000000000000000, 0.9238795325112867385, 1.000000000000000000, 0.9238795325112867385, 1.000000000000000000, 0.9238795325112867385, 1.000000000000000000, 0.9238795325112867385, 1.000000000000000000, 0.9238795325112867385, 1.000000000000000000, 0.9238795325112867385, 1.000000000000000000, 0.9238795325112867385, 1.000000000000000000, 0.9238795325112867385, 1.000000000000000000, 0.9238795325112867385, 1.000000000000000000, 0.9238795325112867385, 1.000000000000000000, 0.9238795325112867385, 1.000000000000000000, 0.9238795325112867385, 1.000000000000000000, 0.9238795325112867385, 1.000000000000000000, 0.9238795325112867385, 1.000000000000000000, 0.9238795325112867385, 1.000000000000000000, 0.9238795325112867385, 1.000000000000000000, 0.9238795325112867385, 1.000000000000000000, 0.9238795325112867385, 1.000000000000000000, 0.9238795325112867385, 1.000000000000000000, 0.9324894593822820044, 0.9847278705211290895),
 ( 1.000000000000000000, 0.9238795325112867385, 1.000000000000000000, 0.9238795325112867385, 1.000000000000000000, 0.9238795325112867385, 1.000000000000000000, 0.9238795325112867385, 1.000000000000000000, 0.9238795325112867385, 1.000000000000000000, 0.9238795325112867385, 1.000000000000000000, 0.9238795325112867385, 1.000000000000000000, 0.9238795325112867385, 1.000000000000000000, 0.9238795325112867385, 1.000000000000000000, 0.9238795325112867385, 1.000000000000000000, 0.9238795325112867385, 1.000000000000000000, 0.9238795325112867385, 1.000000000000000000, 0.9238795325112867385, 1.000000000000000000, 0.9238795325112867385, 1.000000000000000000, 0.9238795325112867385, 1.000000000000000000, 0.9238795325112867385, 1.000000000000000000, 0.9238795325112867385, 1.000000000000000000, 0.9238795325112867385, 1.000000000000000000, 0.9238795325112867385, 1.000000000000000000, 0.9238795325112867385, 1.000000000000000000, 0.9238795325112867385, 1.000000000000000000, 0.9238795325112867385, 1.000000000000000000, 0.9238795325112867385, 1.000000000000000000, 0.9238795325112867385, 1.000000000000000000, 0.9238795325112867385, 1.000000000000000000, 0.9238795325112867385, 1.000000000000000000, 0.9238795325112867385, 1.000000000000000000, 0.9238795325112867385, 1.000000000000000000, 0.9238795325112867385, 1.000000000000000000, 0.9238795325112867385, 1.000000000000000000, 0.9238795325112867385, 1.000000000000000000, 0.9238795325112867385, 1.000000000000000000, 0.9238795325112867385, 1.000000000000000000, 0.9238795325112867385, 1.000000000000000000, 0.9238795325112867385, 1.000000000000000000, 0.9238795325112867385, 1.000000000000000000, 0.9238795325112867385, 1.000000000000000000, 0.9238795325112867385, 1.000000000000000000, 0.9238795325112867385, 1.000000000000000000, 0.9238795325112867385, 1.000000000000000000, 0.9238795325112867385, 1.000000000000000000, 0.9238795325112867385, 1.000000000000000000, 0.9238795325112867385, 1.000000000000000000, 0.9238795325112867385, 1.000000000000000000, 0.9238795325112867385, 1.000000000000000000, 0.9238795325112867385, 1.000000000000000000, 0.9238795325112867385, 1.000000000000000000, 0.9238795325112867385, 1.000000000000000000, 0.9238795325112867385, 1.000000000000000000, 0.9238795325112867385, 1.000000000000000000, 0.9238795325112867385, 1.000000000000000000, 0.9238795325112867385, 1.000000000000000000, 0.9238795325112867385, 1.000000000000000000, 0.9238795325112867385, 1.000000000000000000, 0.9238795325112867385, 1.000000000000000000, 0.9238795325112867385, 1.000000000000000000, 0.9238795325112867385, 1.000000000000000000, 0.9238795325112867385, 1.000000000000000000, 0.9238795325112867385, 1.000000000000000000, 0.9238795325112867385, 1.000000000000000000, 0.9238795325112867385, 1.000000000000000000, 0.9238795325112867385, 1.000000000000000000, 0.9238795325112867385, 1.000000000000000000, 0.9238795325112867385, 1.000000000000000000, 0.9238795325112867385, 1.000000000000000000, 0.9238795325112867385, 1.000000000000000000, 0.9238795325112867385, 1.000000000000000000, 0.9238795325112867385, 1.000000000000000000, 0.9238795325112867385, 1.000000000000000000, 0.9238795325112867385, 1.000000000000000000, 0.9238795325112867385, 1.000000000000000000, 0.9238795325112867385, 1.000000000000000000, 0.9238795325112867385, 1.000000000000000000, 0.9238795325112867385, 1.000000000000000000, 0.9238795325112867385, 1.000000000000000000, 0.9238795325112867385, 1.000000000000000000, 0.9238795325112867385, 1.000000000000000000, 0.9238795325112867385, 1.000000000000000000, 0.9238795325112867385, 1.000000000000000000, 0.9238795325112867385, 1.000000000000000000, 0.9238795325112867385, 1.000000000000000000, 0.9238795325112867385, 1.000000000000000000, 0.9238795325112867385, 1.000000000000000000, 0.9238795325112867385, 1.000000000000000000, 0.9238795325112867385, 1.000000000000000000, 0.9238795325112867385, 1.000000000000000000, 0.9238795325112867385, 1.000000000000000000, 0.9238795325112867385, 1.000000000000000000, 0.9324894593822820044, 0.9847278705211290895) ) ) 
 REPRESENTATION_ITEM ( '' )  SURFACE ( )  );
#1951 = CARTESIAN_POINT ( 'NONE',  ( -23.45015259912689132, -11.24725851716134883, 70.11884051640547000 ) ) ;
#1952 = ORIENTED_EDGE ( 'NONE', *, *, #21868, .F. ) ;
#1953 = CARTESIAN_POINT ( 'NONE',  ( -10.49991623338872415, -13.77081093687474578, 57.63752186588624937 ) ) ;
#1954 = ORIENTED_EDGE ( 'NONE', *, *, #19326, .T. ) ;
#1955 = CARTESIAN_POINT ( 'NONE',  ( -19.24190894175819366, -7.584296403803404196, 63.54593838833191910 ) ) ;
#1956 = FACE_OUTER_BOUND ( 'NONE', #11602, .T. ) ;
#1957 = ORIENTED_EDGE ( 'NONE', *, *, #43597, .T. ) ;
#1958 = FACE_OUTER_BOUND ( 'NONE', #4292, .T. ) ;
#1959 = CARTESIAN_POINT ( 'NONE',  ( -13.94909385650551492, -8.104110260919579645, 48.81699501597546487 ) ) ;
#1960 = ORIENTED_EDGE ( 'NONE', *, *, #10650, .F. ) ;
#1961 = CARTESIAN_POINT ( 'NONE',  ( -17.93803624496681692, -7.826487624369620200, 60.26987800131050932 ) ) ;
#1962 = CARTESIAN_POINT ( 'NONE',  ( -19.04853579327176760, -7.948602568230340282, 63.71617106789811658 ) ) ;
#1963 = CARTESIAN_POINT ( 'NONE',  ( -17.42409385541299471, -14.80920654474435594, 52.02966884056656482 ) ) ;
#1964 = ORIENTED_EDGE ( 'NONE', *, *, #31188, .T. ) ;
#1966 = LINE ( 'NONE', #9125, #9036 ) ;
#1965 =( BOUNDED_CURVE ( )  B_SPLINE_CURVE ( 3, ( #15785, #42398, #24411, #35471 ),
 .UNSPECIFIED., .F., .F. ) 
 B_SPLINE_CURVE_WITH_KNOTS ( ( 4, 4 ),
 ( 0.5000000000000000000, 0.9074455897393689519 ),
 .UNSPECIFIED. ) 
 CURVE ( )  GEOMETRIC_REPRESENTATION_ITEM ( )  RATIONAL_B_SPLINE_CURVE ( ( 0.9999999999999952260, 0.4567392136813272496, 0.3561768502900317102, 0.6983129098261036116 ) ) 
 REPRESENTATION_ITEM ( '' )  );
#1967 = PLANE ( 'NONE',  #12522 ) ;
#1968 = CARTESIAN_POINT ( 'NONE',  ( -20.88147576600584543, -8.209942340109883219, 60.02620652709861560 ) ) ;
#1969 = CARTESIAN_POINT ( 'NONE',  ( -23.38313847423633263, -10.33780256150599541, 59.85849373767491954 ) ) ;
#1970 = EDGE_CURVE ( 'NONE', #1420, #21415, #44084, .T. ) ;
#1971 = ADVANCED_FACE ( 'NONE', ( #17463 ), #13751, .T. ) ;
#1972 = ORIENTED_EDGE ( 'NONE', *, *, #4173, .T. ) ;
#1973 = ORIENTED_EDGE ( 'NONE', *, *, #7462, .F. ) ;
#1974 = CARTESIAN_POINT ( 'NONE',  ( -10.40127070788197017, -12.32249518151173895, 57.51352764219546998 ) ) ;
#1975 = CARTESIAN_POINT ( 'NONE',  ( -12.76954176995949197, -15.35549139150514186, 49.52966884056655772 ) ) ;
#1976 = VERTEX_POINT ( 'NONE', #48225 ) ;
#1977 = CARTESIAN_POINT ( 'NONE',  ( -22.08699904183838214, -20.10091237387970153, 66.11910372887342646 ) ) ;
#1978 = CARTESIAN_POINT ( 'NONE',  ( -19.37709988573221054, -21.53135720868301561, 62.29503678468425676 ) ) ;
#1979 = CARTESIAN_POINT ( 'NONE',  ( -20.36159385759798823, -7.228003583438117552, 51.38655588711986155 ) ) ;
#1980 = CARTESIAN_POINT ( 'NONE',  ( -20.04849592361258104, -21.35284569240296548, 72.69006679631317525 ) ) ;
#1981 = LINE ( 'NONE', #24159, #47153 ) ;
#1982 = CARTESIAN_POINT ( 'NONE',  ( -12.21269597510284832, -10.13573543075226624, 60.66804197197834014 ) ) ;
#1983 =( BOUNDED_CURVE ( )  B_SPLINE_CURVE ( 3, ( #30625, #34043, #23472, #30136 ),
 .UNSPECIFIED., .F., .F. ) 
 B_SPLINE_CURVE_WITH_KNOTS ( ( 4, 4 ),
 ( 4.712388980384689674, 4.921828490624008623 ),
 .UNSPECIFIED. ) 
 CURVE ( )  GEOMETRIC_REPRESENTATION_ITEM ( )  RATIONAL_B_SPLINE_CURVE ( ( 1.000000000000000000, 0.9963479302455156006, 0.9963479302455156006, 1.000000000000000000 ) ) 
 REPRESENTATION_ITEM ( '' )  );
#1984 = VECTOR ( 'NONE', #8791, 1000.000000000000000 ) ;
#1985 = EDGE_LOOP ( 'NONE', ( #44529, #25437, #11830, #4342 ) ) ;
#1986 = EDGE_CURVE ( 'NONE', #15214, #38842, #45039, .T. ) ;
#1987 = EDGE_CURVE ( 'NONE', #38799, #28542, #25823, .T. ) ;
#1988 = CARTESIAN_POINT ( 'NONE',  ( -16.25451963475149952, -21.76959929332391397, 65.36997467570328979 ) ) ;
#1989 = CIRCLE ( 'NONE', #28737, 5.249999999999998224 ) ;
#1990 = CARTESIAN_POINT ( 'NONE',  ( -13.03244235208782698, -8.791229364947284353, 64.00922890431560575 ) ) ;
#1991 = CARTESIAN_POINT ( 'NONE',  ( 10.57590614458695377, 1.637040139411225059, 51.75426295951076838 ) ) ;
#1992 = FACE_OUTER_BOUND ( 'NONE', #28263, .T. ) ;
#1993 = DIRECTION ( 'NONE',  ( -3.071710424422018668E-17, 6.404604876783312462E-16, 1.000000000000000000 ) ) ;
#1994 = ORIENTED_EDGE ( 'NONE', *, *, #10445, .T. ) ;
#1995 = VERTEX_POINT ( 'NONE', #22379 ) ;
#1996 = ORIENTED_EDGE ( 'NONE', *, *, #29658, .T. ) ;
#1997 = EDGE_CURVE ( 'NONE', #16426, #3920, #37880, .T. ) ;
#1998 = CYLINDRICAL_SURFACE ( 'NONE', #35118, 0.1500000000000061007 ) ;
#1999 = CARTESIAN_POINT ( 'NONE',  ( -22.53865852806102765, -10.02986705568149439, 70.23851888881135608 ) ) ;
#2000 = CARTESIAN_POINT ( 'NONE',  ( -21.77718901952371766, -9.327210708589092292, 63.19153729619897319 ) ) ;
#2001 = ORIENTED_EDGE ( 'NONE', *, *, #34563, .T. ) ;
#2002 = CARTESIAN_POINT ( 'NONE',  ( -10.52215087187021325, -13.37195826583270630, 74.67817647370829093 ) ) ;
#2003 = FACE_OUTER_BOUND ( 'NONE', #7911, .T. ) ;
#2004 = ORIENTED_EDGE ( 'NONE', *, *, #32512, .T. ) ;
#2005 = CARTESIAN_POINT ( 'NONE',  ( -14.17008229276201625, -21.58685878473828268, 54.02312124697527906 ) ) ;
#2006 = CARTESIAN_POINT ( 'NONE',  ( -12.23849770038826534, -15.62901903366650025, 52.02966884056656482 ) ) ;
#2007 = ORIENTED_EDGE ( 'NONE', *, *, #19882, .T. ) ;
#2008 = CARTESIAN_POINT ( 'NONE',  ( -16.84865286310842336, -21.83598151670433296, 68.98088545748413480 ) ) ;
#2009 = ORIENTED_EDGE ( 'NONE', *, *, #14134, .T. ) ;
#2010 = CARTESIAN_POINT ( 'NONE',  ( -10.82867520472564848, -11.34449427682889677, 67.73369198428547122 ) ) ;
#2011 = AXIS2_PLACEMENT_3D ( 'NONE', #15786, #26648, #7705 ) ;
#2012 = ORIENTED_EDGE ( 'NONE', *, *, #20395, .T. ) ;
#2013 = PLANE ( 'NONE',  #8729 ) ;
#2014 = CARTESIAN_POINT ( 'NONE',  ( -18.56159385759799108, -7.228003583438117552, 51.38655588711986155 ) ) ;
#2015 = FACE_BOUND ( 'NONE', #10500, .T. ) ;
#2016 = ORIENTED_EDGE ( 'NONE', *, *, #28654, .F. ) ;
#2017 = FACE_OUTER_BOUND ( 'NONE', #3231, .T. ) ;
#2018 = CARTESIAN_POINT ( 'NONE',  ( -14.61186971177858496, -7.910316301228372815, 60.51270451696741048 ) ) ;
#2019 = CARTESIAN_POINT ( 'NONE',  ( -22.87594641915088900, -21.30847235828355579, 54.49999999999995026 ) ) ;
#2020 = PLANE ( 'NONE',  #18780 ) ;
#2021 = CARTESIAN_POINT ( 'NONE',  ( -18.60622205832422082, -22.16490843864383109, 72.47006330605313451 ) ) ;
#2022 = B_SPLINE_CURVE_WITH_KNOTS ( 'NONE', 1,
 ( #3617, #8296 ),
 .UNSPECIFIED., .F., .F.,
 ( 2, 2 ),
 ( 0.000000000000000000, 1.000000000000000000 ),
 .UNSPECIFIED. ) ;
#2023 = LINE ( 'NONE', #47089, #10124 ) ;
#2024 = ORIENTED_EDGE ( 'NONE', *, *, #5945, .T. ) ;
#2025 = CARTESIAN_POINT ( 'NONE',  ( 18.07590614458695200, 0.7915096701590282890, 50.27695098796855433 ) ) ;
#2026 = CARTESIAN_POINT ( 'NONE',  ( -24.65205681464681930, -13.00370337554185340, 63.02538306434979631 ) ) ;
#2027 = CARTESIAN_POINT ( 'NONE',  ( -24.86649340934961927, -14.46998543962672734, 66.30575816177258730 ) ) ;
#2028 = CARTESIAN_POINT ( 'NONE',  ( -15.14827875528926349, -21.90310222313125266, 68.67618668865188170 ) ) ;
#2029 = B_SPLINE_CURVE_WITH_KNOTS ( 'NONE', 1,
 ( #43508, #13438 ),
 .UNSPECIFIED., .F., .F.,
 ( 2, 2 ),
 ( 0.000000000000000000, 1.000000000000000000 ),
 .UNSPECIFIED. ) ;
#2030 = CARTESIAN_POINT ( 'NONE',  ( -15.92022003474064995, -7.921321712309766561, 67.14567102837528978 ) ) ;
#2031 = CARTESIAN_POINT ( 'NONE',  ( -16.84284385650551741, -8.811426318492348031, 52.18089403414752070 ) ) ;
#2032 = EDGE_CURVE ( 'NONE', #25220, #35234, #33938, .T. ) ;
#2033 = ORIENTED_EDGE ( 'NONE', *, *, #9350, .T. ) ;
#2034 = CARTESIAN_POINT ( 'NONE',  ( -22.66067231502460544, -10.16396745975044169, 66.73285430075826241 ) ) ;
#2035 = EDGE_LOOP ( 'NONE', ( #12037, #14708, #12029, #7360, #35912 ) ) ;
#2036 = CARTESIAN_POINT ( 'NONE',  ( -22.60922486080212934, -15.63195587288279675, 49.52966884056655772 ) ) ;
#2037 = CARTESIAN_POINT ( 'NONE',  ( -21.99019323879806365, -13.75373571565882713, 49.52966884056655772 ) ) ;
#2038 = CARTESIAN_POINT ( 'NONE',  ( -22.66414149941106260, -10.08832384041532926, 66.42693508874704378 ) ) ;
#2039 = CYLINDRICAL_SURFACE ( 'NONE', #8558, 0.1499999999999953315 ) ;
#2040 = CARTESIAN_POINT ( 'NONE',  ( -16.98134802626198336, -22.24608854931921087, 72.27204916158488857 ) ) ;
#2041 = ORIENTED_EDGE ( 'NONE', *, *, #10651, .T. ) ;
#2042 = CARTESIAN_POINT ( 'NONE',  ( -36.42409385541304800, -6.859212275519750435, 50.50378509014258555 ) ) ;
#2043 = CARTESIAN_POINT ( 'NONE',  ( -20.84119928492008000, -20.97572016636869918, 62.41471400470057773 ) ) ;
#2044 = EDGE_CURVE ( 'NONE', #8287, #11201, #709, .T. ) ;
#2045 = CARTESIAN_POINT ( 'NONE',  ( -20.63243265594276110, -8.084608023805090582, 63.42466202532494890 ) ) ;
#2046 = ORIENTED_EDGE ( 'NONE', *, *, #2590, .T. ) ;
#2047 = CARTESIAN_POINT ( 'NONE',  ( -9.981160085348813382, -14.48480431966832782, 68.00800125641796967 ) ) ;
#2048 = CARTESIAN_POINT ( 'NONE',  ( -10.17575246482357088, -13.08756589590406172, 71.35828583495015209 ) ) ;
#2049 = EDGE_CURVE ( 'NONE', #35577, #24336, #13021, .T. ) ;
#2050 = ADVANCED_FACE ( 'NONE', ( #8109 ), #27287, .T. ) ;
#2051 = CARTESIAN_POINT ( 'NONE',  ( -13.18362795047878144, -8.683667697493742565, 60.62445659250467145 ) ) ;
#2052 = CARTESIAN_POINT ( 'NONE',  ( -20.81921389985186721, -21.44071754855728784, 58.75979745677555854 ) ) ;
#2053 = CARTESIAN_POINT ( 'NONE',  ( -18.47956468449850931, -19.37530592812942842, 49.52966884056656482 ) ) ;
#2054 = CARTESIAN_POINT ( 'NONE',  ( -10.75774575360340002, -12.66857492743335634, 64.37909207168219439 ) ) ;
#2055 = ORIENTED_EDGE ( 'NONE', *, *, #28089, .F. ) ;
#2056 = ORIENTED_EDGE ( 'NONE', *, *, #23925, .F. ) ;
#2057 = CIRCLE ( 'NONE', #38202, 2.000000000000008882 ) ;
#2058 = CARTESIAN_POINT ( 'NONE',  ( -17.46159385541304232, -7.228003583438117552, 51.38655588711986155 ) ) ;
#2059 = EDGE_CURVE ( 'NONE', #4075, #6465, #16471, .T. ) ;
#2060 = CARTESIAN_POINT ( 'NONE',  ( -21.20019206555516078, -20.76270557045113208, 69.35450156465000759 ) ) ;
#2061 = CARTESIAN_POINT ( 'NONE',  ( -15.43182990062313742, -8.046249867383863830, 74.36513541778452918 ) ) ;
#2062 = B_SPLINE_CURVE_WITH_KNOTS ( 'NONE', 3,
 ( #46138, #45673, #26944, #4063, #42454, #841, #30653, #41964, #5027, #12163 ),
 .UNSPECIFIED., .F., .F.,
 ( 4, 2, 2, 2, 4 ),
 ( 0.000000000000000000, 0.2500000000000000000, 0.5000000000000000000, 0.7500000000000000000, 1.000000000000000000 ),
 .UNSPECIFIED. ) ;
#2063 = B_SPLINE_CURVE_WITH_KNOTS ( 'NONE', 3,
 ( #40094, #19752, #10053, #30843, #31973, #23443, #47488, #6358, #15788, #25074 ),
 .UNSPECIFIED., .F., .F.,
 ( 4, 2, 2, 2, 4 ),
 ( 0.000000000000000000, 0.2500000000000000000, 0.5000000000000000000, 0.7500000000000000000, 1.000000000000000000 ),
 .UNSPECIFIED. ) ;
#2064 = DIRECTION ( 'NONE',  ( 0.9687793358424819923, -0.2479245821708676023, 0.000000000000000000 ) ) ;
#2065 = CARTESIAN_POINT ( 'NONE',  ( -24.32145319184211729, -17.62517394100480672, 66.13695529097154235 ) ) ;
#2066 = VERTEX_POINT ( 'NONE', #4169 ) ;
#2067 = CARTESIAN_POINT ( 'NONE',  ( -16.02724774380223849, -7.491242405164911133, 63.78515641179975404 ) ) ;
#2068 = VERTEX_POINT ( 'NONE', #19665 ) ;
#2069 = CARTESIAN_POINT ( 'NONE',  ( -24.42256168760463808, -14.59956870196896794, 66.37219723247810066 ) ) ;
#2070 = CARTESIAN_POINT ( 'NONE',  ( -17.08524437268610896, -7.816974296902328589, 73.97634902203346030 ) ) ;
#2071 = VERTEX_POINT ( 'NONE', #19171 ) ;
#2072 = LINE ( 'NONE', #10448, #14918 ) ;
#2073 = CARTESIAN_POINT ( 'NONE',  ( -10.55151208239364635, -17.68521041179895548, 68.28217381303441869 ) ) ;
#2074 = ORIENTED_EDGE ( 'NONE', *, *, #44042, .T. ) ;
#2075 = DIRECTION ( 'NONE',  ( -9.444166282346144476E-07, 1.975884201625194781E-06, 0.9999999999976019183 ) ) ;
#2076 = CARTESIAN_POINT ( 'NONE',  ( -13.07710726710083193, -16.59225537930583982, 52.02966884056656482 ) ) ;
#2077 = ADVANCED_FACE ( 'NONE', ( #8584 ), #41836, .F. ) ;
#2078 = CARTESIAN_POINT ( 'NONE',  ( -16.73854499263307716, -21.82594486583910864, 68.70120449160850740 ) ) ;
#2079 = CARTESIAN_POINT ( 'NONE',  ( -11.04812374654697926, -17.69862217806955229, 71.86718199155660614 ) ) ;
#2080 = ORIENTED_EDGE ( 'NONE', *, *, #22426, .F. ) ;
#2081 = CARTESIAN_POINT ( 'NONE',  ( -14.31331640305492847, -8.538396089775591946, 67.36861181020977085 ) ) ;
#2082 = CARTESIAN_POINT ( 'NONE',  ( -23.19494587819374942, -18.77118419879135303, 66.12389430422854275 ) ) ;
#2083 = CYLINDRICAL_SURFACE ( 'NONE', #41994, 0.1500000000000002998 ) ;
#2084 = AXIS2_PLACEMENT_3D ( 'NONE', #2444, #35672, #25098 ) ;
#2085 = AXIS2_PLACEMENT_3D ( 'NONE', #979, #11565, #27073 ) ;
#2086 = DIRECTION ( 'NONE',  ( -0.02843338833657841139, 0.4463087971659328024, 0.8944271909999156334 ) ) ;
#2087 = CYLINDRICAL_SURFACE ( 'NONE', #28208, 1.999999999999999112 ) ;
#2088 = CARTESIAN_POINT ( 'NONE',  ( -27.42409385541305511, -25.10920654474410441, 78.99999999999998579 ) ) ;
#2089 = EDGE_CURVE ( 'NONE', #38102, #21018, #1580, .T. ) ;
#2090 = DIRECTION ( 'NONE',  ( -7.105595949593054157E-06, -6.912614924914188927E-07, 0.9999999999745162738 ) ) ;
#2091 = LINE ( 'NONE', #32840, #26751 ) ;
#2092 = VERTEX_POINT ( 'NONE', #18668 ) ;
#2093 = CARTESIAN_POINT ( 'NONE',  ( -13.89754221028031189, -8.246728053280408588, 74.29980400178126843 ) ) ;
#2094 = CARTESIAN_POINT ( 'NONE',  ( -20.16691314815865255, -21.73601827195274794, 72.58974169946205279 ) ) ;
#2095 = CARTESIAN_POINT ( 'NONE',  ( -24.29779380370725406, -16.39214576242591193, 62.68508962089565273 ) ) ;
#2096 = ORIENTED_EDGE ( 'NONE', *, *, #6143, .T. ) ;
#2097 = CARTESIAN_POINT ( 'NONE',  ( -19.74200936563730124, -21.46758226568296024, 68.94954551542706156 ) ) ;
#2098 = ORIENTED_EDGE ( 'NONE', *, *, #46762, .T. ) ;
#2099 = EDGE_LOOP ( 'NONE', ( #8926, #32290, #25724, #17549, #12791 ) ) ;
#2100 = VERTEX_POINT ( 'NONE', #11302 ) ;
#2101 = EDGE_CURVE ( 'NONE', #47078, #1710, #26793, .T. ) ;
#2102 = CARTESIAN_POINT ( 'NONE',  ( -10.03204778417131315, -15.73800432700728891, 61.19822393253001991 ) ) ;
#2103 = EDGE_CURVE ( 'NONE', #46918, #14429, #23355, .T. ) ;
#2104 = CYLINDRICAL_SURFACE ( 'NONE', #13770, 0.1500000000000006883 ) ;
#2105 = B_SPLINE_CURVE_WITH_KNOTS ( 'NONE', 3,
 ( #5626, #18991, #19905, #8836, #31223, #12752, #12507, #20636, #1176, #35147 ),
 .UNSPECIFIED., .F., .F.,
 ( 4, 2, 2, 2, 4 ),
 ( 0.000000000000000000, 0.2500000000000000000, 0.5000000000000000000, 0.7500000000000000000, 1.000000000000000000 ),
 .UNSPECIFIED. ) ;
#2106 =( BOUNDED_CURVE ( )  B_SPLINE_CURVE ( 3, ( #27989, #35377, #46720, #12962 ),
 .UNSPECIFIED., .F., .F. ) 
 B_SPLINE_CURVE_WITH_KNOTS ( ( 4, 4 ),
 ( 1.570796326794896780, 1.780235837034217727 ),
 .UNSPECIFIED. ) 
 CURVE ( )  GEOMETRIC_REPRESENTATION_ITEM ( )  RATIONAL_B_SPLINE_CURVE ( ( 1.000000000000000000, 0.9963479302455154896, 0.9963479302455154896, 1.000000000000000000 ) ) 
 REPRESENTATION_ITEM ( '' )  );
#2107 = CYLINDRICAL_SURFACE ( 'NONE', #34581, 0.1499999999999994671 ) ;
#2108 = CARTESIAN_POINT ( 'NONE',  ( -19.83021825064065524, -21.38439211167239051, 72.52195586376959113 ) ) ;
#2109 = CARTESIAN_POINT ( 'NONE',  ( -10.74141492653277119, -16.89327574454988223, 57.68760574265544250 ) ) ;
#2110 = VERTEX_POINT ( 'NONE', #38350 ) ;
#2111 = ORIENTED_EDGE ( 'NONE', *, *, #20851, .T. ) ;
#2112 = ADVANCED_FACE ( 'NONE', ( #7867 ), #22887, .T. ) ;
#2113 = CARTESIAN_POINT ( 'NONE',  ( -19.74284385650551599, -8.811426318492348031, 52.18089403414751359 ) ) ;
#2114 = CARTESIAN_POINT ( 'NONE',  ( -24.28619334359350290, -16.42731978468327014, 59.13804568661029037 ) ) ;
#2115 = DIRECTION ( 'NONE',  ( -0.000000000000000000, -1.000000000000000000, -0.000000000000000000 ) ) ;
#2116 = EDGE_CURVE ( 'NONE', #32914, #3385, #19945, .T. ) ;
#2117 = CARTESIAN_POINT ( 'NONE',  ( -20.98034385650551314, -6.424090610841176385, 49.80797279389977916 ) ) ;
#2118 = B_SPLINE_CURVE_WITH_KNOTS ( 'NONE', 1,
 ( #25903, #37199 ),
 .UNSPECIFIED., .F., .F.,
 ( 2, 2 ),
 ( 0.000000000000000000, 1.000000000000000000 ),
 .UNSPECIFIED. ) ;
#2119 =( BOUNDED_CURVE ( )  B_SPLINE_CURVE ( 3, ( #13062, #28100, #41735, #30667 ),
 .UNSPECIFIED., .F., .F. ) 
 B_SPLINE_CURVE_WITH_KNOTS ( ( 4, 4 ),
 ( 0.4074455897393666204, 0.5000000000000000000 ),
 .UNSPECIFIED. ) 
 CURVE ( )  GEOMETRIC_REPRESENTATION_ITEM ( )  RATIONAL_B_SPLINE_CURVE ( ( 0.6983129098260953960, 0.7760317562607160768, 0.8765941196520221634, 1.000000000000025091 ) ) 
 REPRESENTATION_ITEM ( '' )  );
#2120 = VECTOR ( 'NONE', #27838, 1000.000000000000000 ) ;
#2121 = CIRCLE ( 'NONE', #44582, 1.999999999999999556 ) ;
#2122 = ORIENTED_EDGE ( 'NONE', *, *, #47124, .F. ) ;
#2123 = DIRECTION ( 'NONE',  ( 0.000000000000000000, -0.000000000000000000, 1.000000000000000000 ) ) ;
#2124 = CARTESIAN_POINT ( 'NONE',  ( -10.47425561207849753, -17.49314520081206936, 64.81234810402725088 ) ) ;
#2125 = VERTEX_POINT ( 'NONE', #47160 ) ;
#2126 = CYLINDRICAL_SURFACE ( 'NONE', #37468, 0.1499999999999955536 ) ;
#2127 = CARTESIAN_POINT ( 'NONE',  ( -22.39379392724509898, -9.879492423591733186, 73.59047181297640350 ) ) ;
#2128 = CARTESIAN_POINT ( 'NONE',  ( -16.24765015213137076, -21.70976432975602677, 58.58585518740712672 ) ) ;
#2129 = ORIENTED_EDGE ( 'NONE', *, *, #8208, .T. ) ;
#2130 = CARTESIAN_POINT ( 'NONE',  ( -19.99112905230247961, -8.296885111154901793, 73.72096600045514947 ) ) ;
#2131 = EDGE_CURVE ( 'NONE', #42275, #26781, #2091, .T. ) ;
#2132 = CARTESIAN_POINT ( 'NONE',  ( 18.57590614458695200, 3.151498850453765321, 50.28409723815717314 ) ) ;
#2133 = ORIENTED_EDGE ( 'NONE', *, *, #7357, .T. ) ;
#2134 = DIRECTION ( 'NONE',  ( -3.071710424422018668E-17, 6.404604876783312462E-16, 1.000000000000000000 ) ) ;
#2135 = VERTEX_POINT ( 'NONE', #38612 ) ;
#2136 = CYLINDRICAL_SURFACE ( 'NONE', #21103, 0.1500000000000035194 ) ;
#2137 = FACE_OUTER_BOUND ( 'NONE', #36078, .T. ) ;
#2138 = EDGE_LOOP ( 'NONE', ( #7753, #21053, #39584, #11585, #9532 ) ) ;
#2139 = CARTESIAN_POINT ( 'NONE',  ( -14.35043204381087101, -18.34698626059704551, 49.52966884056656482 ) ) ;
#2140 = DIRECTION ( 'NONE',  ( 1.702402328345536248E-17, -7.068183862238076217E-18, 1.000000000000000000 ) ) ;
#2141 = CARTESIAN_POINT ( 'NONE',  ( -24.48810873059073856, -17.17637193698283582, 73.06831349224263761 ) ) ;
#2142 = CARTESIAN_POINT ( 'NONE',  ( -21.19137721460013779, -21.23655545966798996, 65.77792262113059962 ) ) ;
#2143 = ORIENTED_EDGE ( 'NONE', *, *, #2952, .T. ) ;
#2144 = CARTESIAN_POINT ( 'NONE',  ( -22.06133474718976117, -9.563836317021298328, 59.79341455809256445 ) ) ;
#2145 = CARTESIAN_POINT ( 'NONE',  ( -11.29134393598116759, -11.33126488396075437, 64.16354160640879911 ) ) ;
#2146 = FACE_OUTER_BOUND ( 'NONE', #41416, .T. ) ;
#2147 = ORIENTED_EDGE ( 'NONE', *, *, #36326, .F. ) ;
#2148 = FACE_OUTER_BOUND ( 'NONE', #24875, .T. ) ;
#2149 = CONICAL_SURFACE ( 'NONE', #9230, 0.5560000000000009379, 0.06981317007976595157 ) ;
#2150 = VECTOR ( 'NONE', #9834, 1000.000000000000000 ) ;
#2151 = CARTESIAN_POINT ( 'NONE',  ( -12.05749060505181269, -9.640721912800795934, 60.74573338552316670 ) ) ;
#2152 = ORIENTED_EDGE ( 'NONE', *, *, #31958, .T. ) ;
#2153 = VERTEX_POINT ( 'NONE', #42569 ) ;
#2154 = CARTESIAN_POINT ( 'NONE',  ( -17.42409385541299471, -14.80920654474435594, 52.02966884056656482 ) ) ;
#2155 = CARTESIAN_POINT ( 'NONE',  ( -11.45752044641470668, -19.27057170535650954, 71.87181270239314301 ) ) ;
#2156 = ADVANCED_FACE ( 'NONE', ( #20141 ), #39760, .T. ) ;
#2157 = CARTESIAN_POINT ( 'NONE',  ( -13.43773910423563400, -20.62433115109003268, 58.33177939114180788 ) ) ;
#2158 = AXIS2_PLACEMENT_3D ( 'NONE', #31094, #42182, #35506 ) ;
#2159 = CARTESIAN_POINT ( 'NONE',  ( -17.68659385650551741, -9.302874398569244363, 51.68646062012417985 ) ) ;
#2160 = CARTESIAN_POINT ( 'NONE',  ( -18.32857646159318676, -22.20418385865972155, 68.93019298464047040 ) ) ;
#2161 = CARTESIAN_POINT ( 'NONE',  ( -19.48828226429125365, -21.49800194790059038, 62.28038260443739205 ) ) ;
#2162 = CARTESIAN_POINT ( 'NONE',  ( -23.81024772113315890, -18.64597811008791695, 72.94863512192290500 ) ) ;
#2163 = DIRECTION ( 'NONE',  ( 2.654446662475610288E-06, -3.134491601460476904E-06, 0.9999999999915645255 ) ) ;
#2164 = CARTESIAN_POINT ( 'NONE',  ( -13.90650143624606017, -21.37666829811961478, 72.08641044951055221 ) ) ;
#2165 = ORIENTED_EDGE ( 'NONE', *, *, #6143, .F. ) ;
#2166 = ORIENTED_EDGE ( 'NONE', *, *, #44966, .F. ) ;
#2167 = EDGE_CURVE ( 'NONE', #3943, #30787, #25048, .T. ) ;
#2168 = CARTESIAN_POINT ( 'NONE',  ( -24.31477923169101629, -16.30090137217950996, 59.40860294853779777 ) ) ;
#2169 = CARTESIAN_POINT ( 'NONE',  ( -41.91674091423659121, -14.90920654474421170, 67.05882352941175384 ) ) ;
#2170 = CARTESIAN_POINT ( 'NONE',  ( -19.42045769886998841, -21.57377358197381412, 65.87974951360257592 ) ) ;
#2171 = CARTESIAN_POINT ( 'NONE',  ( -13.47433711440449144, -8.491526086692950059, 57.15623147539552917 ) ) ;
#2172 = ADVANCED_FACE ( 'NONE', ( #12508 ), #24758, .T. ) ;
#2173 = CARTESIAN_POINT ( 'NONE',  ( -20.88270717056239789, -21.40782548341276481, 58.82970473467946704 ) ) ;
#2174 = CARTESIAN_POINT ( 'NONE',  ( -21.62409385650551741, -6.426201560718812544, 50.50509628382439331 ) ) ;
#2175 = ORIENTED_EDGE ( 'NONE', *, *, #39104, .F. ) ;
#2176 = CARTESIAN_POINT ( 'NONE',  ( -23.27284462870851911, -18.74605969774991010, 66.10917289053097079 ) ) ;
#2177 = DIRECTION ( 'NONE',  ( 0.02400335114476204179, -0.9997118780597843424, -1.529429985666831130E-10 ) ) ;
#2178 = CARTESIAN_POINT ( 'NONE',  ( -22.10679845867080928, -14.99777973644470919, 52.02966884056656482 ) ) ;
#2179 = VECTOR ( 'NONE', #10449, 1000.000000000000000 ) ;
#2180 = CARTESIAN_POINT ( 'NONE',  ( -18.17062816029565653, -22.22171889179154292, 65.44508531174115262 ) ) ;
#2181 = EDGE_CURVE ( 'NONE', #46754, #13759, #44059, .T. ) ;
#2182 = ORIENTED_EDGE ( 'NONE', *, *, #13017, .F. ) ;
#2183 = CARTESIAN_POINT ( 'NONE',  ( -10.14072131497136198, -13.24157352934983578, 74.83964170301820218 ) ) ;
#2184 = CIRCLE ( 'NONE', #19484, 0.5560000000000009379 ) ;
#2185 = ADVANCED_FACE ( 'NONE', ( #34911 ), #10463, .T. ) ;
#2186 = CARTESIAN_POINT ( 'NONE',  ( -14.74690617566109019, -21.27702427001963414, 58.46617884968173229 ) ) ;
#2187 = ADVANCED_FACE ( 'NONE', ( #13640 ), #40259, .T. ) ;
#2188 = CARTESIAN_POINT ( 'NONE',  ( -17.72612443559818018, -7.765381109175947927, 60.36588690973874094 ) ) ;
#2189 = VECTOR ( 'NONE', #17984, 1000.000000000000227 ) ;
#2190 = CARTESIAN_POINT ( 'NONE',  ( -15.62840352080693407, -7.578723969186683895, 70.73272974284665793 ) ) ;
#2191 = CARTESIAN_POINT ( 'NONE',  ( -11.09893839327029674, -10.87261039219572289, 57.38620067505767963 ) ) ;
#2192 = CARTESIAN_POINT ( 'NONE',  ( -24.39763799706551950, -15.84669482609578317, 69.54779622430706354 ) ) ;
#2193 = EDGE_LOOP ( 'NONE', ( #17391, #27532, #19360, #48710, #15901 ) ) ;
#2194 = CARTESIAN_POINT ( 'NONE',  ( -17.42409385541300892, -14.80920654474439324, 54.49999999999995026 ) ) ;
#2195 = VECTOR ( 'NONE', #353, 1000.000000000000000 ) ;
#2196 = EDGE_LOOP ( 'NONE', ( #24186, #38155, #39682, #34907, #5739 ) ) ;
#2197 = CARTESIAN_POINT ( 'NONE',  ( -13.60238289842205894, -8.884932333444998775, 57.26967755503795132 ) ) ;
#2198 = CARTESIAN_POINT ( 'NONE',  ( -12.68532267716109985, -9.060482739934947460, 71.03420753023118550 ) ) ;
#2199 = ORIENTED_EDGE ( 'NONE', *, *, #8542, .T. ) ;
#2200 = CARTESIAN_POINT ( 'NONE',  ( -14.79284385650551492, -7.406986770994972602, 48.81910596585309747 ) ) ;
#2201 = EDGE_LOOP ( 'NONE', ( #2898, #13217, #22546, #31209, #5524 ) ) ;
#2202 = CARTESIAN_POINT ( 'NONE',  ( -10.88209242003807908, -17.29963164818252608, 64.62739380462950578 ) ) ;
#2203 = CARTESIAN_POINT ( 'NONE',  ( -16.59509239138002101, -21.81331869282671221, 61.64079261740195648 ) ) ;
#2204 = B_SPLINE_CURVE_WITH_KNOTS ( 'NONE', 1,
 ( #8286, #38293 ),
 .UNSPECIFIED., .F., .F.,
 ( 2, 2 ),
 ( 0.000000000000000000, 1.000000000000000000 ),
 .UNSPECIFIED. ) ;
#2205 = VERTEX_POINT ( 'NONE', #6277 ) ;
#2206 = CARTESIAN_POINT ( 'NONE',  ( -21.13745558015973103, -11.09794736473739718, 50.77966884056655772 ) ) ;
#2207 = FACE_OUTER_BOUND ( 'NONE', #30152, .T. ) ;
#2208 = DIRECTION ( 'NONE',  ( -1.000000000000000000, -1.669677910507523057E-21, -6.493791346278465266E-22 ) ) ;
#2209 = CARTESIAN_POINT ( 'NONE',  ( -19.07667242297576138, -10.41096375660395168, 49.52966884056655772 ) ) ;
#2210 = EDGE_LOOP ( 'NONE', ( #34424, #7088, #36305, #33321, #23569 ) ) ;
#2211 = ORIENTED_EDGE ( 'NONE', *, *, #19807, .F. ) ;
#2212 = CARTESIAN_POINT ( 'NONE',  ( -11.70705814868712835, -18.84866425382743671, 68.21689578225554840 ) ) ;
#2213 = CARTESIAN_POINT ( 'NONE',  ( -21.30368986256526043, -21.17021271237730318, 69.24105570176159574 ) ) ;
#2214 = VERTEX_POINT ( 'NONE', #21052 ) ;
#2216 = CARTESIAN_POINT ( 'NONE',  ( -17.74687306060290837, -7.816529701066174951, 60.08060757092961524 ) ) ;
#2215 = CIRCLE ( 'NONE', #14755, 1.000000000000000888 ) ;
#2217 = DIRECTION ( 'NONE',  ( -0.9979768094191907579, -0.06357898915123130767, 0.000000000000000000 ) ) ;
#2218 = CARTESIAN_POINT ( 'NONE',  ( -19.63034385759799605, -6.857644439848013640, 49.98602051094139398 ) ) ;
#2219 = DIRECTION ( 'NONE',  ( 1.000000000000000000, -4.164305804376849172E-17, 1.614929280266638808E-16 ) ) ;
#2220 = AXIS2_PLACEMENT_3D ( 'NONE', #12101, #45356, #41402 ) ;
#2221 = DIRECTION ( 'NONE',  ( 0.000000000000000000, 0.000000000000000000, -1.000000000000000000 ) ) ;
#2222 = CARTESIAN_POINT ( 'NONE',  ( -12.40526392040721682, -9.927684496520663870, 60.63088272232361930 ) ) ;
#2223 = AXIS2_PLACEMENT_3D ( 'NONE', #6931, #44372, #25887 ) ;
#2224 = ORIENTED_EDGE ( 'NONE', *, *, #20934, .T. ) ;
#2225 = ADVANCED_FACE ( 'NONE', ( #32615 ), #13400, .T. ) ;
#2226 = CARTESIAN_POINT ( 'NONE',  ( -22.14133254371160930, -20.05921860014851532, 69.31850691956374533 ) ) ;
#2227 = CARTESIAN_POINT ( 'NONE',  ( -21.57657733182563931, -11.59682721189464871, 52.02966884056656482 ) ) ;
#2228 = CARTESIAN_POINT ( 'NONE',  ( -12.47302444406249933, -9.241390648102244754, 74.43267637782378188 ) ) ;
#2229 = PLANE ( 'NONE',  #26908 ) ;
#2230 = ORIENTED_EDGE ( 'NONE', *, *, #32245, .F. ) ;
#2231 = B_SPLINE_CURVE_WITH_KNOTS ( 'NONE', 3,
 ( #37857, #11767, #26788, #41811, #37349, #23099, #18640, #4371, #19389, #33652 ),
 .UNSPECIFIED., .F., .F.,
 ( 4, 2, 2, 2, 4 ),
 ( 0.000000000000000000, 0.2500000000000000000, 0.5000000000000000000, 0.7500000000000000000, 1.000000000000000000 ),
 .UNSPECIFIED. ) ;
#2232 = ORIENTED_EDGE ( 'NONE', *, *, #6046, .T. ) ;
#2233 = DIRECTION ( 'NONE',  ( 0.9687793358424821033, -0.2479245821708679909, 0.000000000000000000 ) ) ;
#2234 = CARTESIAN_POINT ( 'NONE',  ( -19.83346284351035393, -21.43866980266018274, 65.46486087551818400 ) ) ;
#2235 = DIRECTION ( 'NONE',  ( 3.071710424422018668E-17, -6.404604876783312462E-16, -1.000000000000000000 ) ) ;
#2236 =( BOUNDED_CURVE ( )  B_SPLINE_CURVE ( 3, ( #4241, #12585, #19980, #5455 ),
 .UNSPECIFIED., .F., .F. ) 
 B_SPLINE_CURVE_WITH_KNOTS ( ( 4, 4 ),
 ( 0.000000000000000000, 0.4074455897393641779 ),
 .UNSPECIFIED. ) 
 CURVE ( )  GEOMETRIC_REPRESENTATION_ITEM ( )  RATIONAL_B_SPLINE_CURVE ( ( 1.000000000000000000, 0.4567392136813311909, 0.3561768502900300448, 0.6983129098260966172 ) ) 
 REPRESENTATION_ITEM ( '' )  );
#2237 = ORIENTED_EDGE ( 'NONE', *, *, #23244, .T. ) ;
#2238 = ADVANCED_FACE ( 'NONE', ( #32141 ), #2953, .T. ) ;
#2239 = DIRECTION ( 'NONE',  ( -3.071710424422018668E-17, 6.404604876783312462E-16, 1.000000000000000000 ) ) ;
#2240 = CARTESIAN_POINT ( 'NONE',  ( -10.00761937521931522, -15.51608998476985946, 57.75288115419267854 ) ) ;
#2241 = ADVANCED_FACE ( 'NONE', ( #47640 ), #6431, .T. ) ;
#2242 = EDGE_CURVE ( 'NONE', #9318, #12877, #15099, .T. ) ;
#2243 = VERTEX_POINT ( 'NONE', #10690 ) ;
#2244 = CARTESIAN_POINT ( 'NONE',  ( -11.35719102664687874, -18.40077844947705543, 58.09242476654641507 ) ) ;
#2245 = AXIS2_PLACEMENT_3D ( 'NONE', #4042, #46368, #1060 ) ;
#2246 = CARTESIAN_POINT ( 'NONE',  ( -12.88266153074016529, -9.482350759114249072, 70.95811324639576867 ) ) ;
#2247 =( GEOMETRIC_REPRESENTATION_CONTEXT ( 3 ) GLOBAL_UNCERTAINTY_ASSIGNED_CONTEXT ( ( #43031 ) ) GLOBAL_UNIT_ASSIGNED_CONTEXT ( ( #15533, #27609, #34253 ) ) REPRESENTATION_CONTEXT ( 'NONE', 'WORKASPACE' ) );
#2248 = ORIENTED_EDGE ( 'NONE', *, *, #44277, .F. ) ;
#2249 = CARTESIAN_POINT ( 'NONE',  ( -22.71059208588729561, -10.14448404190931186, 70.02650598627910483 ) ) ;
#2250 = ORIENTED_EDGE ( 'NONE', *, *, #12608, .T. ) ;
#2251 =( BOUNDED_CURVE ( )  B_SPLINE_CURVE ( 3, ( #18763, #44636, #21976, #3260 ),
 .UNSPECIFIED., .F., .F. ) 
 B_SPLINE_CURVE_WITH_KNOTS ( ( 4, 4 ),
 ( 0.000000000000000000, 0.4074455897279358751 ),
 .UNSPECIFIED. ) 
 CURVE ( )  GEOMETRIC_REPRESENTATION_ITEM ( )  RATIONAL_B_SPLINE_CURVE ( ( 1.000000000000000000, 0.4567392136965727767, 0.3561768502956727533, 0.6983129097972999855 ) ) 
 REPRESENTATION_ITEM ( '' )  );
#2252 = LINE ( 'NONE', #10130, #2355 ) ;
#2253 = CIRCLE ( 'NONE', #29790, 1.250000000000001110 ) ;
#2254 = ORIENTED_EDGE ( 'NONE', *, *, #41350, .F. ) ;
#2255 = CARTESIAN_POINT ( 'NONE',  ( -15.95707318215220205, -7.504986700048139170, 63.85506303619484214 ) ) ;
#2256 = CARTESIAN_POINT ( 'NONE',  ( -18.33659385759798965, -8.995762431863214559, 51.38120296130585274 ) ) ;
#2257 = LINE ( 'NONE', #12616, #35981 ) ;
#2258 = VERTEX_POINT ( 'NONE', #34061 ) ;
#2259 = LINE ( 'NONE', #42431, #35652 ) ;
#2260 = CARTESIAN_POINT ( 'NONE',  ( -24.21281492007539526, -12.87834259335418530, 73.38658464541695992 ) ) ;
#2261 = CARTESIAN_POINT ( 'NONE',  ( -13.01616685277437568, -9.306763517318225709, 70.86397465682092900 ) ) ;
#2262 = AXIS2_PLACEMENT_3D ( 'NONE', #44784, #42047, #11034 ) ;
#2263 = CARTESIAN_POINT ( 'NONE',  ( -50.42409385541305511, -15.80920654474410725, 74.99999999999998579 ) ) ;
#2264 = CARTESIAN_POINT ( 'NONE',  ( -10.45720011525486015, -15.50224624050967037, 61.10959345291067280 ) ) ;
#2265 = LINE ( 'NONE', #23962, #17172 ) ;
#2266 = ORIENTED_EDGE ( 'NONE', *, *, #29882, .F. ) ;
#2267 = CARTESIAN_POINT ( 'NONE',  ( -21.44055400477819973, -12.39439182751215718, 49.52966884056655772 ) ) ;
#2268 =( BOUNDED_CURVE ( )  B_SPLINE_CURVE ( 3, ( #46000, #11783, #4161, #5121 ),
 .UNSPECIFIED., .F., .F. ) 
 B_SPLINE_CURVE_WITH_KNOTS ( ( 4, 4 ),
 ( 0.5000000000000000000, 0.9074455897393647330 ),
 .UNSPECIFIED. ) 
 CURVE ( )  GEOMETRIC_REPRESENTATION_ITEM ( )  RATIONAL_B_SPLINE_CURVE ( ( 1.000000000000011324, 0.4567392136813218095, 0.3561768502900186650, 0.6983129098261137147 ) ) 
 REPRESENTATION_ITEM ( '' )  );
#2269 = CARTESIAN_POINT ( 'NONE',  ( -24.66912536856318994, -13.07314766736345746, 62.95547313412625101 ) ) ;
#2270 = DIRECTION ( 'NONE',  ( 0.5729733056696845184, -0.8195740302071247152, -7.403245353804670970E-08 ) ) ;
#2271 = LINE ( 'NONE', #14047, #18701 ) ;
#2272 = CARTESIAN_POINT ( 'NONE',  ( -15.87557863975121641, -7.931372594209569193, 67.14007279017359053 ) ) ;
#2273 = CARTESIAN_POINT ( 'NONE',  ( -19.07667242297576138, -10.41096375660394990, 52.02966884056656482 ) ) ;
#2274 = EDGE_CURVE ( 'NONE', #30416, #44513, #43256, .T. ) ;
#2275 = VERTEX_POINT ( 'NONE', #14350 ) ;
#2276 = CARTESIAN_POINT ( 'NONE',  ( -9.424093855413051557, -27.10920654474410796, 77.00000000000000000 ) ) ;
#2277 = CARTESIAN_POINT ( 'NONE',  ( -24.82492784865917201, -15.66438054851105832, 73.25949685721523963 ) ) ;
#2278 = ORIENTED_EDGE ( 'NONE', *, *, #38859, .T. ) ;
#2279 = CARTESIAN_POINT ( 'NONE',  ( -10.36968235478426870, -15.03336378326449285, 71.48349971081816534 ) ) ;
#2280 = FACE_OUTER_BOUND ( 'NONE', #266, .T. ) ;
#2281 = CARTESIAN_POINT ( 'NONE',  ( -50.42609385541305755, -14.80920654474415699, 62.92941176470587550 ) ) ;
#2282 = CARTESIAN_POINT ( 'NONE',  ( -22.62394951084894146, -10.04809318868971424, 70.29706442286226320 ) ) ;
#2283 = DIRECTION ( 'NONE',  ( 0.000000000000000000, 0.000000000000000000, 1.000000000000000000 ) ) ;
#2284 = ORIENTED_EDGE ( 'NONE', *, *, #40405, .F. ) ;
#2285 = CARTESIAN_POINT ( 'NONE',  ( -24.83515304063678286, -14.04764234229505959, 73.23776096988058271 ) ) ;
#2286 = CARTESIAN_POINT ( 'NONE',  ( -50.42609385541305755, -14.80920654474415699, 62.02941176470587692 ) ) ;
#2287 = EDGE_LOOP ( 'NONE', ( #25145, #9987, #602, #9804, #31501 ) ) ;
#2288 = DIRECTION ( 'NONE',  ( 6.374839753205895344E-22, 0.007114381193220357599, -0.9999746924698832418 ) ) ;
#2289 = CARTESIAN_POINT ( 'NONE',  ( -21.62409385541304374, -9.359200813967568422, 50.49621490985803263 ) ) ;
#2290 = EDGE_CURVE ( 'NONE', #38294, #3327, #43871, .T. ) ;
#2291 = AXIS2_PLACEMENT_3D ( 'NONE', #23123, #45785, #8341 ) ;
#2292 = CARTESIAN_POINT ( 'NONE',  ( -13.33887157028844150, -9.124797958614562887, 64.20946578470248767 ) ) ;
#2293 = AXIS2_PLACEMENT_3D ( 'NONE', #5647, #20655, #31970 ) ;
#2294 = CARTESIAN_POINT ( 'NONE',  ( -24.14992822999210276, -18.01341164000503525, 59.11882993461590274 ) ) ;
#2295 = FACE_OUTER_BOUND ( 'NONE', #8756, .T. ) ;
#2296 = CARTESIAN_POINT ( 'NONE',  ( -11.52367966561213386, -11.04268899456634578, 57.20903262758894670 ) ) ;
#2297 = AXIS2_PLACEMENT_3D ( 'NONE', #33032, #47367, #13596 ) ;
#2298 = AXIS2_PLACEMENT_3D ( 'NONE', #46917, #1859, #6283 ) ;
#2299 = EDGE_LOOP ( 'NONE', ( #26074, #31385, #6841, #23143 ) ) ;
#2300 = VERTEX_POINT ( 'NONE', #3302 ) ;
#2301 = CARTESIAN_POINT ( 'NONE',  ( -19.59909385541304516, -8.105421454601382081, 49.25000573077640098 ) ) ;
#2302 = CARTESIAN_POINT ( 'NONE',  ( -10.37462440636232053, -14.89569459299594278, 75.09778901493891112 ) ) ;
#2303 = CARTESIAN_POINT ( 'NONE',  ( -12.83203711565397676, -20.76220377597121214, 54.02312124697528617 ) ) ;
#2304 = CIRCLE ( 'NONE', #42420, 0.5560000000000009379 ) ;
#2305 = DIRECTION ( 'NONE',  ( 1.000000000000000000, 0.000000000000000000, 0.000000000000000000 ) ) ;
#2306 = EDGE_CURVE ( 'NONE', #733, #9420, #33312, .T. ) ;
#2307 = CARTESIAN_POINT ( 'NONE',  ( -12.12094469647606942, -10.15824389949702322, 60.55918111604575671 ) ) ;
#2308 = ORIENTED_EDGE ( 'NONE', *, *, #39276, .T. ) ;
#2309 = FACE_OUTER_BOUND ( 'NONE', #25049, .T. ) ;
#2310 = CYLINDRICAL_SURFACE ( 'NONE', #27292, 2.000000000000001776 ) ;
#2311 = ORIENTED_EDGE ( 'NONE', *, *, #21050, .T. ) ;
#2312 = CARTESIAN_POINT ( 'NONE',  ( -17.98584164848810474, -22.23808382151284491, 62.06031347038508983 ) ) ;
#2313 = CARTESIAN_POINT ( 'NONE',  ( -17.08524326626993428, -7.816974356186509709, 74.24401709311408126 ) ) ;
#2314 = ORIENTED_EDGE ( 'NONE', *, *, #36771, .F. ) ;
#2315 = EDGE_CURVE ( 'NONE', #7630, #37913, #1099, .T. ) ;
#2316 = ADVANCED_FACE ( 'NONE', ( #14586 ), #37255, .T. ) ;
#2317 = CARTESIAN_POINT ( 'NONE',  ( -45.92409385541306932, -12.76354662275040042, 70.50000000000000000 ) ) ;
#2318 = CARTESIAN_POINT ( 'NONE',  ( -18.50162202296811742, -21.72577595440482057, 72.28510940981611554 ) ) ;
#2319 = EDGE_LOOP ( 'NONE', ( #48567, #44736, #34467, #39848, #16752 ) ) ;
#2320 = FACE_OUTER_BOUND ( 'NONE', #24702, .T. ) ;
#2321 = ADVANCED_FACE ( 'NONE', ( #37503 ), #9879, .T. ) ;
#2322 = CARTESIAN_POINT ( 'NONE',  ( -24.83498170362974022, -14.04605013716215822, 73.37917436033832530 ) ) ;
#2323 = ADVANCED_FACE ( 'NONE', ( #37756 ), #40479, .T. ) ;
#2324 = CARTESIAN_POINT ( 'NONE',  ( -15.49416032233947682, -8.028509233753512220, 74.07985659018983426 ) ) ;
#2325 = CARTESIAN_POINT ( 'NONE',  ( -22.57384314992541263, -19.55061350403557441, 72.87073974848900093 ) ) ;
#2326 = ORIENTED_EDGE ( 'NONE', *, *, #20906, .F. ) ;
#2327 = DIRECTION ( 'NONE',  ( -0.9991556020692448081, 0.04108628546905851442, 9.785000776664589550E-17 ) ) ;
#2328 = DIRECTION ( 'NONE',  ( 0.000000000000000000, 0.007114381193220285608, -0.9999746924698833528 ) ) ;
#2329 = CIRCLE ( 'NONE', #25920, 4.686500000000000554 ) ;
#2330 = PLANE ( 'NONE',  #34101 ) ;
#2331 = CARTESIAN_POINT ( 'NONE',  ( -11.96181355942711910, -19.87549434724351727, 58.11177690156993947 ) ) ;
#2332 = B_SPLINE_CURVE_WITH_KNOTS ( 'NONE', 3,
 ( #45193, #8016, #18564, #15600, #44699, #38013, #22036, #25974, #34314, #37032 ),
 .UNSPECIFIED., .F., .F.,
 ( 4, 2, 2, 2, 4 ),
 ( 0.6272669072877752328, 0.7522669073072968393, 0.8772669073268184459, 1.002266907346339941, 1.127266907365861659 ),
 .UNSPECIFIED. ) ;
#2333 = CARTESIAN_POINT ( 'NONE',  ( -24.72409385541305582, -14.90920654474417972, 64.04117647058822627 ) ) ;
#2334 = ADVANCED_FACE ( 'NONE', ( #7998 ), #8714, .T. ) ;
#2335 = CARTESIAN_POINT ( 'NONE',  ( -16.85302834907681557, -22.23803867529147738, 68.80905311428833215 ) ) ;
#2336 = CARTESIAN_POINT ( 'NONE',  ( -23.58616457878146377, -18.99640866789479432, 66.00884704819274873 ) ) ;
#2337 = ORIENTED_EDGE ( 'NONE', *, *, #735, .F. ) ;
#2338 = DIRECTION ( 'NONE',  ( 1.000000000000000000, -4.164305804376849172E-17, 1.614929280266638808E-16 ) ) ;
#2339 = AXIS2_PLACEMENT_3D ( 'NONE', #46570, #16501, #17223 ) ;
#2340 = CARTESIAN_POINT ( 'NONE',  ( -45.55409385541305767, -12.91120565595569936, 69.30071302485083606 ) ) ;
#2341 = CARTESIAN_POINT ( 'NONE',  ( -13.29033873113971076, -20.46027459610395027, 58.15723269990255062 ) ) ;
#2342 = VERTEX_POINT ( 'NONE', #11667 ) ;
#2343 = CYLINDRICAL_SURFACE ( 'NONE', #8224, 2.000000000000001776 ) ;
#2344 = VERTEX_POINT ( 'NONE', #35030 ) ;
#2345 = ORIENTED_EDGE ( 'NONE', *, *, #44104, .T. ) ;
#2346 = EDGE_LOOP ( 'NONE', ( #48110, #34485, #12786, #14619, #18151 ) ) ;
#2347 = CARTESIAN_POINT ( 'NONE',  ( -16.17465015159496744, -21.74764722426833075, 58.28585602925419806 ) ) ;
#2348 = CARTESIAN_POINT ( 'NONE',  ( -23.11004562739756096, -18.89484649831948104, 66.01316609496412013 ) ) ;
#2349 = CARTESIAN_POINT ( 'NONE',  ( -17.46222794319647775, -7.759011850482251837, 67.03511641684839617 ) ) ;
#2350 = CARTESIAN_POINT ( 'NONE',  ( -17.18480517372767125, -21.85814792571105514, 72.05054515682328997 ) ) ;
#2351 = CARTESIAN_POINT ( 'NONE',  ( -22.21784385759799108, -6.860780111191482789, 51.02154966934377001 ) ) ;
#2352 = ORIENTED_EDGE ( 'NONE', *, *, #41187, .T. ) ;
#2353 = VERTEX_POINT ( 'NONE', #34298 ) ;
#2354 = CARTESIAN_POINT ( 'NONE',  ( -18.44909385650551670, -8.104110260919579645, 48.81699501597546487 ) ) ;
#2355 = VECTOR ( 'NONE', #21692, 1000.000000000000000 ) ;
#2356 = CARTESIAN_POINT ( 'NONE',  ( -18.55956930788366677, -7.446158750330262421, 74.02559786541287679 ) ) ;
#2357 = DIRECTION ( 'NONE',  ( 0.4846961512978548159, 0.8746825943832683414, 4.196010046976494103E-08 ) ) ;
#2358 = VECTOR ( 'NONE', #20615, 999.9999999999998863 ) ;
#2359 = EDGE_CURVE ( 'NONE', #46199, #23813, #14442, .T. ) ;
#2360 = CARTESIAN_POINT ( 'NONE',  ( -18.67409385650551457, -9.792211528768504536, 50.49490371617623197 ) ) ;
#2361 = VECTOR ( 'NONE', #13653, 1000.000000000000000 ) ;
#2362 = ORIENTED_EDGE ( 'NONE', *, *, #2957, .F. ) ;
#2363 = ADVANCED_FACE ( 'NONE', ( #1298 ), #12634, .T. ) ;
#2364 = CARTESIAN_POINT ( 'NONE',  ( -10.37406300525030645, -14.84993649218493417, 74.80338706735179244 ) ) ;
#2365 = CARTESIAN_POINT ( 'NONE',  ( -24.87406966366976135, -14.83187089386463775, 59.34276618600990361 ) ) ;
#2366 = AXIS2_PLACEMENT_3D ( 'NONE', #41844, #37890, #716 ) ;
#2367 = VERTEX_POINT ( 'NONE', #11921 ) ;
#2368 = DIRECTION ( 'NONE',  ( 2.866981220435666553E-17, -1.000000000000000000, -1.190614954331866791E-16 ) ) ;
#2369 = ORIENTED_EDGE ( 'NONE', *, *, #38500, .F. ) ;
#2370 = CARTESIAN_POINT ( 'NONE',  ( -19.54284385541296842, -7.587656875400136336, 49.25157356644799478 ) ) ;
#2371 = CARTESIAN_POINT ( 'NONE',  ( -28.42409385541305511, -6.859206544744110623, 52.99999999999997158 ) ) ;
#2372 = CARTESIAN_POINT ( 'NONE',  ( -22.28468842640968006, -19.91619389767071269, 65.98949666203347419 ) ) ;
#2373 = EDGE_CURVE ( 'NONE', #2586, #15392, #2704, .T. ) ;
#2374 = VERTEX_POINT ( 'NONE', #5018 ) ;
#2375 = DIRECTION ( 'NONE',  ( 0.000000000000000000, 0.007114381193220344589, -0.9999746924698832418 ) ) ;
#2376 = EDGE_CURVE ( 'NONE', #38493, #28218, #38231, .T. ) ;
#2377 = CARTESIAN_POINT ( 'NONE',  ( -16.78659385541304161, -7.222650657624102521, 49.61879703869476543 ) ) ;
#2378 = CARTESIAN_POINT ( 'NONE',  ( -23.12302755141047683, -18.95946607990388699, 62.50406880580509750 ) ) ;
#2379 = ORIENTED_EDGE ( 'NONE', *, *, #11206, .F. ) ;
#2380 = CARTESIAN_POINT ( 'NONE',  ( -24.83168737706420615, -15.60343295348776138, 73.10965427473990985 ) ) ;
#2381 = CARTESIAN_POINT ( 'NONE',  ( -24.47853618617655158, -14.58602005854247174, 69.79708117814310242 ) ) ;
#2382 = ORIENTED_EDGE ( 'NONE', *, *, #22006, .T. ) ;
#2383 = CARTESIAN_POINT ( 'NONE',  ( -13.35685195715142193, -21.05109796036597913, 61.56000367517481919 ) ) ;
#2384 = FACE_OUTER_BOUND ( 'NONE', #40725, .T. ) ;
#2385 = ORIENTED_EDGE ( 'NONE', *, *, #5184, .T. ) ;
#2386 = CARTESIAN_POINT ( 'NONE',  ( -13.17196901619666605, -8.691656238230125453, 60.57803720896963995 ) ) ;
#2387 = CARTESIAN_POINT ( 'NONE',  ( -24.65023647254185590, -12.99629722456026393, 63.01759562046499497 ) ) ;
#2388 = CARTESIAN_POINT ( 'NONE',  ( -24.16424020987968646, -16.88652737071335252, 72.76847378359866525 ) ) ;
#2389 = B_SPLINE_CURVE_WITH_KNOTS ( 'NONE', 3,
 ( #16166, #12963, #20127, #19890, #19650, #42784, #31208, #15689, #34894, #1162 ),
 .UNSPECIFIED., .F., .F.,
 ( 4, 2, 2, 2, 4 ),
 ( 0.6272669072977071769, 0.7522669073147385532, 0.8772669073317700406, 1.002266907348801528, 1.127266907365832793 ),
 .UNSPECIFIED. ) ;
#2390 = VECTOR ( 'NONE', #515, 1000.000000000000114 ) ;
#2391 = DIRECTION ( 'NONE',  ( 4.267285103686815209E-17, -5.292884291094200710E-16, -1.000000000000000000 ) ) ;
#2392 = ORIENTED_EDGE ( 'NONE', *, *, #47249, .F. ) ;
#2393 = CYLINDRICAL_SURFACE ( 'NONE', #9540, 0.1500000000000057399 ) ;
#2394 = EDGE_CURVE ( 'NONE', #45181, #19972, #31347, .T. ) ;
#2395 = CARTESIAN_POINT ( 'NONE',  ( -24.14981099001045095, -11.60321323961852258, 59.59580478148293992 ) ) ;
#2396 =( BOUNDED_CURVE ( )  B_SPLINE_CURVE ( 3, ( #17141, #5621, #9554, #35389 ),
 .UNSPECIFIED., .F., .F. ) 
 B_SPLINE_CURVE_WITH_KNOTS ( ( 4, 4 ),
 ( 0.9074455897393687298, 1.000000000000000000 ),
 .UNSPECIFIED. ) 
 CURVE ( )  GEOMETRIC_REPRESENTATION_ITEM ( )  RATIONAL_B_SPLINE_CURVE ( ( 0.6983129098261148249, 0.7760317562607169650, 0.8765941196520120604, 1.000000000000000000 ) ) 
 REPRESENTATION_ITEM ( '' )  );
#2397 = CARTESIAN_POINT ( 'NONE',  ( -10.83536385990051798, -17.31742045656482176, 64.77739380450887552 ) ) ;
#2398 = ORIENTED_EDGE ( 'NONE', *, *, #23944, .T. ) ;
#2399 = CARTESIAN_POINT ( 'NONE',  ( -26.42409385541305511, -25.10920654474410441, 63.99999999999998579 ) ) ;
#2400 = AXIS2_PLACEMENT_3D ( 'NONE', #13486, #16931, #43054 ) ;
#2401 = CARTESIAN_POINT ( 'NONE',  ( -12.00971629994662493, -9.691756596678954949, 60.67422760384662439 ) ) ;
#2402 = ORIENTED_EDGE ( 'NONE', *, *, #40804, .F. ) ;
#2403 = EDGE_LOOP ( 'NONE', ( #47008, #18455, #19113, #12704, #9164 ) ) ;
#2404 = CARTESIAN_POINT ( 'NONE',  ( -24.18037300165767434, -17.94870813986570113, 59.18873840842728384 ) ) ;
#2405 = CARTESIAN_POINT ( 'NONE',  ( -13.11130243257871264, -9.228466417706050251, 63.79457649077198056 ) ) ;
#2406 = CARTESIAN_POINT ( 'NONE',  ( -10.02292926433220011, -15.66126330378499176, 61.23127357194864828 ) ) ;
#2407 = AXIS2_PLACEMENT_3D ( 'NONE', #1400, #15688, #34398 ) ;
#2408 = CARTESIAN_POINT ( 'NONE',  ( -19.09284385650552096, -7.406986770994973490, 48.81910596585309747 ) ) ;
#2409 = CARTESIAN_POINT ( 'NONE',  ( -14.92409385541305333, -14.80920654474410725, 45.99899999999998101 ) ) ;
#2410 = CARTESIAN_POINT ( 'NONE',  ( -23.52949419687348964, -11.28347464189849703, 70.17738639980606763 ) ) ;
#2411 = DIRECTION ( 'NONE',  ( -1.000000000000000000, -0.000000000000000000, -0.000000000000000000 ) ) ;
#2412 = CARTESIAN_POINT ( 'NONE',  ( -12.22131315432520537, -20.14153059940332824, 65.06686082697517293 ) ) ;
#2413 =( BOUNDED_SURFACE ( )  B_SPLINE_SURFACE ( 3, 1, ( 
 ( #12751, #39335 ),
 ( #46962, #12506 ),
 ( #27527, #43286 ),
 ( #42566, #8835 ),
 ( #23848, #27770 ),
 ( #38849, #14404 ),
 ( #44496, #44262 ) ),
 .UNSPECIFIED., .T., .F., .F. ) 
 B_SPLINE_SURFACE_WITH_KNOTS ( ( 4, 3, 4 ),
 ( 2, 2 ),
 ( 0.000000000000000000, 0.5000000000000000000, 1.000000000000000000 ),
 ( 0.000000000000000000, 1.000000000000000000 ),
 .UNSPECIFIED. ) 
 GEOMETRIC_REPRESENTATION_ITEM ( )  RATIONAL_B_SPLINE_SURFACE ( (
 ( 1.000000000000000000, 1.000000000000000000),
 ( 0.3333333333333335369, 0.3333333333333330373),
 ( 0.3333333333333335369, 0.3333333333333330373),
 ( 1.000000000000000000, 1.000000000000000000),
 ( 0.3333333333333333703, 0.3333333333333333703),
 ( 0.3333333333333333703, 0.3333333333333333703),
 ( 1.000000000000000000, 1.000000000000000000) ) ) 
 REPRESENTATION_ITEM ( '' )  SURFACE ( )  );
#2414 = CARTESIAN_POINT ( 'NONE',  ( -23.20936678059565494, -18.85217346302747643, 59.03977614772677640 ) ) ;
#2415 = ORIENTED_EDGE ( 'NONE', *, *, #29630, .F. ) ;
#2416 = ORIENTED_EDGE ( 'NONE', *, *, #36323, .T. ) ;
#2417 = DIRECTION ( 'NONE',  ( 0.000000000000000000, -0.9999954153791273948, -0.003028072113819838245 ) ) ;
#2418 = STYLED_ITEM ( 'NONE', ( #3339 ), #76 ) ;
#2419 = CARTESIAN_POINT ( 'NONE',  ( -23.08461988266076048, -9.965480423839858659, 66.64843946037336764 ) ) ;
#2420 = B_SPLINE_CURVE_WITH_KNOTS ( 'NONE', 1,
 ( #45954, #34611 ),
 .UNSPECIFIED., .F., .F.,
 ( 2, 2 ),
 ( 0.000000000000000000, 1.000000000000000000 ),
 .UNSPECIFIED. ) ;
#2421 = CARTESIAN_POINT ( 'NONE',  ( -27.51331730537552289, -17.63476259924578926, 53.49999999999995026 ) ) ;
#2422 = CARTESIAN_POINT ( 'NONE',  ( -10.99934521469463888, -17.58926687486790641, 71.85101586268936558 ) ) ;
#2423 = CARTESIAN_POINT ( 'NONE',  ( -11.09028998197301874, -11.82864193257709751, 71.10363318086781703 ) ) ;
#2424 = ADVANCED_FACE ( 'NONE', ( #31599 ), #4517, .T. ) ;
#2425 = CARTESIAN_POINT ( 'NONE',  ( -19.76784385650551812, -6.428312510596451368, 51.20221977374900035 ) ) ;
#2426 = ORIENTED_EDGE ( 'NONE', *, *, #46649, .T. ) ;
#2427 = CARTESIAN_POINT ( 'NONE',  ( -20.16691211377460391, -21.73601867580754288, 72.58974061177721637 ) ) ;
#2428 = CARTESIAN_POINT ( 'NONE',  ( -15.46621039653938112, -10.55127575485719760, 49.52966884056655772 ) ) ;
#2429 = AXIS2_PLACEMENT_3D ( 'NONE', #45470, #44997, #11245 ) ;
#2430 = CARTESIAN_POINT ( 'NONE',  ( -16.43682605374082684, -21.78988669087135222, 62.05008312678486249 ) ) ;
#2431 = CARTESIAN_POINT ( 'NONE',  ( -10.43098718212803000, -15.70539730037032911, 61.32316937334011442 ) ) ;
#2432 = ORIENTED_EDGE ( 'NONE', *, *, #42135, .F. ) ;
#2433 = VECTOR ( 'NONE', #11280, 1000.000000000000000 ) ;
#2434 = DIRECTION ( 'NONE',  ( -1.000000000000000000, 4.164305804376849172E-17, -1.614929280266638808E-16 ) ) ;
#2435 = LINE ( 'NONE', #40111, #21168 ) ;
#2436 = EDGE_CURVE ( 'NONE', #36242, #8916, #22700, .T. ) ;
#2437 = CARTESIAN_POINT ( 'NONE',  ( -15.61268995836261375, -7.582723730348911673, 70.80328162622285504 ) ) ;
#2438 = ADVANCED_FACE ( 'NONE', ( #46128 ), #46378, .T. ) ;
#2439 = PLANE ( 'NONE',  #31439 ) ;
#2440 = ORIENTED_EDGE ( 'NONE', *, *, #5872, .F. ) ;
#2441 = CARTESIAN_POINT ( 'NONE',  ( -20.72573862760241070, -8.580110178657996300, 60.14125250079693785 ) ) ;
#2442 = ORIENTED_EDGE ( 'NONE', *, *, #5184, .F. ) ;
#2443 = CARTESIAN_POINT ( 'NONE',  ( -24.36926384684218050, -16.02131533650774031, 66.06884749925394829 ) ) ;
#2444 = CARTESIAN_POINT ( 'NONE',  ( -45.92409385541306222, -14.80920654474410725, 70.50000000000000000 ) ) ;
#2445 = EDGE_CURVE ( 'NONE', #22471, #22864, #30025, .T. ) ;
#2446 = VERTEX_POINT ( 'NONE', #23974 ) ;
#2447 = DIRECTION ( 'NONE',  ( -3.071710424422018668E-17, 6.404604876783312462E-16, 1.000000000000000000 ) ) ;
#2448 = CIRCLE ( 'NONE', #37844, 1.999999999999999778 ) ;
#2449 = CARTESIAN_POINT ( 'NONE',  ( -12.56171917241870695, -20.45376946399996854, 71.99148991968543498 ) ) ;
#2450 = ORIENTED_EDGE ( 'NONE', *, *, #9696, .T. ) ;
#2451 = LINE ( 'NONE', #13984, #22078 ) ;
#2452 = EDGE_CURVE ( 'NONE', #3868, #47072, #33150, .T. ) ;
#2453 = CARTESIAN_POINT ( 'NONE',  ( -10.64577744754535082, -11.71757184301072563, 74.67344733366148546 ) ) ;
#2454 = CARTESIAN_POINT ( 'NONE',  ( -24.86287066056264550, -14.39952644145777327, 66.28954435112517274 ) ) ;
#2455 = ORIENTED_EDGE ( 'NONE', *, *, #40556, .T. ) ;
#2456 = CYLINDRICAL_SURFACE ( 'NONE', #14455, 1.999999999999999556 ) ;
#2457 = CARTESIAN_POINT ( 'NONE',  ( -17.19980177718173309, -7.762775310937221285, 70.49035839668022163 ) ) ;
#2458 = DIRECTION ( 'NONE',  ( -3.071710424422018668E-17, 6.404604876783312462E-16, 1.000000000000000000 ) ) ;
#2459 = VECTOR ( 'NONE', #6899, 1000.000000000000000 ) ;
#2460 = CARTESIAN_POINT ( 'NONE',  ( -11.31430947714633994, -19.07219073454920277, 68.36689628406799102 ) ) ;
#2461 = VERTEX_POINT ( 'NONE', #9440 ) ;
#2462 = ORIENTED_EDGE ( 'NONE', *, *, #320, .T. ) ;
#2463 = CARTESIAN_POINT ( 'NONE',  ( -11.72760323093659807, -18.87748041585143710, 68.50224213730197675 ) ) ;
#2464 = CARTESIAN_POINT ( 'NONE',  ( -11.01197672498281044, -17.74032467813711733, 71.85246142747087106 ) ) ;
#2465 = ORIENTED_EDGE ( 'NONE', *, *, #32444, .T. ) ;
#2466 = CARTESIAN_POINT ( 'NONE',  ( -50.42609385541305755, -14.80920654474412679, 59.01176470588234224 ) ) ;
#2467 = CARTESIAN_POINT ( 'NONE',  ( -18.73034385759799036, -6.857644439848013640, 49.98602051094139398 ) ) ;
#2468 = CARTESIAN_POINT ( 'NONE',  ( -22.88264614489240856, -10.34704276773305764, 63.35713876973677827 ) ) ;
#2469 = EDGE_CURVE ( 'NONE', #20234, #33331, #5750, .T. ) ;
#2470 = CARTESIAN_POINT ( 'NONE',  ( -13.89388974506275787, -21.36980381032900667, 72.11102993026078423 ) ) ;
#2471 = CARTESIAN_POINT ( 'NONE',  ( -15.55171241031346696, -7.598245096497682205, 70.79485117658632021 ) ) ;
#2472 = EDGE_CURVE ( 'NONE', #18626, #38687, #28140, .T. ) ;
#2473 = ORIENTED_EDGE ( 'NONE', *, *, #41030, .T. ) ;
#2474 = CYLINDRICAL_SURFACE ( 'NONE', #6091, 0.1499999999999986899 ) ;
#2475 = FACE_OUTER_BOUND ( 'NONE', #30961, .T. ) ;
#2476 = AXIS2_PLACEMENT_3D ( 'NONE', #39433, #5710, #32041 ) ;
#2477 = CARTESIAN_POINT ( 'NONE',  ( -22.83135259498468628, -9.684349502702678691, 73.68172289069366343 ) ) ;
#2478 = DIRECTION ( 'NONE',  ( 3.413470714839332458E-33, -1.190614954331866791E-16, 1.000000000000000000 ) ) ;
#2479 = EDGE_CURVE ( 'NONE', #1105, #31075, #36241, .T. ) ;
#2480 = ORIENTED_EDGE ( 'NONE', *, *, #3951, .F. ) ;
#2481 = EDGE_LOOP ( 'NONE', ( #42885, #32173, #36088, #32848 ) ) ;
#2482 = CARTESIAN_POINT ( 'NONE',  ( -17.56717618076180187, -7.360494862701306928, 63.73552352176282909 ) ) ;
#2483 = AXIS2_PLACEMENT_3D ( 'NONE', #18053, #41205, #10682 ) ;
#2484 = CARTESIAN_POINT ( 'NONE',  ( -22.63008487438422733, -10.12971324841507581, 70.31178520543817001 ) ) ;
#2485 = PLANE ( 'NONE',  #37833 ) ;
#2486 = SHAPE_REPRESENTATION ( 'Cylinder Spindle Drive Pinion', ( #29031 ), #29815 ) ;
#2487 = ORIENTED_EDGE ( 'NONE', *, *, #13354, .T. ) ;
#2488 = B_SPLINE_CURVE_WITH_KNOTS ( 'NONE', 1,
 ( #31694, #45991 ),
 .UNSPECIFIED., .F., .F.,
 ( 2, 2 ),
 ( 0.000000000000000000, 1.000000000000000000 ),
 .UNSPECIFIED. ) ;
#2489 = DIRECTION ( 'NONE',  ( -0.6771828760946863035, 0.7358147540815750398, -3.419290845356464001E-09 ) ) ;
#2490 = AXIS2_PLACEMENT_3D ( 'NONE', #46219, #42772, #12478 ) ;
#2491 = CARTESIAN_POINT ( 'NONE',  ( -10.92672688430831229, -11.16395088679539249, 64.40527978002718612 ) ) ;
#2492 = VERTEX_POINT ( 'NONE', #31837 ) ;
#2493 = CIRCLE ( 'NONE', #26090, 3.249999999999999112 ) ;
#2494 = CARTESIAN_POINT ( 'NONE',  ( -23.56592830594333421, -19.02588402289573466, 65.97389426991706785 ) ) ;
#2495 = CARTESIAN_POINT ( 'NONE',  ( -12.96547641683174312, -9.412684695659720546, 71.14925319132085235 ) ) ;
#2496 = CARTESIAN_POINT ( 'NONE',  ( -15.88655729437939534, -7.980152340574909076, 67.44007279406643818 ) ) ;
#2497 = EDGE_LOOP ( 'NONE', ( #26654, #9011, #31857, #48087, #29228 ) ) ;
#2498 = CARTESIAN_POINT ( 'NONE',  ( -24.34138212120913991, -16.17068457824029792, 62.74328676669021831 ) ) ;
#2499 = ORIENTED_EDGE ( 'NONE', *, *, #10108, .F. ) ;
#2500 = DIRECTION ( 'NONE',  ( -0.6264825908887947659, 0.7794354131762692983, -3.858680030446929083E-08 ) ) ;
#2501 = CARTESIAN_POINT ( 'NONE',  ( -13.49409790474204840, -20.66256726344224504, 61.53118467422925164 ) ) ;
#2502 = ADVANCED_FACE ( 'NONE', ( #47100 ), #32330, .T. ) ;
#2503 = FACE_OUTER_BOUND ( 'NONE', #26474, .T. ) ;
#2504 = VERTEX_POINT ( 'NONE', #20753 ) ;
#2505 = LINE ( 'NONE', #9900, #9737 ) ;
#2506 = CARTESIAN_POINT ( 'NONE',  ( -10.68551981713787136, -12.73596763222149519, 64.28308208171728211 ) ) ;
#2507 = CARTESIAN_POINT ( 'NONE',  ( -17.42409385541300892, -14.80920654474439502, 77.49999999999994316 ) ) ;
#2508 = EDGE_CURVE ( 'NONE', #47594, #260, #21486, .T. ) ;
#2509 = VECTOR ( 'NONE', #12897, 1000.000000000000000 ) ;
#2510 = CARTESIAN_POINT ( 'NONE',  ( -13.69528297853595511, -8.884503987240256251, 57.25351257252668091 ) ) ;
#2511 = DIRECTION ( 'NONE',  ( -0.000000000000000000, -1.000000000000000000, -0.000000000000000000 ) ) ;
#2512 = CARTESIAN_POINT ( 'NONE',  ( -10.40404453354760683, -17.30384760780096087, 61.27930367573277692 ) ) ;
#2513 = ORIENTED_EDGE ( 'NONE', *, *, #46170, .F. ) ;
#2514 = DIRECTION ( 'NONE',  ( 0.7621627669932625748, -0.6473854467078884456, 3.680865982637999047E-08 ) ) ;
#2515 = CARTESIAN_POINT ( 'NONE',  ( -12.14849447404118088, -10.12808629081546563, 67.91385578414299573 ) ) ;
#2516 = CARTESIAN_POINT ( 'NONE',  ( -22.93575444817954079, -9.796624443348585842, 70.18895421311056282 ) ) ;
#2517 = CARTESIAN_POINT ( 'NONE',  ( -13.72009916595086132, -20.81131062084115513, 61.40157432139535842 ) ) ;
#2518 = DIRECTION ( 'NONE',  ( -0.5351595679979644915, -0.8447509909909737269, 1.882431089060611027E-16 ) ) ;
#2519 = CARTESIAN_POINT ( 'NONE',  ( -12.97364571557156232, -9.395203622806569399, 49.41430056510258595 ) ) ;
#2520 = ORIENTED_EDGE ( 'NONE', *, *, #41580, .T. ) ;
#2521 = ORIENTED_EDGE ( 'NONE', *, *, #26961, .F. ) ;
#2522 = CARTESIAN_POINT ( 'NONE',  ( -22.73241942378198388, -10.24594066210862486, 66.54182232569581856 ) ) ;
#2523 = CYLINDRICAL_SURFACE ( 'NONE', #18704, 0.1500000000000014655 ) ;
#2524 = ORIENTED_EDGE ( 'NONE', *, *, #9769, .F. ) ;
#2525 = CARTESIAN_POINT ( 'NONE',  ( -11.60526899143904345, -18.79015832504765271, 68.23161775275829655 ) ) ;
#2527 = CARTESIAN_POINT ( 'NONE',  ( -45.92409385541293432, 985.6101381041504510, 70.50000000000000000 ) ) ;
#2526 = CARTESIAN_POINT ( 'NONE',  ( -10.11857101092534528, -16.26968670661729632, 71.70396332877544410 ) ) ;
#2528 = CARTESIAN_POINT ( 'NONE',  ( -30.42409385541305156, -25.10920654474410441, 63.99999999999998579 ) ) ;
#2529 = CARTESIAN_POINT ( 'NONE',  ( -11.42622260759249286, -18.51434353338492400, 61.57710833179551457 ) ) ;
#2530 = DIRECTION ( 'NONE',  ( 0.07061531369766044230, 0.9975036227860933913, 1.268851335910971019E-08 ) ) ;
#2531 = ORIENTED_EDGE ( 'NONE', *, *, #20559, .F. ) ;
#2532 = ADVANCED_FACE ( 'NONE', ( #39948 ), #43164, .T. ) ;
#2533 = FACE_BOUND ( 'NONE', #17002, .T. ) ;
#2534 = CARTESIAN_POINT ( 'NONE',  ( -13.43921408130402817, -8.993432070331126127, 60.73950277491898220 ) ) ;
#2535 = EDGE_CURVE ( 'NONE', #4116, #25391, #4552, .T. ) ;
#2536 = DIRECTION ( 'NONE',  ( 0.7248509490090242480, -0.6889057277456162032, 1.880377065355303572E-09 ) ) ;
#2537 = CARTESIAN_POINT ( 'NONE',  ( -23.72463700453396385, -17.86031891732679355, 59.01995031396651825 ) ) ;
#2538 = ADVANCED_FACE ( 'NONE', ( #9194 ), #2523, .T. ) ;
#2539 = ADVANCED_FACE ( 'NONE', ( #35752 ), #17529, .F. ) ;
#2540 = ADVANCED_FACE ( 'NONE', ( #47585 ), #4550, .T. ) ;
#2541 = ORIENTED_EDGE ( 'NONE', *, *, #32856, .F. ) ;
#2542 = PLANE ( 'NONE',  #3893 ) ;
#2543 = CARTESIAN_POINT ( 'NONE',  ( -11.49052871324551717, -18.52330408776863280, 61.27710786653850761 ) ) ;
#2544 = VECTOR ( 'NONE', #20952, 1000.000000000000227 ) ;
#2545 = CARTESIAN_POINT ( 'NONE',  ( -23.00441852451001523, -19.11762575345012749, 58.88410642058937583 ) ) ;
#2546 = CARTESIAN_POINT ( 'NONE',  ( -20.81300959806216966, -21.44393162792159657, 58.82287916276853679 ) ) ;
#2547 =( BOUNDED_CURVE ( )  B_SPLINE_CURVE ( 3, ( #47206, #6806, #6323, #32191 ),
 .UNSPECIFIED., .F., .F. ) 
 B_SPLINE_CURVE_WITH_KNOTS ( ( 4, 4 ),
 ( 1.570796326794896780, 1.780235837034217727 ),
 .UNSPECIFIED. ) 
 CURVE ( )  GEOMETRIC_REPRESENTATION_ITEM ( )  RATIONAL_B_SPLINE_CURVE ( ( 1.000000000000000000, 0.9963479302455154896, 0.9963479302455154896, 1.000000000000000000 ) ) 
 REPRESENTATION_ITEM ( '' )  );
#2548 = CARTESIAN_POINT ( 'NONE',  ( -10.73412800634210029, -11.53077167852495677, 71.20365559628196195 ) ) ;
#2549 = CARTESIAN_POINT ( 'NONE',  ( -12.23220206747518013, -19.57856285391799034, 58.22682373937799838 ) ) ;
#2550 = ORIENTED_EDGE ( 'NONE', *, *, #17972, .T. ) ;
#2551 = ORIENTED_EDGE ( 'NONE', *, *, #34875, .T. ) ;
#2552 = CARTESIAN_POINT ( 'NONE',  ( -19.26159385541304303, -7.228003583438117552, 51.38655588711986155 ) ) ;
#2553 = CARTESIAN_POINT ( 'NONE',  ( -50.42609385541305755, -14.80920654474427600, 73.99411764705880046 ) ) ;
#2554 = CARTESIAN_POINT ( 'NONE',  ( -24.03565964049345283, -17.10859733140495464, 69.60443069367661906 ) ) ;
#2555 =( BOUNDED_CURVE ( )  B_SPLINE_CURVE ( 3, ( #40590, #29775, #28796, #36408 ),
 .UNSPECIFIED., .F., .F. ) 
 B_SPLINE_CURVE_WITH_KNOTS ( ( 4, 4 ),
 ( 0.4074455897393630122, 0.5000000000000000000 ),
 .UNSPECIFIED. ) 
 CURVE ( )  GEOMETRIC_REPRESENTATION_ITEM ( )  RATIONAL_B_SPLINE_CURVE ( ( 0.6983129098260923984, 0.7760317562606954267, 0.8765941196519972944, 0.9999999999999964473 ) ) 
 REPRESENTATION_ITEM ( '' )  );
#2556 = CARTESIAN_POINT ( 'NONE',  ( -15.35027035934970918, -7.653577032698213323, 74.26481056556292515 ) ) ;
#2557 = ADVANCED_FACE ( 'NONE', ( #10156 ), #25178, .T. ) ;
#2558 = CARTESIAN_POINT ( 'NONE',  ( -10.37541943412130863, -14.96049300415475436, 75.08306784598362071 ) ) ;
#2559 = ORIENTED_EDGE ( 'NONE', *, *, #13, .F. ) ;
#2560 = CARTESIAN_POINT ( 'NONE',  ( -19.33163353770262205, -22.01086598974156772, 58.72518590534810556 ) ) ;
#2561 = CARTESIAN_POINT ( 'NONE',  ( -19.23707162763026801, -10.47461692831663882, 52.02966884056656482 ) ) ;
#2562 = ORIENTED_EDGE ( 'NONE', *, *, #47541, .F. ) ;
#2563 = LINE ( 'NONE', #25213, #6871 ) ;
#2564 = CYLINDRICAL_SURFACE ( 'NONE', #33770, 4.686499999999997002 ) ;
#2565 =( BOUNDED_CURVE ( )  B_SPLINE_CURVE ( 3, ( #31181, #42758, #35102, #16866 ),
 .UNSPECIFIED., .F., .F. ) 
 B_SPLINE_CURVE_WITH_KNOTS ( ( 4, 4 ),
 ( 0.5000000000000000000, 0.9074455897393640669 ),
 .UNSPECIFIED. ) 
 CURVE ( )  GEOMETRIC_REPRESENTATION_ITEM ( )  RATIONAL_B_SPLINE_CURVE ( ( 1.000000000000005995, 0.4567392136813334114, 0.3561768502900266586, 0.6983129098260919543 ) ) 
 REPRESENTATION_ITEM ( '' )  );
#2566 = ORIENTED_EDGE ( 'NONE', *, *, #39163, .T. ) ;
#2567 = CARTESIAN_POINT ( 'NONE',  ( -12.72364920584387349, -9.064356868646193277, 49.69365772853683438 ) ) ;
#2568 = CARTESIAN_POINT ( 'NONE',  ( -13.02585106727260822, -13.15662797718154131, 52.02966884056656482 ) ) ;
#2569 = ORIENTED_EDGE ( 'NONE', *, *, #8542, .F. ) ;
#2570 = CARTESIAN_POINT ( 'NONE',  ( -18.59601872632196518, -7.856991649524070809, 73.85536540707786912 ) ) ;
#2571 = CARTESIAN_POINT ( 'NONE',  ( -24.10335570753463230, -17.07466383872621307, 69.29851186845237976 ) ) ;
#2572 = CARTESIAN_POINT ( 'NONE',  ( -16.59344411340201475, -21.75974756046277747, 65.22564390621562325 ) ) ;
#2573 = CARTESIAN_POINT ( 'NONE',  ( -22.53398831605844421, -19.59353892774318595, 72.92935240240784367 ) ) ;
#2574 = VERTEX_POINT ( 'NONE', #37695 ) ;
#2575 = CARTESIAN_POINT ( 'NONE',  ( -15.32518304399999387, -21.95751765168108349, 72.16080051677664642 ) ) ;
#2576 = CARTESIAN_POINT ( 'NONE',  ( -24.06765785688162751, -12.42634649716644013, 69.92810001462744651 ) ) ;
#2577 = CARTESIAN_POINT ( 'NONE',  ( -12.00910550946480093, -19.92697606054074910, 58.04027092519303466 ) ) ;
#2578 = CARTESIAN_POINT ( 'NONE',  ( -17.42409385541299471, -14.80920654474435771, 49.52966884056655772 ) ) ;
#2579 = CARTESIAN_POINT ( 'NONE',  ( -21.84909385650551528, -8.104110260919577868, 48.81699501597546487 ) ) ;
#2580 = CARTESIAN_POINT ( 'NONE',  ( -16.78341102624552050, -22.23169286577646986, 68.88055947109249644 ) ) ;
#2581 = CARTESIAN_POINT ( 'NONE',  ( -23.54659830298692569, -19.05403935986104003, 66.08035378328281695 ) ) ;
#2582 = ORIENTED_EDGE ( 'NONE', *, *, #34712, .T. ) ;
#2583 = CARTESIAN_POINT ( 'NONE',  ( -23.58068229492725720, -11.36663999465536179, 73.66193538997137580 ) ) ;
#2584 = CYLINDRICAL_SURFACE ( 'NONE', #9338, 1.000000000000000888 ) ;
#2585 = CARTESIAN_POINT ( 'NONE',  ( -10.00543091975737831, -15.49190080042082940, 57.76781588145245649 ) ) ;
#2586 = VERTEX_POINT ( 'NONE', #18000 ) ;
#2587 = CARTESIAN_POINT ( 'NONE',  ( -19.78614083979442029, -21.39864764726399216, 69.23482476778590922 ) ) ;
#2588 = B_SPLINE_CURVE_WITH_KNOTS ( 'NONE', 3,
 ( #3821, #34572, #15856, #12176, #33841, #42218, #1092, #8482, #4795, #34818 ),
 .UNSPECIFIED., .F., .F.,
 ( 4, 2, 2, 2, 4 ),
 ( 0.000000000000000000, 0.2500000000000000000, 0.5000000000000000000, 0.7500000000000000000, 1.000000000000000000 ),
 .UNSPECIFIED. ) ;
#2589 = ORIENTED_EDGE ( 'NONE', *, *, #27980, .T. ) ;
#2590 = EDGE_CURVE ( 'NONE', #42959, #3873, #28148, .T. ) ;
#2591 = EDGE_CURVE ( 'NONE', #45017, #39895, #35194, .T. ) ;
#2592 = ORIENTED_EDGE ( 'NONE', *, *, #16262, .T. ) ;
#2593 = ORIENTED_EDGE ( 'NONE', *, *, #18017, .F. ) ;
#2594 = VECTOR ( 'NONE', #6001, 1000.000000000000000 ) ;
#2595 = CARTESIAN_POINT ( 'NONE',  ( -21.34581862946232889, -20.66775363590295100, 72.52446429492309221 ) ) ;
#2596 = DIRECTION ( 'NONE',  ( -3.298726454030011118E-06, 1.683524824177191357E-06, 0.9999999999931419303 ) ) ;
#2597 = PLANE ( 'NONE',  #44083 ) ;
#2598 = ORIENTED_EDGE ( 'NONE', *, *, #24802, .F. ) ;
#2599 = EDGE_LOOP ( 'NONE', ( #20684, #13603, #13294, #28141 ) ) ;
#2600 = EDGE_CURVE ( 'NONE', #28218, #43409, #29728, .T. ) ;
#2601 = EDGE_CURVE ( 'NONE', #5056, #18999, #47288, .T. ) ;
#2602 = CARTESIAN_POINT ( 'NONE',  ( -18.39284385650552167, -7.406986770994973490, 48.81910596585309747 ) ) ;
#2603 = CARTESIAN_POINT ( 'NONE',  ( -14.81535805098777736, -7.777528402031247623, 53.89198173725363716 ) ) ;
#2604 = CARTESIAN_POINT ( 'NONE',  ( -10.82849721076305194, -17.15437656679925738, 61.45743105333846756 ) ) ;
#2605 = CARTESIAN_POINT ( 'NONE',  ( -17.32409385650551314, -6.426201560718813433, 50.50509628382439331 ) ) ;
#2606 = ORIENTED_EDGE ( 'NONE', *, *, #47427, .F. ) ;
#2607 = EDGE_CURVE ( 'NONE', #17100, #6762, #1382, .T. ) ;
#2608 = DIRECTION ( 'NONE',  ( -3.549360974554993999E-17, 6.371834667797928663E-18, 1.000000000000000000 ) ) ;
#2609 = DIRECTION ( 'NONE',  ( -3.071710424422018668E-17, 6.404604876783312462E-16, 1.000000000000000000 ) ) ;
#2610 = EDGE_LOOP ( 'NONE', ( #24201, #43210, #17542, #32687 ) ) ;
#2611 = LINE ( 'NONE', #29437, #43798 ) ;
#2612 = VERTEX_POINT ( 'NONE', #3242 ) ;
#2613 = DIRECTION ( 'NONE',  ( 1.224646799147353207E-16, 1.000000000000000000, -1.912410701131276611E-32 ) ) ;
#2614 = FACE_OUTER_BOUND ( 'NONE', #17833, .T. ) ;
#2615 = CARTESIAN_POINT ( 'NONE',  ( -19.03885666732217885, -7.536228653801991584, 67.15717731432056326 ) ) ;
#2616 = CIRCLE ( 'NONE', #42741, 0.5000000000000004441 ) ;
#2617 = VERTEX_POINT ( 'NONE', #29348 ) ;
#2618 = CARTESIAN_POINT ( 'NONE',  ( -18.97948276208418150, -7.924750873940990203, 60.11659987143988815 ) ) ;
#2619 = CARTESIAN_POINT ( 'NONE',  ( -11.36942910905634108, -11.19057675027386800, 64.24062247360485856 ) ) ;
#2620 = CYLINDRICAL_SURFACE ( 'NONE', #45748, 0.1500000000000020206 ) ;
#2621 = ORIENTED_EDGE ( 'NONE', *, *, #27337, .F. ) ;
#2622 = CARTESIAN_POINT ( 'NONE',  ( -20.71200339104809274, -20.98905351909935035, 58.93009817979976361 ) ) ;
#2623 = CARTESIAN_POINT ( 'NONE',  ( -24.84793648988037518, -14.18443574041886457, 69.83770584630335065 ) ) ;
#2624 = ORIENTED_EDGE ( 'NONE', *, *, #12755, .F. ) ;
#2625 = CARTESIAN_POINT ( 'NONE',  ( -10.64512080333459387, -11.71903002653516168, 74.81486074884371362 ) ) ;
#2626 = ORIENTED_EDGE ( 'NONE', *, *, #13686, .F. ) ;
#2627 = CARTESIAN_POINT ( 'NONE',  ( -17.42409385541299471, -14.80920654474435594, 52.02966884056656482 ) ) ;
#2628 = CARTESIAN_POINT ( 'NONE',  ( -13.71293330176565384, -21.26916511146244915, 68.64120417180296840 ) ) ;
#2629 = FACE_OUTER_BOUND ( 'NONE', #5332, .T. ) ;
#2630 = CARTESIAN_POINT ( 'NONE',  ( -22.73035995389123798, -10.24127042357611650, 70.20105554212841525 ) ) ;
#2631 = VERTEX_POINT ( 'NONE', #22447 ) ;
#2632 = CARTESIAN_POINT ( 'NONE',  ( -21.95939004544374740, -9.477125498926222136, 59.72171213236985921 ) ) ;
#2633 = CARTESIAN_POINT ( 'NONE',  ( -18.97054302448013985, -7.521389842619064403, 67.08567168106696954 ) ) ;
#2634 = CARTESIAN_POINT ( 'NONE',  ( -21.54712039243748833, -8.603915288790302540, 73.73982196406554124 ) ) ;
#2635 = B_SPLINE_CURVE_WITH_KNOTS ( 'NONE', 3,
 ( #33569, #47894, #40492, #37772, #25720, #40735, #11430, #128, #37028, #48615 ),
 .UNSPECIFIED., .F., .F.,
 ( 4, 2, 2, 2, 4 ),
 ( 0.000000000000000000, 0.2500000000000000000, 0.5000000000000000000, 0.7500000000000000000, 1.000000000000000000 ),
 .UNSPECIFIED. ) ;
#2636 = VERTEX_POINT ( 'NONE', #48 ) ;
#2637 = CARTESIAN_POINT ( 'NONE',  ( -9.976559278833523337, -14.59036342035520306, 67.97144843379662404 ) ) ;
#2638 = CARTESIAN_POINT ( 'NONE',  ( -22.58237342315448615, -13.83214364962418230, 49.52966884056655772 ) ) ;
#2639 = B_SPLINE_CURVE_WITH_KNOTS ( 'NONE', 3,
 ( #44834, #11087, #22659, #18700, #26109, #37657, #3949, #18961, #1451, #24115 ),
 .UNSPECIFIED., .F., .F.,
 ( 4, 2, 2, 2, 4 ),
 ( 0.1272669073657988204, 0.2522669073462828204, 0.3772669073267668205, 0.5022669073072507651, 0.6272669072877348206 ),
 .UNSPECIFIED. ) ;
#2640 = EDGE_CURVE ( 'NONE', #7134, #16837, #13761, .T. ) ;
#2641 = VERTEX_POINT ( 'NONE', #25896 ) ;
#2642 = ORIENTED_EDGE ( 'NONE', *, *, #41119, .F. ) ;
#2643 = CARTESIAN_POINT ( 'NONE',  ( -18.35035633668588773, -22.20141378626043860, 68.91540458395735413 ) ) ;
#2644 = FACE_OUTER_BOUND ( 'NONE', #29928, .T. ) ;
#2645 = DIRECTION ( 'NONE',  ( -1.000000000000000000, 0.000000000000000000, 0.000000000000000000 ) ) ;
#2646 = CARTESIAN_POINT ( 'NONE',  ( -10.45378225047720200, -13.70027870591744446, 74.83384660681542755 ) ) ;
#2647 = CARTESIAN_POINT ( 'NONE',  ( -19.45739170982025357, -7.641871707264925817, 60.12239523375242101 ) ) ;
#2648 = CARTESIAN_POINT ( 'NONE',  ( -12.40380833417894912, -19.68739609921301792, 61.39678633575574906 ) ) ;
#2649 = CARTESIAN_POINT ( 'NONE',  ( -12.60227155074094441, -19.95281705956671559, 68.35129494334645983 ) ) ;
#2650 = CARTESIAN_POINT ( 'NONE',  ( -20.63628304827270199, -8.086446354347476273, 66.96759359044023086 ) ) ;
#2651 = ORIENTED_EDGE ( 'NONE', *, *, #6993, .F. ) ;
#2652 = ORIENTED_EDGE ( 'NONE', *, *, #4389, .F. ) ;
#2653 = EDGE_CURVE ( 'NONE', #7442, #5861, #37310, .T. ) ;
#2654 = CARTESIAN_POINT ( 'NONE',  ( -13.25048244539004827, -9.122748337194952484, 60.43949979652826698 ) ) ;
#2655 = AXIS2_PLACEMENT_3D ( 'NONE', #29899, #15091, #3297 ) ;
#2656 = EDGE_CURVE ( 'NONE', #32569, #18851, #21802, .T. ) ;
#2657 = FACE_OUTER_BOUND ( 'NONE', #4683, .T. ) ;
#2658 = CARTESIAN_POINT ( 'NONE',  ( -10.57990114081760957, -13.11695186304740979, 71.22300718686658172 ) ) ;
#2659 = CARTESIAN_POINT ( 'NONE',  ( -18.97893323490226791, -7.523212336634692576, 67.00733453731432121 ) ) ;
#2660 = CYLINDRICAL_SURFACE ( 'NONE', #30778, 0.1500000000000035194 ) ;
#2661 = EDGE_CURVE ( 'NONE', #8589, #29913, #45118, .T. ) ;
#2662 = CARTESIAN_POINT ( 'NONE',  ( -20.04909385650551457, -8.104110260919579645, 48.81699501597546487 ) ) ;
#2663 = VERTEX_POINT ( 'NONE', #14053 ) ;
#2664 = CARTESIAN_POINT ( 'NONE',  ( -16.60428136649079534, -9.623610389719635450, 52.02966884056656482 ) ) ;
#2665 = CARTESIAN_POINT ( 'NONE',  ( -10.22367903246940557, -12.89696208012659717, 67.83808713863969331 ) ) ;
#2666 = DIRECTION ( 'NONE',  ( -3.071710424422018668E-17, 6.404604876783312462E-16, 1.000000000000000000 ) ) ;
#2667 = FACE_OUTER_BOUND ( 'NONE', #21033, .T. ) ;
#2668 = EDGE_LOOP ( 'NONE', ( #41272, #36699, #13492, #43121 ) ) ;
#2669 = CARTESIAN_POINT ( 'NONE',  ( -10.57458986182457750, -16.25351003539013561, 71.74750329799698534 ) ) ;
#2670 = CARTESIAN_POINT ( 'NONE',  ( -17.91716493482169525, -7.374790294242734134, 60.26716059546817661 ) ) ;
#2671 = CARTESIAN_POINT ( 'NONE',  ( -26.42409385541305511, -25.10920654474410441, 48.99999999999997868 ) ) ;
#2672 =( BOUNDED_CURVE ( )  B_SPLINE_CURVE ( 3, ( #18114, #32892, #15152, #7554 ),
 .UNSPECIFIED., .F., .F. ) 
 B_SPLINE_CURVE_WITH_KNOTS ( ( 4, 4 ),
 ( 0.9074455897393624015, 1.000000000000000000 ),
 .UNSPECIFIED. ) 
 CURVE ( )  GEOMETRIC_REPRESENTATION_ITEM ( )  RATIONAL_B_SPLINE_CURVE ( ( 0.6983129098260865142, 0.7760317562606925401, 0.8765941196519970724, 1.000000000000000000 ) ) 
 REPRESENTATION_ITEM ( '' )  );
#2673 = ORIENTED_EDGE ( 'NONE', *, *, #27858, .F. ) ;
#2674 = CARTESIAN_POINT ( 'NONE',  ( -20.98580030992770418, -20.83533690608478040, 65.88453944791919525 ) ) ;
#2675 = ORIENTED_EDGE ( 'NONE', *, *, #43911, .T. ) ;
#2676 = VECTOR ( 'NONE', #40730, 1000.000000000000000 ) ;
#2677 = LINE ( 'NONE', #25574, #27360 ) ;
#2678 = CARTESIAN_POINT ( 'NONE',  ( -10.00972249263052838, -14.08138219831849014, 61.11810067724670148 ) ) ;
#2679 = ORIENTED_EDGE ( 'NONE', *, *, #33077, .T. ) ;
#2680 = CARTESIAN_POINT ( 'NONE',  ( -15.80316865820435446, -9.815700611529285524, 50.77966884056655772 ) ) ;
#2681 = CIRCLE ( 'NONE', #6599, 4.686499999999999666 ) ;
#2682 = CARTESIAN_POINT ( 'NONE',  ( -14.62409385650551386, -6.426201560718813433, 50.50509628382439331 ) ) ;
#2683 = VERTEX_POINT ( 'NONE', #10406 ) ;
#2684 = CARTESIAN_POINT ( 'NONE',  ( -18.84909840123831160, -7.954480093619391567, 70.59898004676588812 ) ) ;
#2685 = EDGE_CURVE ( 'NONE', #32730, #38697, #8034, .T. ) ;
#2686 = DIRECTION ( 'NONE',  ( -3.071710424422018668E-17, 6.404604876783312462E-16, 1.000000000000000000 ) ) ;
#2687 = CARTESIAN_POINT ( 'NONE',  ( -20.95545100651803594, -20.91135505560678354, 65.59926067308570907 ) ) ;
#2688 = ORIENTED_EDGE ( 'NONE', *, *, #29882, .T. ) ;
#2689 = CARTESIAN_POINT ( 'NONE',  ( -19.94877900550811844, -21.81838596911105554, 69.13471258482660176 ) ) ;
#2690 =( BOUNDED_CURVE ( )  B_SPLINE_CURVE ( 3, ( #21308, #28682, #2583, #17586 ),
 .UNSPECIFIED., .F., .F. ) 
 B_SPLINE_CURVE_WITH_KNOTS ( ( 4, 4 ),
 ( 0.5000000000000000000, 0.9074455897393649551 ),
 .UNSPECIFIED. ) 
 CURVE ( )  GEOMETRIC_REPRESENTATION_ITEM ( )  RATIONAL_B_SPLINE_CURVE ( ( 1.000000000000019540, 0.4567392136813264170, 0.3561768502900144462, 0.6983129098261048329 ) ) 
 REPRESENTATION_ITEM ( '' )  );
#2691 = CARTESIAN_POINT ( 'NONE',  ( -10.95687064503993824, -18.50777464695341479, 57.92997716917032136 ) ) ;
#2692 = CARTESIAN_POINT ( 'NONE',  ( -23.29452124531334434, -19.39641313704064629, 59.00693762799269848 ) ) ;
#2693 = CYLINDRICAL_SURFACE ( 'NONE', #31866, 0.1500000000000002720 ) ;
#2694 = ORIENTED_EDGE ( 'NONE', *, *, #16466, .T. ) ;
#2695 = VERTEX_POINT ( 'NONE', #25415 ) ;
#2696 = CARTESIAN_POINT ( 'NONE',  ( -22.54039128431939787, -19.66481624898402458, 69.38238023638768937 ) ) ;
#2697 = CARTESIAN_POINT ( 'NONE',  ( -24.69852180232685157, -16.41745880042978101, 59.30827708941524889 ) ) ;
#2698 = EDGE_LOOP ( 'NONE', ( #2462, #46521, #11217, #2598, #14273 ) ) ;
#2699 = CARTESIAN_POINT ( 'NONE',  ( -23.80321479583337307, -17.81075880182941873, 59.30378417737343710 ) ) ;
#2700 = CARTESIAN_POINT ( 'NONE',  ( -17.88659385759798681, -7.222650657624104298, 49.61879703869476543 ) ) ;
#2701 = CARTESIAN_POINT ( 'NONE',  ( -15.55326400670571196, -7.597850160029695488, 70.65343888371961611 ) ) ;
#2702 = ORIENTED_EDGE ( 'NONE', *, *, #30237, .T. ) ;
#2703 = CARTESIAN_POINT ( 'NONE',  ( -10.54203096409779050, -13.52967128519119200, 74.86920801952661009 ) ) ;
#2704 = B_SPLINE_CURVE_WITH_KNOTS ( 'NONE', 3,
 ( #26937, #41955, #41711, #23015, #8231, #16067, #1550, #4287, #23246, #38734 ),
 .UNSPECIFIED., .F., .F.,
 ( 4, 2, 2, 2, 4 ),
 ( 0.1272669073658395933, 0.2522669073439455234, 0.3772669073220514813, 0.5022669073001573281, 0.6272669072782632860 ),
 .UNSPECIFIED. ) ;
#2705 = EDGE_CURVE ( 'NONE', #6966, #37287, #34488, .T. ) ;
#2706 = CARTESIAN_POINT ( 'NONE',  ( -18.92057809895272413, -7.919864474132485732, 66.90071783790344284 ) ) ;
#2707 = CARTESIAN_POINT ( 'NONE',  ( -13.57571756020798581, -20.65642803140422856, 61.51646323935151628 ) ) ;
#2708 = EDGE_CURVE ( 'NONE', #1365, #25, #30583, .T. ) ;
#2709 = EDGE_LOOP ( 'NONE', ( #11574, #17305 ) ) ;
#2710 = AXIS2_PLACEMENT_3D ( 'NONE', #4888, #1170, #37618 ) ;
#2711 = ADVANCED_FACE ( 'NONE', ( #7936 ), #8654, .T. ) ;
#2712 = ORIENTED_EDGE ( 'NONE', *, *, #10175, .T. ) ;
#2713 = FACE_OUTER_BOUND ( 'NONE', #32187, .T. ) ;
#2714 = PRESENTATION_STYLE_ASSIGNMENT (( #28354 ) ) ;
#2715 = CARTESIAN_POINT ( 'NONE',  ( -10.00816431203761780, -14.09700820520310671, 61.02482976538944826 ) ) ;
#2716 = CARTESIAN_POINT ( 'NONE',  ( -15.26784385541301425, -9.357632978295642445, 49.97845033065664921 ) ) ;
#2717 = EDGE_CURVE ( 'NONE', #5348, #47871, #23400, .T. ) ;
#2718 = ORIENTED_EDGE ( 'NONE', *, *, #25374, .F. ) ;
#2719 = CARTESIAN_POINT ( 'NONE',  ( -24.23275881451340297, -13.18375842335132830, 59.47153824729769411 ) ) ;
#2720 = CYLINDRICAL_SURFACE ( 'NONE', #46137, 0.1500000000000029365 ) ;
#2721 = ORIENTED_EDGE ( 'NONE', *, *, #3390, .T. ) ;
#2722 = DIRECTION ( 'NONE',  ( 0.000000000000000000, 0.000000000000000000, -1.000000000000000000 ) ) ;
#2723 = CARTESIAN_POINT ( 'NONE',  ( -12.57255317706665387, -20.46319310760117816, 71.96687053577548454 ) ) ;
#2724 = DIRECTION ( 'NONE',  ( 0.3374354101627465297, 0.9413486835218388693, 1.423378189492272923E-08 ) ) ;
#2725 = ORIENTED_EDGE ( 'NONE', *, *, #22932, .F. ) ;
#2726 = CARTESIAN_POINT ( 'NONE',  ( -14.62409385759799108, -9.359200813967568422, 50.49621490985803263 ) ) ;
#2727 = EDGE_LOOP ( 'NONE', ( #16534, #10363, #44094, #48223 ) ) ;
#2728 = DIRECTION ( 'NONE',  ( -0.2196488028684550620, -0.9755790093059855117, 7.835600157697873389E-08 ) ) ;
#2729 = CARTESIAN_POINT ( 'NONE',  ( -22.74914502862361587, -19.44157078561079999, 72.79967855327656423 ) ) ;
#2730 = CARTESIAN_POINT ( 'NONE',  ( -19.37066084507306130, -21.53310995536324413, 58.71610482352626548 ) ) ;
#2731 = ORIENTED_EDGE ( 'NONE', *, *, #14015, .F. ) ;
#2732 = CARTESIAN_POINT ( 'NONE',  ( -21.43551424305475450, -21.08722505841212680, 69.21483509587649507 ) ) ;
#2733 = CARTESIAN_POINT ( 'NONE',  ( -10.60833884242739522, -12.99528357717770355, 64.15347367985145866 ) ) ;
#2734 = DIRECTION ( 'NONE',  ( -0.06357898915124167438, 0.9979768094191900918, 0.000000000000000000 ) ) ;
#2735 = B_SPLINE_CURVE_WITH_KNOTS ( 'NONE', 1,
 ( #17329, #21763 ),
 .UNSPECIFIED., .F., .F.,
 ( 2, 2 ),
 ( 0.000000000000000000, 1.000000000000000000 ),
 .UNSPECIFIED. ) ;
#2736 = EDGE_CURVE ( 'NONE', #5301, #18974, #20280, .T. ) ;
#2737 = DIRECTION ( 'NONE',  ( -3.071710424422018668E-17, 6.404604876783312462E-16, 1.000000000000000000 ) ) ;
#2738 = CARTESIAN_POINT ( 'NONE',  ( -13.89284385759799356, -8.630756214087126565, 51.74842643355248129 ) ) ;
#2739 = CARTESIAN_POINT ( 'NONE',  ( -17.03658212107600534, -14.90837637761270251, 52.02966884056656482 ) ) ;
#2740 = ORIENTED_EDGE ( 'NONE', *, *, #6979, .F. ) ;
#2741 = DIRECTION ( 'NONE',  ( -0.3478314405900309603, -0.9375570856950864451, 9.567072274253696421E-17 ) ) ;
#2742 = DIRECTION ( 'NONE',  ( -0.9979768094191906469, -0.06357898915123129380, 0.000000000000000000 ) ) ;
#2743 = VECTOR ( 'NONE', #5325, 1000.000000000000000 ) ;
#2744 = DIRECTION ( 'NONE',  ( -2.866981220435666553E-17, 1.000000000000000000, 1.190614954331866791E-16 ) ) ;
#2745 = CARTESIAN_POINT ( 'NONE',  ( -10.99586697244644640, -11.04334986774487781, 60.86381167495338929 ) ) ;
#2746 = CARTESIAN_POINT ( 'NONE',  ( -24.76540221579651302, -16.07765826482591365, 66.17829537637275905 ) ) ;
#2747 = AXIS2_PLACEMENT_3D ( 'NONE', #9139, #5447, #2217 ) ;
#2748 = VERTEX_POINT ( 'NONE', #27598 ) ;
#2749 = ORIENTED_EDGE ( 'NONE', *, *, #45902, .F. ) ;
#2750 = CARTESIAN_POINT ( 'NONE',  ( -21.24554520941113367, -21.20453976546471608, 65.76949229983627276 ) ) ;
#2751 = DIRECTION ( 'NONE',  ( -0.8356905716187448263, 0.5492005722024784209, 7.728900804118606451E-08 ) ) ;
#2752 = VERTEX_POINT ( 'NONE', #775 ) ;
#2754 = CARTESIAN_POINT ( 'NONE',  ( -13.38659385650551847, -9.302874398569244363, 51.68646062012417985 ) ) ;
#2753 = CARTESIAN_POINT ( 'NONE',  ( -11.64235137327199610, -18.84330536064715034, 68.36689631560025759 ) ) ;
#2755 = CARTESIAN_POINT ( 'NONE',  ( -11.32868513771122743, -18.25189784781867530, 58.09098068066235498 ) ) ;
#2756 = CARTESIAN_POINT ( 'NONE',  ( -11.82099749022622426, -9.899105802180386604, 64.21409645106085406 ) ) ;
#2757 = CARTESIAN_POINT ( 'NONE',  ( -24.74075724160099554, -16.21284971877490122, 62.77824058731629009 ) ) ;
#2758 = FACE_OUTER_BOUND ( 'NONE', #35585, .T. ) ;
#2759 = FACE_BOUND ( 'NONE', #17471, .T. ) ;
#2760 = EDGE_CURVE ( 'NONE', #23333, #37436, #4711, .T. ) ;
#2761 = CARTESIAN_POINT ( 'NONE',  ( -23.89968659910968185, -17.46782286739716028, 65.94357233134253704 ) ) ;
#2762 = CARTESIAN_POINT ( 'NONE',  ( -23.19916440516392697, -19.59445054535707698, 54.27966884056655061 ) ) ;
#2763 = CYLINDRICAL_SURFACE ( 'NONE', #13360, 0.1500000000000011879 ) ;
#2764 = VERTEX_POINT ( 'NONE', #34972 ) ;
#2765 = FACE_OUTER_BOUND ( 'NONE', #22404, .T. ) ;
#2766 = LINE ( 'NONE', #41410, #46308 ) ;
#2767 = B_SPLINE_CURVE_WITH_KNOTS ( 'NONE', 3,
 ( #19081, #4318, #26472, #33102, #44969, #7037, #7778, #15128, #26229, #30428 ),
 .UNSPECIFIED., .F., .F.,
 ( 4, 2, 2, 2, 4 ),
 ( 0.000000000000000000, 0.2500000000000000000, 0.5000000000000000000, 0.7500000000000000000, 1.000000000000000000 ),
 .UNSPECIFIED. ) ;
#2768 = SHAPE_REPRESENTATION ( 'MAS-175', ( #14072, #20408, #3890, #6240, #5428, #41624, #10179, #43184, #48689, #2293 ), #25866 ) ;
#2769 = DIRECTION ( 'NONE',  ( 3.413470714839332458E-33, -1.190614954331866791E-16, 1.000000000000000000 ) ) ;
#2770 = CARTESIAN_POINT ( 'NONE',  ( -24.18648589646226910, -17.93571655855329894, 59.16411793359512217 ) ) ;
#2771 = CARTESIAN_POINT ( 'NONE',  ( -24.03385203260749847, -12.34657780677343375, 73.45045475050159212 ) ) ;
#2772 = CARTESIAN_POINT ( 'NONE',  ( -24.87123160714014958, -14.59964084223042491, 62.89791924484052998 ) ) ;
#2773 = ORIENTED_EDGE ( 'NONE', *, *, #23450, .T. ) ;
#2774 = ORIENTED_EDGE ( 'NONE', *, *, #14832, .F. ) ;
#2775 = CARTESIAN_POINT ( 'NONE',  ( -16.73034385541304303, -6.857644439848013640, 49.98602051094139398 ) ) ;
#2776 = EDGE_CURVE ( 'NONE', #26191, #18567, #4861, .T. ) ;
#2777 = ORIENTED_EDGE ( 'NONE', *, *, #12545, .T. ) ;
#2778 = CARTESIAN_POINT ( 'NONE',  ( -13.18646824325598566, -9.237624247784513187, 64.10049605889102509 ) ) ;
#2779 = FACE_OUTER_BOUND ( 'NONE', #6573, .T. ) ;
#2780 = ADVANCED_FACE ( 'NONE', ( #1015 ), #9606, .T. ) ;
#2781 = B_SPLINE_CURVE_WITH_KNOTS ( 'NONE', 3,
 ( #29394, #11171, #14100, #36286, #3035, #10451, #48587, #28905, #36747, #29150 ),
 .UNSPECIFIED., .F., .F.,
 ( 4, 2, 2, 2, 4 ),
 ( 0.1272669073657631822, 0.2522669073462648903, 0.3772669073267665429, 0.5022669073072681956, 0.6272669072877699037 ),
 .UNSPECIFIED. ) ;
#2782 = DIRECTION ( 'NONE',  ( -5.731567514496413899E-31, -1.020425574103664789E-16, -1.000000000000000000 ) ) ;
#2783 = LINE ( 'NONE', #7477, #19926 ) ;
#2784 = EDGE_LOOP ( 'NONE', ( #33088, #44144, #32827, #44767 ) ) ;
#2785 = DIRECTION ( 'NONE',  ( -1.000000000000000000, 0.000000000000000000, -0.000000000000000000 ) ) ;
#2786 = DIRECTION ( 'NONE',  ( -5.551115123125782702E-17, -1.232595164407830946E-32, -1.000000000000000000 ) ) ;
#2787 = VERTEX_POINT ( 'NONE', #27108 ) ;
#2788 = LINE ( 'NONE', #32118, #47745 ) ;
#2789 = EDGE_CURVE ( 'NONE', #46311, #784, #47891, .T. ) ;
#2790 = CARTESIAN_POINT ( 'NONE',  ( -13.18904211892903078, -11.30002761096173813, 53.49999999999995026 ) ) ;
#2791 = EDGE_CURVE ( 'NONE', #29130, #43276, #45840, .T. ) ;
#2792 = ORIENTED_EDGE ( 'NONE', *, *, #42325, .F. ) ;
#2793 = DIRECTION ( 'NONE',  ( 6.374839753205896285E-22, 0.007114381193220324640, -0.9999746924698832418 ) ) ;
#2794 = DIRECTION ( 'NONE',  ( -3.071710424422018668E-17, 6.404604876783312462E-16, 1.000000000000000000 ) ) ;
#2795 = CARTESIAN_POINT ( 'NONE',  ( -9.979271025556270658, -14.52814615614862070, 68.03517031705335683 ) ) ;
#2796 = EDGE_CURVE ( 'NONE', #31355, #46961, #19730, .T. ) ;
#2798 = ADVANCED_FACE ( 'NONE', ( #47291 ), #16736, .T. ) ;
#2797 = ORIENTED_EDGE ( 'NONE', *, *, #11598, .T. ) ;
#2799 = DIRECTION ( 'NONE',  ( -3.071710424422018668E-17, 6.404604876783312462E-16, 1.000000000000000000 ) ) ;
#2800 = CARTESIAN_POINT ( 'NONE',  ( -23.38668381416880138, -18.47650297087272975, 73.06368285098588444 ) ) ;
#2801 = DIRECTION ( 'NONE',  ( 1.000000000000000000, 0.000000000000000000, 0.000000000000000000 ) ) ;
#2802 = CARTESIAN_POINT ( 'NONE',  ( -23.94296205860991122, -17.35973477539799603, 65.95859725740298529 ) ) ;
#2803 = ORIENTED_EDGE ( 'NONE', *, *, #48449, .F. ) ;
#2804 = CYLINDRICAL_SURFACE ( 'NONE', #21896, 1.249999999999999334 ) ;
#2805 = FACE_OUTER_BOUND ( 'NONE', #13035, .T. ) ;
#2806 = CARTESIAN_POINT ( 'NONE',  ( -15.51710240044429590, -8.021979398744527145, 74.07985680213998592 ) ) ;
#2807 = CARTESIAN_POINT ( 'NONE',  ( -14.42683416945219221, -8.428067588089273698, 67.40975083869261653 ) ) ;
#2808 = FACE_OUTER_BOUND ( 'NONE', #43285, .T. ) ;
#2809 = CARTESIAN_POINT ( 'NONE',  ( -17.42409385541299471, -14.80920654474434883, 62.02966884056656482 ) ) ;
#2810 = VERTEX_POINT ( 'NONE', #1975 ) ;
#2811 = CARTESIAN_POINT ( 'NONE',  ( -24.31823732957325745, -17.63313362019280106, 66.05861802595141796 ) ) ;
#2812 = CARTESIAN_POINT ( 'NONE',  ( -13.22252872046149541, -18.37919617513480475, 53.88362224778187226 ) ) ;
#2813 = CYLINDRICAL_SURFACE ( 'NONE', #42338, 1.249999999999999334 ) ;
#2814 =( BOUNDED_SURFACE ( )  B_SPLINE_SURFACE ( 3, 1, ( 
 ( #3506, #34515 ),
 ( #15547, #41918 ),
 ( #12119, #26176 ),
 ( #18518, #34029 ),
 ( #798, #27135 ),
 ( #15795, #22979 ),
 ( #8198, #42162 ) ),
 .UNSPECIFIED., .T., .F., .F. ) 
 B_SPLINE_SURFACE_WITH_KNOTS ( ( 4, 3, 4 ),
 ( 2, 2 ),
 ( 0.000000000000000000, 0.5000000000000000000, 1.000000000000000000 ),
 ( 0.000000000000000000, 1.000000000000000000 ),
 .UNSPECIFIED. ) 
 GEOMETRIC_REPRESENTATION_ITEM ( )  RATIONAL_B_SPLINE_SURFACE ( (
 ( 1.000000000000000000, 1.000000000000000000),
 ( 0.3333333333333335369, 0.3333333333333330373),
 ( 0.3333333333333335369, 0.3333333333333330373),
 ( 1.000000000000000000, 1.000000000000000000),
 ( 0.3333333333333333703, 0.3333333333333333703),
 ( 0.3333333333333333703, 0.3333333333333333703),
 ( 1.000000000000000000, 1.000000000000000000) ) ) 
 REPRESENTATION_ITEM ( '' )  SURFACE ( )  );
#2815 = ORIENTED_EDGE ( 'NONE', *, *, #13611, .T. ) ;
#2816 = CARTESIAN_POINT ( 'NONE',  ( -10.04615901573667003, -15.84412989934948257, 64.66918126557563085 ) ) ;
#2817 = AXIS2_PLACEMENT_3D ( 'NONE', #28652, #42942, #35546 ) ;
#2818 = EDGE_LOOP ( 'NONE', ( #13739, #45229, #28599, #41545, #46357 ) ) ;
#2819 = ORIENTED_EDGE ( 'NONE', *, *, #8829, .T. ) ;
#2820 = ORIENTED_EDGE ( 'NONE', *, *, #43969, .T. ) ;
#2821 = CYLINDRICAL_SURFACE ( 'NONE', #6860, 6.899999999999999467 ) ;
#2822 = DIRECTION ( 'NONE',  ( 1.235321093103353499E-06, 4.801898924785047334E-07, 0.9999999999991215915 ) ) ;
#2823 = LINE ( 'NONE', #29420, #2361 ) ;
#2824 = CARTESIAN_POINT ( 'NONE',  ( -22.65132463393941364, -10.07854832284319890, 70.31178513642615258 ) ) ;
#2825 =( BOUNDED_CURVE ( )  B_SPLINE_CURVE ( 3, ( #23416, #15507, #41387, #34232 ),
 .UNSPECIFIED., .F., .F. ) 
 B_SPLINE_CURVE_WITH_KNOTS ( ( 4, 4 ),
 ( 0.4074455897393645110, 0.5000000000000000000 ),
 .UNSPECIFIED. ) 
 CURVE ( )  GEOMETRIC_REPRESENTATION_ITEM ( )  RATIONAL_B_SPLINE_CURVE ( ( 0.6983129098261006140, 0.7760317562606882102, 0.8765941196519829726, 0.9999999999999736877 ) ) 
 REPRESENTATION_ITEM ( '' )  );
#2826 = ORIENTED_EDGE ( 'NONE', *, *, #17243, .F. ) ;
#2827 = VERTEX_POINT ( 'NONE', #5917 ) ;
#2828 = CARTESIAN_POINT ( 'NONE',  ( -18.56159385650551741, -9.295667164867525756, 49.30633214617472504 ) ) ;
#2829 = EDGE_CURVE ( 'NONE', #7981, #22280, #35037, .T. ) ;
#2830 = FACE_OUTER_BOUND ( 'NONE', #323, .T. ) ;
#2831 = LINE ( 'NONE', #7283, #21418 ) ;
#2832 = CARTESIAN_POINT ( 'NONE',  ( -18.61784385650552309, -9.790100578890868377, 49.79778022625163203 ) ) ;
#2833 =( BOUNDED_SURFACE ( )  B_SPLINE_SURFACE ( 3, 1, ( 
 ( #4361, #8306 ),
 ( #41799, #19136 ),
 ( #30722, #45749 ),
 ( #12232, #30483 ),
 ( #27252, #11999 ),
 ( #42035, #38314 ),
 ( #45021, #41296 ) ),
 .UNSPECIFIED., .T., .F., .F. ) 
 B_SPLINE_SURFACE_WITH_KNOTS ( ( 4, 3, 4 ),
 ( 2, 2 ),
 ( 0.000000000000000000, 0.5000000000000000000, 1.000000000000000000 ),
 ( 0.000000000000000000, 1.000000000000000000 ),
 .UNSPECIFIED. ) 
 GEOMETRIC_REPRESENTATION_ITEM ( )  RATIONAL_B_SPLINE_SURFACE ( (
 ( 1.000000000000000000, 1.000000000000000000),
 ( 0.3333333333333335369, 0.3333333333333330373),
 ( 0.3333333333333335369, 0.3333333333333330373),
 ( 1.000000000000000000, 1.000000000000000000),
 ( 0.3333333333333333703, 0.3333333333333333703),
 ( 0.3333333333333333703, 0.3333333333333333703),
 ( 1.000000000000000000, 1.000000000000000000) ) ) 
 REPRESENTATION_ITEM ( '' )  SURFACE ( )  );
#2834 = ORIENTED_EDGE ( 'NONE', *, *, #16274, .F. ) ;
#2835 = CYLINDRICAL_SURFACE ( 'NONE', #36295, 5.500000000000000000 ) ;
#2836 = CARTESIAN_POINT ( 'NONE',  ( -17.42409385541299471, -14.80920654474435771, 49.52966884056655772 ) ) ;
#2837 = ORIENTED_EDGE ( 'NONE', *, *, #17489, .F. ) ;
#2838 = DIRECTION ( 'NONE',  ( -8.993561335472250294E-07, 8.977735684497376994E-07, 0.9999999999991925348 ) ) ;
#2839 = EDGE_CURVE ( 'NONE', #21252, #31120, #13526, .T. ) ;
#2840 = VECTOR ( 'NONE', #5845, 1000.000000000000000 ) ;
#2841 = CIRCLE ( 'NONE', #45330, 0.3999999999999978018 ) ;
#2842 = VERTEX_POINT ( 'NONE', #13278 ) ;
#2843 = LINE ( 'NONE', #18096, #44954 ) ;
#2844 = CARTESIAN_POINT ( 'NONE',  ( -19.60046790782316251, -21.46228069541063732, 65.46486213989528835 ) ) ;
#2845 = EDGE_CURVE ( 'NONE', #20172, #38891, #14574, .T. ) ;
#2846 = EDGE_CURVE ( 'NONE', #14728, #2636, #43547, .T. ) ;
#2847 = CARTESIAN_POINT ( 'NONE',  ( -10.40127070788197017, -12.32249518151173895, 57.51352764219546998 ) ) ;
#2848 = VERTEX_POINT ( 'NONE', #17224 ) ;
#2849 = CARTESIAN_POINT ( 'NONE',  ( -12.81450527785482230, -9.474959380418823685, 74.61923006088066757 ) ) ;
#2850 = CARTESIAN_POINT ( 'NONE',  ( -22.83585279654753109, -10.36919270525743464, 63.35720607436116580 ) ) ;
#2851 = LINE ( 'NONE', #47925, #29984 ) ;
#2852 = ORIENTED_EDGE ( 'NONE', *, *, #16604, .F. ) ;
#2853 = CARTESIAN_POINT ( 'NONE',  ( -23.61204160381034711, -11.53669949605622769, 66.42214514747726639 ) ) ;
#2854 = DIRECTION ( 'NONE',  ( -0.6973657521612035559, 0.7167154300785205656, -1.015100525525034718E-08 ) ) ;
#2855 = CARTESIAN_POINT ( 'NONE',  ( -20.92409385541305511, -10.60920654474410618, 81.49999999999998579 ) ) ;
#2856 = ORIENTED_EDGE ( 'NONE', *, *, #466, .T. ) ;
#2857 = DIRECTION ( 'NONE',  ( -0.5497669574358331479, 0.8353180786453390239, 7.898837271846010071E-08 ) ) ;
#2858 = EDGE_CURVE ( 'NONE', #12172, #21456, #30294, .T. ) ;
#2859 = EDGE_LOOP ( 'NONE', ( #7531, #28675, #40101, #15893 ) ) ;
#2860 = CARTESIAN_POINT ( 'NONE',  ( -11.00561500425097528, -11.89266776388777380, 74.55840173649494318 ) ) ;
#2861 = CARTESIAN_POINT ( 'NONE',  ( -20.19231683483797468, -8.325423577284542631, 70.55100341277885434 ) ) ;
#2862 = DIRECTION ( 'NONE',  ( 3.413470714839332458E-33, -1.190614954331866791E-16, 1.000000000000000000 ) ) ;
#2863 = CARTESIAN_POINT ( 'NONE',  ( -24.31482381427648676, -13.31912605980313558, 59.36267924676594276 ) ) ;
#2864 = ORIENTED_EDGE ( 'NONE', *, *, #37278, .T. ) ;
#2865 = DIRECTION ( 'NONE',  ( 0.9687793358424821033, -0.2479245821708680464, 0.000000000000000000 ) ) ;
#2866 = CARTESIAN_POINT ( 'NONE',  ( -14.72778340125292651, -21.32322296975913645, 58.46617885012763338 ) ) ;
#2867 = DIRECTION ( 'NONE',  ( -0.8447509909909772796, 0.5351595679979588294, -3.339321029457348113E-17 ) ) ;
#2868 = ORIENTED_EDGE ( 'NONE', *, *, #10235, .F. ) ;
#2869 = CARTESIAN_POINT ( 'NONE',  ( -9.985760891864103428, -14.37924521898145258, 68.04455407903930109 ) ) ;
#2870 = B_SPLINE_CURVE_WITH_KNOTS ( 'NONE', 3,
 ( #20789, #35794, #2070, #5289, #12669, #35066, #27694, #2313, #31637, #24253 ),
 .UNSPECIFIED., .F., .F.,
 ( 4, 2, 2, 2, 4 ),
 ( 0.000000000000000000, 0.2500000000000000000, 0.5000000000000000000, 0.7500000000000000000, 1.000000000000000000 ),
 .UNSPECIFIED. ) ;
#2871 = CARTESIAN_POINT ( 'NONE',  ( -24.65023673758593148, -12.99629830290576038, 63.01759453279318279 ) ) ;
#2872 = EDGE_CURVE ( 'NONE', #18814, #29649, #26858, .T. ) ;
#2873 = VERTEX_POINT ( 'NONE', #32018 ) ;
#2874 = ORIENTED_EDGE ( 'NONE', *, *, #17770, .F. ) ;
#2875 = DIRECTION ( 'NONE',  ( 2.201155577252676169E-06, 7.355553122608190330E-06, 0.9999999999705252440 ) ) ;
#2876 = CARTESIAN_POINT ( 'NONE',  ( -16.00544582274271477, -7.903112417841744453, 63.95538887075813506 ) ) ;
#2877 = CARTESIAN_POINT ( 'NONE',  ( -23.82048026265336560, -11.84452950502918256, 59.78235734495926579 ) ) ;
#2878 = CARTESIAN_POINT ( 'NONE',  ( -10.40277084706750621, -15.44444119821074679, 57.86792809062918508 ) ) ;
#2879 = DIRECTION ( 'NONE',  ( -3.071710424422018668E-17, 6.404604876783312462E-16, 1.000000000000000000 ) ) ;
#2880 = CARTESIAN_POINT ( 'NONE',  ( -50.42409385541305511, -15.80920654474410725, 56.99999999999998579 ) ) ;
#2881 = CARTESIAN_POINT ( 'NONE',  ( -14.80056147340629380, -21.78207226143426922, 61.82095877133116346 ) ) ;
#2882 = VECTOR ( 'NONE', #26574, 1000.000000000000000 ) ;
#2883 = AXIS2_PLACEMENT_3D ( 'NONE', #34307, #45903, #11425 ) ;
#2884 = EDGE_LOOP ( 'NONE', ( #1523, #40900, #27884, #43501, #37097, #9722, #42896, #35000, #19040, #35792, #47064, #39509, #13409, #25009, #19684, #35865, #7342, #1386, #11327, #8219, #32206, #23486, #2559, #24103, #30649, #7267, #45817, #22573, #43360, #8362, #48431, #22142, #2392, #41518 ) ) ;
#2885 = ORIENTED_EDGE ( 'NONE', *, *, #22335, .T. ) ;
#2886 = CARTESIAN_POINT ( 'NONE',  ( -19.11145865927416310, -7.964113456900453691, 63.43089235103782642 ) ) ;
#2887 = CARTESIAN_POINT ( 'NONE',  ( -21.55204993259905066, -9.089641334111684401, 73.69309041467538179 ) ) ;
#2888 = DIRECTION ( 'NONE',  ( 0.8459089628457130416, 0.5333273165489315071, -7.771812505054809235E-08 ) ) ;
#2889 = CARTESIAN_POINT ( 'NONE',  ( -18.96371539328398725, -7.519906776682348415, 67.02258991573486924 ) ) ;
#2890 = VECTOR ( 'NONE', #15166, 1000.000000000000000 ) ;
#2891 = CARTESIAN_POINT ( 'NONE',  ( -10.00368807899092971, -15.89896712085359098, 53.49999999999994316 ) ) ;
#2892 = ORIENTED_EDGE ( 'NONE', *, *, #31131, .F. ) ;
#2893 = CARTESIAN_POINT ( 'NONE',  ( -20.61159385650551812, -6.922745924619793101, 51.69366785382590024 ) ) ;
#2894 = ORIENTED_EDGE ( 'NONE', *, *, #29597, .F. ) ;
#2895 = CARTESIAN_POINT ( 'NONE',  ( -22.05923648098858791, -20.05472392750071720, 62.23439162613904330 ) ) ;
#2896 = DIRECTION ( 'NONE',  ( -3.534154189880001717E-15, 4.519331686442879103E-31, 1.000000000000000000 ) ) ;
#2897 = CARTESIAN_POINT ( 'NONE',  ( -10.03035355355731006, -15.72374577095404824, 61.22284339518546403 ) ) ;
#2898 = ORIENTED_EDGE ( 'NONE', *, *, #33030, .F. ) ;
#2899 = CARTESIAN_POINT ( 'NONE',  ( -22.21990939174572333, -19.97672261113873660, 65.70421733412537435 ) ) ;
#2900 = CARTESIAN_POINT ( 'NONE',  ( -17.70613249112851761, -7.363797380145674865, 60.19405475747598899 ) ) ;
#2901 = EDGE_CURVE ( 'NONE', #30726, #42456, #39690, .T. ) ;
#2902 = CARTESIAN_POINT ( 'NONE',  ( -21.56832988282965857, -21.00015211897737899, 72.67446426350551292 ) ) ;
#2903 = CARTESIAN_POINT ( 'NONE',  ( -16.03618328653303848, -7.893388160315826241, 60.20028212586171890 ) ) ;
#2904 = ORIENTED_EDGE ( 'NONE', *, *, #28510, .F. ) ;
#2905 = DIRECTION ( 'NONE',  ( 1.616182858256114592E-16, 0.003028072113811714535, -0.9999954153791273948 ) ) ;
#2906 = VECTOR ( 'NONE', #39292, 1000.000000000000000 ) ;
#2907 = ORIENTED_EDGE ( 'NONE', *, *, #21080, .T. ) ;
#2908 = CARTESIAN_POINT ( 'NONE',  ( -24.37288983953117594, -15.99971190300345292, 66.06324957111131368 ) ) ;
#2909 = ADVANCED_FACE ( 'NONE', ( #1744 ), #13043, .T. ) ;
#2910 = ADVANCED_FACE ( 'NONE', ( #9379 ), #30316, .T. ) ;
#2911 = CARTESIAN_POINT ( 'NONE',  ( -11.25989503537269698, -11.38792718504117829, 64.29882039368452240 ) ) ;
#2912 = ORIENTED_EDGE ( 'NONE', *, *, #3392, .T. ) ;
#2913 = CARTESIAN_POINT ( 'NONE',  ( -18.50162525266306091, -21.72577549820248421, 72.58510940979837756 ) ) ;
#2914 = EDGE_CURVE ( 'NONE', #29156, #19709, #25018, .T. ) ;
#2915 = CARTESIAN_POINT ( 'NONE',  ( -12.84615363328625826, -20.17103110633857455, 72.09181604382622766 ) ) ;
#2916 = EDGE_LOOP ( 'NONE', ( #37319, #22808, #28235, #38298 ) ) ;
#2917 = CARTESIAN_POINT ( 'NONE',  ( -21.17409385541299116, -6.859212275519752211, 50.50378509014304029 ) ) ;
#2918 = CIRCLE ( 'NONE', #46976, 5.249999999999998224 ) ;
#2919 = ADVANCED_FACE ( 'NONE', ( #3670 ), #41960, .T. ) ;
#2920 = CARTESIAN_POINT ( 'NONE',  ( -24.72409385541305582, -14.80920654474415699, 62.02941176470587692 ) ) ;
#2921 = CARTESIAN_POINT ( 'NONE',  ( -21.57897937893636353, -8.625392431642884716, 73.80117520113515184 ) ) ;
#2922 = VERTEX_POINT ( 'NONE', #21658 ) ;
#2923 = CARTESIAN_POINT ( 'NONE',  ( -19.90432934692537614, -21.83431937171774706, 69.04987052938618319 ) ) ;
#2924 = B_SPLINE_CURVE_WITH_KNOTS ( 'NONE', 3,
 ( #47172, #10477, #28467, #6041, #44452, #3065, #21067, #10237, #48133, #47421 ),
 .UNSPECIFIED., .F., .F.,
 ( 4, 2, 2, 2, 4 ),
 ( 0.000000000000000000, 0.2500000000000000000, 0.5000000000000000000, 0.7500000000000000000, 1.000000000000000000 ),
 .UNSPECIFIED. ) ;
#2925 = CARTESIAN_POINT ( 'NONE',  ( -24.04756562706866418, -17.22461864935846876, 69.70780031821135481 ) ) ;
#2926 = DIRECTION ( 'NONE',  ( 0.3926557917762824590, -0.9196855055857630079, -5.808111619717073930E-09 ) ) ;
#2927 = EDGE_CURVE ( 'NONE', #30495, #47915, #33684, .T. ) ;
#2928 = ORIENTED_EDGE ( 'NONE', *, *, #735, .T. ) ;
#2929 = EDGE_LOOP ( 'NONE', ( #36857, #38318, #26533, #30939, #12333 ) ) ;
#2930 = DIRECTION ( 'NONE',  ( 3.071710424422018668E-17, -6.404604876783312462E-16, -1.000000000000000000 ) ) ;
#2931 = CARTESIAN_POINT ( 'NONE',  ( -11.84831518238830839, -10.57700509508930686, 71.04181123525845010 ) ) ;
#2932 = CARTESIAN_POINT ( 'NONE',  ( -17.78823985852933731, -7.818684566706888717, 60.08060768393342954 ) ) ;
#2933 = CARTESIAN_POINT ( 'NONE',  ( -16.53659385759799250, -8.995762431863214559, 51.38120296130585274 ) ) ;
#2934 = CARTESIAN_POINT ( 'NONE',  ( -22.88264614489240856, -10.34704276773305764, 63.35713876973677827 ) ) ;
#2935 = CARTESIAN_POINT ( 'NONE',  ( -13.83108396514174565, -21.33561889020367630, 72.04112409899799729 ) ) ;
#2936 = FACE_OUTER_BOUND ( 'NONE', #31371, .T. ) ;
#2937 = DIRECTION ( 'NONE',  ( 1.684279440454093594E-06, -5.535644408139047379E-06, 0.9999999999832598352 ) ) ;
#2938 = ORIENTED_EDGE ( 'NONE', *, *, #34457, .T. ) ;
#2939 = CARTESIAN_POINT ( 'NONE',  ( -10.54215788045047653, -13.52898884568911519, 74.78703633234691495 ) ) ;
#2940 = CYLINDRICAL_SURFACE ( 'NONE', #40810, 0.1500000000000014932 ) ;
#2941 = DIRECTION ( 'NONE',  ( 1.000000000000000000, -0.000000000000000000, 2.168404344971008375E-16 ) ) ;
#2942 = CARTESIAN_POINT ( 'NONE',  ( -12.35878062960998669, -9.253330100773967004, 53.76227901944321985 ) ) ;
#2943 =( BOUNDED_SURFACE ( )  B_SPLINE_SURFACE ( 3, 1, ( 
 ( #44270, #47221 ),
 ( #13466, #36833 ),
 ( #5859, #3119 ),
 ( #21371, #2401 ),
 ( #21120, #2151 ),
 ( #25303, #36359 ),
 ( #6092, #20875 ) ),
 .UNSPECIFIED., .T., .F., .F. ) 
 B_SPLINE_SURFACE_WITH_KNOTS ( ( 4, 3, 4 ),
 ( 2, 2 ),
 ( 0.000000000000000000, 0.5000000000000000000, 1.000000000000000000 ),
 ( 0.000000000000000000, 1.000000000000000000 ),
 .UNSPECIFIED. ) 
 GEOMETRIC_REPRESENTATION_ITEM ( )  RATIONAL_B_SPLINE_SURFACE ( (
 ( 1.000000000000000000, 1.000000000000000000),
 ( 0.3333333333333335369, 0.3333333333333330373),
 ( 0.3333333333333335369, 0.3333333333333330373),
 ( 1.000000000000000000, 1.000000000000000000),
 ( 0.3333333333333333703, 0.3333333333333333703),
 ( 0.3333333333333333703, 0.3333333333333333703),
 ( 1.000000000000000000, 1.000000000000000000) ) ) 
 REPRESENTATION_ITEM ( '' )  SURFACE ( )  );
#2944 = ORIENTED_EDGE ( 'NONE', *, *, #23691, .T. ) ;
#2945 = CIRCLE ( 'NONE', #25732, 1.999999999999999112 ) ;
#2946 = ORIENTED_EDGE ( 'NONE', *, *, #46580, .T. ) ;
#2947 = DIRECTION ( 'NONE',  ( 0.000000000000000000, 0.000000000000000000, 1.000000000000000000 ) ) ;
#2948 = CARTESIAN_POINT ( 'NONE',  ( -22.60239429201187278, -10.09890714409725199, 70.01178508710252402 ) ) ;
#2949 = CARTESIAN_POINT ( 'NONE',  ( -23.33763712988734440, -19.34056874305829510, 58.99072323483983382 ) ) ;
#2950 = FACE_OUTER_BOUND ( 'NONE', #46296, .T. ) ;
#2951 = VECTOR ( 'NONE', #21534, 1000.000000000000000 ) ;
#2952 = EDGE_CURVE ( 'NONE', #21408, #38015, #5341, .T. ) ;
#2953 =( BOUNDED_SURFACE ( )  B_SPLINE_SURFACE ( 3, 1, ( 
 ( #9739, #2336 ),
 ( #17344, #29166 ),
 ( #32387, #16182 ),
 ( #28680, #36527 ),
 ( #43715, #9969 ),
 ( #36298, #2581 ),
 ( #17584, #31224 ) ),
 .UNSPECIFIED., .T., .F., .F. ) 
 B_SPLINE_SURFACE_WITH_KNOTS ( ( 4, 3, 4 ),
 ( 2, 2 ),
 ( 0.000000000000000000, 0.5000000000000000000, 1.000000000000000000 ),
 ( 0.000000000000000000, 1.000000000000000000 ),
 .UNSPECIFIED. ) 
 GEOMETRIC_REPRESENTATION_ITEM ( )  RATIONAL_B_SPLINE_SURFACE ( (
 ( 1.000000000000000000, 1.000000000000000000),
 ( 0.3333333333333335369, 0.3333333333333330373),
 ( 0.3333333333333335369, 0.3333333333333330373),
 ( 1.000000000000000000, 1.000000000000000000),
 ( 0.3333333333333333703, 0.3333333333333333703),
 ( 0.3333333333333333703, 0.3333333333333333703),
 ( 1.000000000000000000, 1.000000000000000000) ) ) 
 REPRESENTATION_ITEM ( '' )  SURFACE ( )  );
#2954 = ORIENTED_EDGE ( 'NONE', *, *, #42838, .F. ) ;
#2955 = CARTESIAN_POINT ( 'NONE',  ( -24.45714095472541771, -14.31630891555219165, 69.66747352629326429 ) ) ;
#2956 = CARTESIAN_POINT ( 'NONE',  ( -11.29134393598116759, -11.33126488396075437, 64.16354160640879911 ) ) ;
#2957 = EDGE_CURVE ( 'NONE', #15234, #24799, #48719, .T. ) ;
#2958 = ORIENTED_EDGE ( 'NONE', *, *, #33706, .F. ) ;
#2959 = CARTESIAN_POINT ( 'NONE',  ( -8.424093855413067544, -8.109206544744111511, 50.49999999999999289 ) ) ;
#2960 = CARTESIAN_POINT ( 'NONE',  ( -24.47697530877170990, -14.85041752174647733, 63.12785080464042409 ) ) ;
#2961 = DIRECTION ( 'NONE',  ( -0.9918916210775229336, -0.1270866320121812332, 6.503929234589265847E-08 ) ) ;
#2962 = ORIENTED_EDGE ( 'NONE', *, *, #8108, .F. ) ;
#2963 = DIRECTION ( 'NONE',  ( -0.9294853595766551235, -0.3688590060343601706, 1.396818737099928616E-16 ) ) ;
#2964 =( BOUNDED_CURVE ( )  B_SPLINE_CURVE ( 3, ( #28897, #33534, #39990, #6740 ),
 .UNSPECIFIED., .F., .F. ) 
 B_SPLINE_CURVE_WITH_KNOTS ( ( 4, 4 ),
 ( 0.5000000000000000000, 0.9074455897393621795 ),
 .UNSPECIFIED. ) 
 CURVE ( )  GEOMETRIC_REPRESENTATION_ITEM ( )  RATIONAL_B_SPLINE_CURVE ( ( 1.000000000000000888, 0.4567392136813415160, 0.3561768502900331534, 0.6983129098260766332 ) ) 
 REPRESENTATION_ITEM ( '' )  );
#2965 = ORIENTED_EDGE ( 'NONE', *, *, #48207, .F. ) ;
#2966 = CARTESIAN_POINT ( 'NONE',  ( -10.99582063857411995, -11.91441743271276188, 74.55840195587596497 ) ) ;
#2967 = ORIENTED_EDGE ( 'NONE', *, *, #28625, .T. ) ;
#2968 = LINE ( 'NONE', #32769, #20724 ) ;
#2969 = CARTESIAN_POINT ( 'NONE',  ( -24.49635618495769407, -12.46679672499890046, 73.35730262454691797 ) ) ;
#2970 = EDGE_CURVE ( 'NONE', #47542, #18577, #3182, .T. ) ;
#2971 = CARTESIAN_POINT ( 'NONE',  ( -14.33942418930512019, -10.56099362034968614, 49.52966884056655772 ) ) ;
#2972 = B_SPLINE_CURVE_WITH_KNOTS ( 'NONE', 1,
 ( #44519, #3143 ),
 .UNSPECIFIED., .F., .F.,
 ( 2, 2 ),
 ( 0.000000000000000000, 1.000000000000000000 ),
 .UNSPECIFIED. ) ;
#2973 = AXIS2_PLACEMENT_3D ( 'NONE', #33729, #30074, #19219 ) ;
#2974 = EDGE_CURVE ( 'NONE', #41284, #24527, #39070, .T. ) ;
#2975 = AXIS2_PLACEMENT_3D ( 'NONE', #21900, #21437, #33442 ) ;
#2976 = CARTESIAN_POINT ( 'NONE',  ( -24.86610161942810038, -14.46236550061385984, 66.29797407254456232 ) ) ;
#2977 = FACE_OUTER_BOUND ( 'NONE', #38275, .T. ) ;
#2978 = DIRECTION ( 'NONE',  ( -3.071710424422018668E-17, 6.404604876783312462E-16, 1.000000000000000000 ) ) ;
#2979 = ORIENTED_EDGE ( 'NONE', *, *, #32814, .T. ) ;
#2980 = CARTESIAN_POINT ( 'NONE',  ( -20.57801275890795267, -8.499987852562307822, 66.87284105708988591 ) ) ;
#2981 = AXIS2_PLACEMENT_3D ( 'NONE', #8332, #20626, #46491 ) ;
#2982 = AXIS2_PLACEMENT_3D ( 'NONE', #26974, #23958, #28376 ) ;
#2983 = CARTESIAN_POINT ( 'NONE',  ( -19.66559402580761784, -10.06176755239059872, 49.52966884056655772 ) ) ;
#2984 = CARTESIAN_POINT ( 'NONE',  ( -46.29409385541305255, -13.24559821555319061, 71.00222776205100672 ) ) ;
#2985 = FACE_OUTER_BOUND ( 'NONE', #21104, .T. ) ;
#2986 = EDGE_CURVE ( 'NONE', #12909, #43562, #43194, .T. ) ;
#2987 = CARTESIAN_POINT ( 'NONE',  ( -16.52839481157216639, -21.81011260682906183, 58.44152394349971047 ) ) ;
#2988 = CARTESIAN_POINT ( 'NONE',  ( -24.20300570612225499, -13.06358601049079482, 62.84766556631919343 ) ) ;
#2989 = ORIENTED_EDGE ( 'NONE', *, *, #43931, .F. ) ;
#2990 = ORIENTED_EDGE ( 'NONE', *, *, #29440, .T. ) ;
#2991 = B_SPLINE_CURVE_WITH_KNOTS ( 'NONE', 3,
 ( #15371, #3839, #22543, #15622, #30193, #26970, #14625, #44977, #11226, #30678 ),
 .UNSPECIFIED., .F., .F.,
 ( 4, 2, 2, 2, 4 ),
 ( 0.6272669072877863350, 0.7522669073072822954, 0.8772669073267782558, 1.002266907346274216, 1.127266907365770177 ),
 .UNSPECIFIED. ) ;
#2992 = CARTESIAN_POINT ( 'NONE',  ( -16.98261445675647963, -21.79527095473675402, 72.46543221550747660 ) ) ;
#2993 = DIRECTION ( 'NONE',  ( 0.000000000000000000, 0.000000000000000000, 1.000000000000000000 ) ) ;
#2994 = ORIENTED_EDGE ( 'NONE', *, *, #25328, .T. ) ;
#2996 = FACE_OUTER_BOUND ( 'NONE', #30465, .T. ) ;
#2995 = CARTESIAN_POINT ( 'NONE',  ( -17.42260713176972686, -20.05920633423509258, 49.52966884056656482 ) ) ;
#2997 = CARTESIAN_POINT ( 'NONE',  ( -11.34825743494507400, -18.28566363406474693, 58.10714629622172112 ) ) ;
#2998 = CARTESIAN_POINT ( 'NONE',  ( -45.55409385541305767, -12.76354662275040219, 69.95698270748289360 ) ) ;
#2999 = CARTESIAN_POINT ( 'NONE',  ( -12.10599122619147749, -20.02663529450013513, 61.58173959111590534 ) ) ;
#3000 = ADVANCED_FACE ( 'NONE', ( #44558 ), #25834, .T. ) ;
#3001 = CARTESIAN_POINT ( 'NONE',  ( -24.83433702558981082, -14.04005949775414663, 73.22997357260834406 ) ) ;
#3002 = CARTESIAN_POINT ( 'NONE',  ( -23.33103958787803478, -18.66444169543841269, 73.06368517745727331 ) ) ;
#3003 = CARTESIAN_POINT ( 'NONE',  ( -14.84243821726248314, -7.820811810980328183, 57.05011197146747293 ) ) ;
#3004 = VERTEX_POINT ( 'NONE', #10814 ) ;
#3005 = DIRECTION ( 'NONE',  ( 3.413470714839332458E-33, -1.190614954331866791E-16, 1.000000000000000000 ) ) ;
#3006 = CARTESIAN_POINT ( 'NONE',  ( -10.59656512619885227, -13.05092609425065220, 68.02360230423869325 ) ) ;
#3007 = CARTESIAN_POINT ( 'NONE',  ( -18.05440415122280839, -21.83127237841607027, 65.36004252941745563 ) ) ;
#3008 = CARTESIAN_POINT ( 'NONE',  ( -24.18639045584301428, -17.93591939540326408, 59.14231917793316740 ) ) ;
#3009 = CYLINDRICAL_SURFACE ( 'NONE', #19699, 0.1499999999999981903 ) ;
#3010 = DIRECTION ( 'NONE',  ( -0.9687793358424822143, 0.2479245821708672415, 0.000000000000000000 ) ) ;
#3011 = VERTEX_POINT ( 'NONE', #22154 ) ;
#3012 = ORIENTED_EDGE ( 'NONE', *, *, #1432, .T. ) ;
#3013 = CARTESIAN_POINT ( 'NONE',  ( -16.16784385541304303, -9.357632978295830739, 49.97845033065684106 ) ) ;
#3014 = ORIENTED_EDGE ( 'NONE', *, *, #17654, .F. ) ;
#3015 = CARTESIAN_POINT ( 'NONE',  ( -16.98261445675647963, -21.79527095473675402, 72.46543221550747660 ) ) ;
#3016 = CIRCLE ( 'NONE', #47036, 4.686499999999998778 ) ;
#3017 = DIRECTION ( 'NONE',  ( 0.000000000000000000, -0.9999954153791273948, -0.003028072113819838245 ) ) ;
#3018 = STYLED_ITEM ( 'NONE', ( #7702 ), #48569 ) ;
#3019 = EDGE_CURVE ( 'NONE', #45804, #16141, #8310, .T. ) ;
#3020 = VECTOR ( 'NONE', #117, 1000.000000000000000 ) ;
#3021 = CARTESIAN_POINT ( 'NONE',  ( -15.74783386771837890, -7.961078896070159061, 70.62461975990308360 ) ) ;
#3022 = CARTESIAN_POINT ( 'NONE',  ( -16.52839481157216639, -21.81011260682906183, 58.44152394349971047 ) ) ;
#3023 = ORIENTED_EDGE ( 'NONE', *, *, #40879, .T. ) ;
#3024 = CARTESIAN_POINT ( 'NONE',  ( -16.27008067537174796, -7.904986561263926959, 60.50028479261354875 ) ) ;
#3025 = CIRCLE ( 'NONE', #8564, 1.250000000000001110 ) ;
#3026 = FACE_OUTER_BOUND ( 'NONE', #16486, .T. ) ;
#3027 = EDGE_LOOP ( 'NONE', ( #18259, #31844, #3708, #42426 ) ) ;
#3028 = CARTESIAN_POINT ( 'NONE',  ( -24.42173158788804699, -14.58342405553281473, 66.41122531969938336 ) ) ;
#3029 = CARTESIAN_POINT ( 'NONE',  ( -12.55198883488284878, -12.25722835735234639, 54.07175714974878389 ) ) ;
#3030 = ORIENTED_EDGE ( 'NONE', *, *, #37682, .T. ) ;
#3031 = CARTESIAN_POINT ( 'NONE',  ( -19.36683724782897897, -21.58655468785150688, 62.00975759738177118 ) ) ;
#3032 = CARTESIAN_POINT ( 'NONE',  ( -22.26799053462541522, -13.56958363389006905, 53.27966884056655061 ) ) ;
#3033 = CARTESIAN_POINT ( 'NONE',  ( -9.978987780385143225, -14.53464483151434372, 67.99653628095502711 ) ) ;
#3034 = ORIENTED_EDGE ( 'NONE', *, *, #36794, .T. ) ;
#3035 = CARTESIAN_POINT ( 'NONE',  ( -20.19591720527444778, -7.893910298445437235, 73.89909326007249035 ) ) ;
#3036 = EDGE_CURVE ( 'NONE', #13279, #4206, #38354, .T. ) ;
#3037 = CARTESIAN_POINT ( 'NONE',  ( -24.82767328945774210, -13.97813652794827988, 73.16625576376715401 ) ) ;
#3038 = EDGE_CURVE ( 'NONE', #41056, #11741, #29724, .T. ) ;
#3039 = CARTESIAN_POINT ( 'NONE',  ( -24.69822986944709697, -13.19963441799314197, 59.54763197719577761 ) ) ;
#3040 = FACE_OUTER_BOUND ( 'NONE', #35287, .T. ) ;
#3041 = EDGE_LOOP ( 'NONE', ( #23030, #43391, #22933, #19767 ) ) ;
#3042 = DIRECTION ( 'NONE',  ( -2.584300828889512628E-08, -1.497441464807615962E-06, 0.9999999999988784527 ) ) ;
#3043 = CARTESIAN_POINT ( 'NONE',  ( -22.92319923916556590, -10.39759239192951235, 63.07185995337425055 ) ) ;
#3044 = EDGE_CURVE ( 'NONE', #13463, #20348, #16117, .T. ) ;
#3045 = CARTESIAN_POINT ( 'NONE',  ( -22.35534385650551670, -7.417179338643134834, 52.18511593390279302 ) ) ;
#3046 = AXIS2_PLACEMENT_3D ( 'NONE', #41887, #41639, #15267 ) ;
#3047 = CYLINDRICAL_SURFACE ( 'NONE', #37681, 0.1500000000000007716 ) ;
#3048 = CARTESIAN_POINT ( 'NONE',  ( -17.95017679193155047, -22.24060860892481628, 62.02535923035622289 ) ) ;
#3049 = VERTEX_POINT ( 'NONE', #30769 ) ;
#3050 = LINE ( 'NONE', #32842, #33116 ) ;
#3051 =( BOUNDED_CURVE ( )  B_SPLINE_CURVE ( 3, ( #15242, #11570, #25611, #33463 ),
 .UNSPECIFIED., .F., .F. ) 
 B_SPLINE_CURVE_WITH_KNOTS ( ( 4, 4 ),
 ( 0.000000000000000000, 0.4074455897393602921 ),
 .UNSPECIFIED. ) 
 CURVE ( )  GEOMETRIC_REPRESENTATION_ITEM ( )  RATIONAL_B_SPLINE_CURVE ( ( 1.000000000000000000, 0.4567392136813441250, 0.3561768502900348188, 0.6983129098260720813 ) ) 
 REPRESENTATION_ITEM ( '' )  );
#3052 = EDGE_CURVE ( 'NONE', #27215, #13964, #26178, .T. ) ;
#3053 = CARTESIAN_POINT ( 'NONE',  ( -15.50784783684063051, -8.076599273749138774, 74.07985659288991087 ) ) ;
#3054 = CARTESIAN_POINT ( 'NONE',  ( -18.56115164150112662, -7.446410555819776178, 73.88418448558978469 ) ) ;
#3055 = B_SPLINE_CURVE_WITH_KNOTS ( 'NONE', 3,
 ( #24468, #13823, #16801, #43423, #39710, #28864, #17035, #39472, #13344, #36001 ),
 .UNSPECIFIED., .F., .F.,
 ( 4, 2, 2, 2, 4 ),
 ( 0.000000000000000000, 0.2500000000000000000, 0.5000000000000000000, 0.7500000000000000000, 1.000000000000000000 ),
 .UNSPECIFIED. ) ;
#3056 = VERTEX_POINT ( 'NONE', #42080 ) ;
#3057 = CARTESIAN_POINT ( 'NONE',  ( -10.05862351292959467, -15.92886012141397245, 64.69266982328383619 ) ) ;
#3058 = CIRCLE ( 'NONE', #47886, 2.000000000000000000 ) ;
#3059 = B_SPLINE_CURVE_WITH_KNOTS ( 'NONE', 3,
 ( #19339, #1111, #27221, #23539, #23784, #31151, #38277, #42736, #38537, #30446 ),
 .UNSPECIFIED., .F., .F.,
 ( 4, 2, 2, 2, 4 ),
 ( 0.6272669072782822708, 0.7522669073001799767, 0.8772669073220777936, 1.002266907343975610, 1.127266907365873205 ),
 .UNSPECIFIED. ) ;
#3060 = VERTEX_POINT ( 'NONE', #16192 ) ;
#3061 = ORIENTED_EDGE ( 'NONE', *, *, #29431, .F. ) ;
#3062 = ORIENTED_EDGE ( 'NONE', *, *, #43174, .F. ) ;
#3063 = VECTOR ( 'NONE', #10142, 1000.000000000000114 ) ;
#3064 = CARTESIAN_POINT ( 'NONE',  ( -11.32522400900782067, -11.27219014254736074, 60.96413645226084554 ) ) ;
#3065 = CARTESIAN_POINT ( 'NONE',  ( -15.93141941972390008, -7.970206387582725149, 63.86114100741836808 ) ) ;
#3066 = EDGE_CURVE ( 'NONE', #22327, #5003, #23365, .T. ) ;
#3067 = CARTESIAN_POINT ( 'NONE',  ( -22.16159385759798894, -7.228003583438117552, 51.38655588711986155 ) ) ;
#3068 = EDGE_CURVE ( 'NONE', #45257, #20025, #17116, .T. ) ;
#3069 = ORIENTED_EDGE ( 'NONE', *, *, #19985, .F. ) ;
#3070 = ORIENTED_EDGE ( 'NONE', *, *, #9498, .F. ) ;
#3071 = CARTESIAN_POINT ( 'NONE',  ( -16.87409385650551386, -9.792211528768504536, 50.49490371617623197 ) ) ;
#3072 = B_SPLINE_CURVE_WITH_KNOTS ( 'NONE', 3,
 ( #28973, #6812, #13456, #20865, #21362, #2630, #36352, #10276, #21829, #18116 ),
 .UNSPECIFIED., .F., .F.,
 ( 4, 2, 2, 2, 4 ),
 ( 0.000000000000000000, 0.2500000000000000000, 0.5000000000000000000, 0.7500000000000000000, 1.000000000000000000 ),
 .UNSPECIFIED. ) ;
#3073 = EDGE_CURVE ( 'NONE', #15483, #2214, #960, .T. ) ;
#3074 = B_SPLINE_CURVE_WITH_KNOTS ( 'NONE', 3,
 ( #40611, #41116, #26588, #14483, #33963, #48247, #3196, #6895, #17955, #18445 ),
 .UNSPECIFIED., .F., .F.,
 ( 4, 2, 2, 2, 4 ),
 ( 0.000000000000000000, 0.2500000000000000000, 0.5000000000000000000, 0.7500000000000000000, 1.000000000000000000 ),
 .UNSPECIFIED. ) ;
#3076 = EDGE_CURVE ( 'NONE', #14119, #42743, #38360, .T. ) ;
#3075 = CARTESIAN_POINT ( 'NONE',  ( -19.88388893082392528, -8.193741602349351894, 70.40667630031393287 ) ) ;
#3077 = CARTESIAN_POINT ( 'NONE',  ( -22.05923734882601295, -20.05472318235705131, 62.53439162613685909 ) ) ;
#3078 = CARTESIAN_POINT ( 'NONE',  ( -17.77409385650551243, -9.792211528768504536, 50.49490371617623197 ) ) ;
#3079 = EDGE_LOOP ( 'NONE', ( #19123, #47899 ) ) ;
#3080 = DIRECTION ( 'NONE',  ( -3.071710424422018668E-17, 6.404604876783312462E-16, 1.000000000000000000 ) ) ;
#3081 = CARTESIAN_POINT ( 'NONE',  ( -22.11022017764905456, -20.07639638992645104, 62.53439153403956396 ) ) ;
#3082 = CARTESIAN_POINT ( 'NONE',  ( -22.09234508783963236, -20.09219152016766685, 62.38439162497947166 ) ) ;
#3083 = EDGE_LOOP ( 'NONE', ( #26250, #25541, #27967, #44915, #38356 ) ) ;
#3084 = DIRECTION ( 'NONE',  ( 1.000000000000000000, -0.000000000000000000, 0.000000000000000000 ) ) ;
#3085 = CIRCLE ( 'NONE', #12553, 2.000000000000000444 ) ;
#3086 = CIRCLE ( 'NONE', #29819, 2.000000000000001332 ) ;
#3087 = VERTEX_POINT ( 'NONE', #34426 ) ;
#3088 = DIRECTION ( 'NONE',  ( -0.000000000000000000, -1.000000000000000000, -0.000000000000000000 ) ) ;
#3089 = CARTESIAN_POINT ( 'NONE',  ( -24.83010077369927515, -14.00069395148988605, 73.32260284066204292 ) ) ;
#3090 = CARTESIAN_POINT ( 'NONE',  ( -21.59804182614902146, -20.98026282434625500, 72.70941811628220819 ) ) ;
#3091 = ORIENTED_EDGE ( 'NONE', *, *, #46108, .F. ) ;
#3092 = CARTESIAN_POINT ( 'NONE',  ( -10.70532053225239366, -12.67267096592666675, 61.08381491717225487 ) ) ;
#3093 = LINE ( 'NONE', #33354, #35988 ) ;
#3094 =( BOUNDED_SURFACE ( )  B_SPLINE_SURFACE ( 3, 1, ( 
 ( #24431, #27863 ),
 ( #43386, #42890 ),
 ( #35488, #16766 ),
 ( #27629, #31805 ),
 ( #35720, #13069 ),
 ( #9406, #9655 ),
 ( #8685, #2240 ) ),
 .UNSPECIFIED., .T., .F., .F. ) 
 B_SPLINE_SURFACE_WITH_KNOTS ( ( 4, 3, 4 ),
 ( 2, 2 ),
 ( 0.000000000000000000, 0.5000000000000000000, 1.000000000000000000 ),
 ( 0.000000000000000000, 1.000000000000000000 ),
 .UNSPECIFIED. ) 
 GEOMETRIC_REPRESENTATION_ITEM ( )  RATIONAL_B_SPLINE_SURFACE ( (
 ( 1.000000000000000000, 1.000000000000000000),
 ( 0.3333333333333335369, 0.3333333333333330373),
 ( 0.3333333333333335369, 0.3333333333333330373),
 ( 1.000000000000000000, 1.000000000000000000),
 ( 0.3333333333333333703, 0.3333333333333333703),
 ( 0.3333333333333333703, 0.3333333333333333703),
 ( 1.000000000000000000, 1.000000000000000000) ) ) 
 REPRESENTATION_ITEM ( '' )  SURFACE ( )  );
#3095 = CARTESIAN_POINT ( 'NONE',  ( -22.96475595555910942, -9.828888949534857034, 70.16178519762588905 ) ) ;
#3096 = CARTESIAN_POINT ( 'NONE',  ( -10.09159279195849379, -16.12743201725144360, 68.17041960190522332 ) ) ;
#3097 = ORIENTED_EDGE ( 'NONE', *, *, #33554, .T. ) ;
#3098 = DIRECTION ( 'NONE',  ( -2.866981220435666553E-17, 1.000000000000000000, 1.190614954331866791E-16 ) ) ;
#3099 = CARTESIAN_POINT ( 'NONE',  ( -21.36564388993269148, -20.65448255276599809, 72.82446398674419186 ) ) ;
#3100 = CARTESIAN_POINT ( 'NONE',  ( -21.52725980274252393, -9.076272844571150245, 70.43132538913752683 ) ) ;
#3101 = ORIENTED_EDGE ( 'NONE', *, *, #17983, .T. ) ;
#3102 = LINE ( 'NONE', #11720, #25007 ) ;
#3104 = EDGE_CURVE ( 'NONE', #3303, #10012, #18937, .T. ) ;
#3103 = ORIENTED_EDGE ( 'NONE', *, *, #32752, .F. ) ;
#3105 = CARTESIAN_POINT ( 'NONE',  ( -13.12040755923265500, -20.89053954678383462, 58.22462863256119903 ) ) ;
#3106 = CARTESIAN_POINT ( 'NONE',  ( -12.79725838692604434, -20.12850099319811292, 71.80653676770127447 ) ) ;
#3107 = DIRECTION ( 'NONE',  ( -0.9687793358424819923, 0.2479245821708680464, 0.000000000000000000 ) ) ;
#3108 = ADVANCED_FACE ( 'NONE', ( #11803 ), #34756, .T. ) ;
#3109 = CARTESIAN_POINT ( 'NONE',  ( -21.17162584072666220, -21.24822939621656559, 65.72420603834571295 ) ) ;
#3110 = ORIENTED_EDGE ( 'NONE', *, *, #44313, .F. ) ;
#3111 = CARTESIAN_POINT ( 'NONE',  ( -22.07364868997043672, -9.574310151912669653, 59.83244270001737419 ) ) ;
#3112 = ORIENTED_EDGE ( 'NONE', *, *, #48606, .F. ) ;
#3113 = CARTESIAN_POINT ( 'NONE',  ( -11.16004581379495342, -11.56782820372427167, 64.03393219759587396 ) ) ;
#3114 = B_SPLINE_CURVE_WITH_KNOTS ( 'NONE', 3,
 ( #6814, #39577, #21831, #29464, #21599, #32669, #10746, #39817, #32896, #40536 ),
 .UNSPECIFIED., .F., .F.,
 ( 4, 2, 2, 2, 4 ),
 ( 0.000000000000000000, 0.2500000000000000000, 0.5000000000000000000, 0.7500000000000000000, 1.000000000000000000 ),
 .UNSPECIFIED. ) ;
#3115 = CARTESIAN_POINT ( 'NONE',  ( -15.41750689856725565, -7.634439986883705842, 74.33631595678771475 ) ) ;
#3116 = ORIENTED_EDGE ( 'NONE', *, *, #38582, .F. ) ;
#3117 = DIRECTION ( 'NONE',  ( -3.071710424422018668E-17, 6.404604876783312462E-16, 1.000000000000000000 ) ) ;
#3118 =( BOUNDED_CURVE ( )  B_SPLINE_CURVE ( 3, ( #3780, #37739, #30382, #42181 ),
 .UNSPECIFIED., .F., .F. ) 
 B_SPLINE_CURVE_WITH_KNOTS ( ( 4, 4 ),
 ( 0.5000000000000000000, 0.9074455897393630677 ),
 .UNSPECIFIED. ) 
 CURVE ( )  GEOMETRIC_REPRESENTATION_ITEM ( )  RATIONAL_B_SPLINE_CURVE ( ( 0.9999999999999968914, 0.4567392136813352987, 0.3561768502900335975, 0.6983129098260885126 ) ) 
 REPRESENTATION_ITEM ( '' )  );
#3119 = CARTESIAN_POINT ( 'NONE',  ( -11.96194199484143539, -9.742791280557115741, 60.60272182217008208 ) ) ;
#3120 = ORIENTED_EDGE ( 'NONE', *, *, #23272, .F. ) ;
#3121 = VERTEX_POINT ( 'NONE', #19419 ) ;
#3122 = CARTESIAN_POINT ( 'NONE',  ( -14.93108437845038594, -21.82978844404615160, 65.36242591972883531 ) ) ;
#3124 = CARTESIAN_POINT ( 'NONE',  ( -15.19549097431359463, -21.91815212410659086, 68.76088336006283441 ) ) ;
#3123 = AXIS2_PLACEMENT_3D ( 'NONE', #35313, #1588, #20062 ) ;
#3125 = ORIENTED_CLOSED_SHELL ( 'NONE', *, #8687, .F. );
#3126 = CARTESIAN_POINT ( 'NONE',  ( -23.46236539141196076, -19.17297946188329405, 62.46068554577072263 ) ) ;
#3127 = DIRECTION ( 'NONE',  ( 1.916827916228666765E-06, 6.156520255201565618E-06, -0.9999999999792115180 ) ) ;
#3128 = CARTESIAN_POINT ( 'NONE',  ( -17.42409385541299471, -14.80920654474435594, 52.02966884056656482 ) ) ;
#3129 = DIRECTION ( 'NONE',  ( 0.9753750245375037986, 0.2205528542287732707, 7.244220459260263973E-08 ) ) ;
#3130 = CARTESIAN_POINT ( 'NONE',  ( -20.31413516131974362, -8.378470924821744603, 67.06632013881642251 ) ) ;
#3131 = AXIS2_PLACEMENT_3D ( 'NONE', #27483, #24540, #9261 ) ;
#3132 = EDGE_CURVE ( 'NONE', #9892, #28, #32626, .T. ) ;
#3133 = ORIENTED_EDGE ( 'NONE', *, *, #452, .F. ) ;
#3134 = ORIENTED_EDGE ( 'NONE', *, *, #8371, .F. ) ;
#3135 = CARTESIAN_POINT ( 'NONE',  ( -24.30048588269890431, -16.36411231998812710, 59.12332431758469653 ) ) ;
#3136 = EDGE_CURVE ( 'NONE', #35971, #9441, #7968, .T. ) ;
#3137 = EDGE_CURVE ( 'NONE', #26463, #45860, #35232, .T. ) ;
#3138 = ADVANCED_FACE ( 'NONE', ( #43542 ), #1921, .F. ) ;
#3139 = DIRECTION ( 'NONE',  ( -1.000000000000000000, -1.669677910507523057E-21, -6.493791346278465266E-22 ) ) ;
#3140 = DIRECTION ( 'NONE',  ( 0.000000000000000000, 0.000000000000000000, 1.000000000000000000 ) ) ;
#3141 = CIRCLE ( 'NONE', #33821, 4.686500000000000554 ) ;
#3142 = CARTESIAN_POINT ( 'NONE',  ( -18.96308807049092238, -7.519770507884219413, 67.07788641161226906 ) ) ;
#3143 = CARTESIAN_POINT ( 'NONE',  ( -23.34092575347512266, -10.28207967581048088, 59.78698817202694471 ) ) ;
#3144 = ORIENTED_EDGE ( 'NONE', *, *, #17911, .T. ) ;
#3145 = B_SPLINE_CURVE_WITH_KNOTS ( 'NONE', 3,
 ( #25114, #2692, #27050, #11799, #26085, #7871, #19415, #42075, #48474, #4397 ),
 .UNSPECIFIED., .F., .F.,
 ( 4, 2, 2, 2, 4 ),
 ( 0.1272669073658451999, 0.2522669073488033042, 0.3772669073317613808, 0.5022669073147194574, 0.6272669072976775340 ),
 .UNSPECIFIED. ) ;
#3146 = CARTESIAN_POINT ( 'NONE',  ( -20.78034385650551386, -6.424090610841174609, 49.80797279389977916 ) ) ;
#3147 = VERTEX_POINT ( 'NONE', #9320 ) ;
#3148 = CARTESIAN_POINT ( 'NONE',  ( -15.32409385541304481, -9.359200813967568422, 50.49621490985804684 ) ) ;
#3149 = CARTESIAN_POINT ( 'NONE',  ( -11.05034076241727625, -11.79557573020262318, 71.37388789199357575 ) ) ;
#3150 = CARTESIAN_POINT ( 'NONE',  ( -18.20818224600564150, -22.21799970308342154, 65.50565518846025270 ) ) ;
#3151 = ORIENTED_EDGE ( 'NONE', *, *, #21193, .F. ) ;
#3152 = CYLINDRICAL_SURFACE ( 'NONE', #21202, 0.1500000000000048794 ) ;
#3153 = CARTESIAN_POINT ( 'NONE',  ( -21.39967327233876304, -20.63170314183283693, 72.80974286114339122 ) ) ;
#3154 = EDGE_CURVE ( 'NONE', #1265, #20388, #5384, .T. ) ;
#3155 = VECTOR ( 'NONE', #7116, 1000.000000000000227 ) ;
#3156 = ORIENTED_EDGE ( 'NONE', *, *, #27149, .T. ) ;
#3157 = FACE_OUTER_BOUND ( 'NONE', #880, .T. ) ;
#3158 = CIRCLE ( 'NONE', #47216, 4.686499999999997002 ) ;
#3159 = ORIENTED_EDGE ( 'NONE', *, *, #34982, .F. ) ;
#3160 = DIRECTION ( 'NONE',  ( -3.549360974554993999E-17, 6.371834667797928663E-18, 1.000000000000000000 ) ) ;
#3161 = VECTOR ( 'NONE', #37100, 1000.000000000000000 ) ;
#3162 = ORIENTED_EDGE ( 'NONE', *, *, #23073, .T. ) ;
#3163 =( BOUNDED_CURVE ( )  B_SPLINE_CURVE ( 3, ( #15631, #38274, #35075, #45457 ),
 .UNSPECIFIED., .F., .F. ) 
 B_SPLINE_CURVE_WITH_KNOTS ( ( 4, 4 ),
 ( 0.5000000000000000000, 0.9074455897393711723 ),
 .UNSPECIFIED. ) 
 CURVE ( )  GEOMETRIC_REPRESENTATION_ITEM ( )  RATIONAL_B_SPLINE_CURVE ( ( 0.9999999999999897859, 0.4567392136813225867, 0.3561768502900338751, 0.6983129098261126044 ) ) 
 REPRESENTATION_ITEM ( '' )  );
#3164 = LINE ( 'NONE', #17455, #12414 ) ;
#3165 = CARTESIAN_POINT ( 'NONE',  ( -17.65301634040397261, -7.362555908020970818, 63.69023642131870133 ) ) ;
#3166 = VERTEX_POINT ( 'NONE', #1429 ) ;
#3167 = CARTESIAN_POINT ( 'NONE',  ( -12.82148049030644366, -13.86501071932494789, 49.52966884056655772 ) ) ;
#3168 = CARTESIAN_POINT ( 'NONE',  ( -20.29576906775320921, -8.423958474866362067, 70.32270528577072355 ) ) ;
#3169 = EDGE_CURVE ( 'NONE', #22665, #37829, #32209, .T. ) ;
#3170 = VERTEX_POINT ( 'NONE', #17416 ) ;
#3171 = FACE_OUTER_BOUND ( 'NONE', #29667, .T. ) ;
#3172 = AXIS2_PLACEMENT_3D ( 'NONE', #9459, #20774, #31855 ) ;
#3173 = DIRECTION ( 'NONE',  ( 3.071710424422018668E-17, -6.404604876783312462E-16, -1.000000000000000000 ) ) ;
#3174 = CARTESIAN_POINT ( 'NONE',  ( -10.72552571836178181, -12.61109718544098612, 60.79853568372239891 ) ) ;
#3175 = ORIENTED_EDGE ( 'NONE', *, *, #14116, .T. ) ;
#3176 = CARTESIAN_POINT ( 'NONE',  ( -10.48067321144888808, -16.03043919553437036, 68.12767830706636119 ) ) ;
#3177 = CARTESIAN_POINT ( 'NONE',  ( -11.36226365097591184, -11.30848497612717374, 60.69388164123920859 ) ) ;
#3178 = CARTESIAN_POINT ( 'NONE',  ( -21.34582186320181307, -20.66775149956831115, 72.82446429489806405 ) ) ;
#3179 = VERTEX_POINT ( 'NONE', #46745 ) ;
#3180 = ORIENTED_EDGE ( 'NONE', *, *, #33371, .T. ) ;
#3181 = CARTESIAN_POINT ( 'NONE',  ( -14.07539661982785262, -8.605278201040592378, 74.34954655214895070 ) ) ;
#3182 = LINE ( 'NONE', #44093, #3752 ) ;
#3183 = CARTESIAN_POINT ( 'NONE',  ( -20.77185612116493374, -8.153571591454063849, 63.47268022219622452 ) ) ;
#3184 = CARTESIAN_POINT ( 'NONE',  ( -14.45534385759799179, -8.623186033802571870, 49.24843789510467218 ) ) ;
#3185 = CARTESIAN_POINT ( 'NONE',  ( -15.87557486115803052, -7.931373420853707223, 67.44007279014866185 ) ) ;
#3186 = CARTESIAN_POINT ( 'NONE',  ( -13.83248983650026709, -21.33638410845934885, 72.18253639678975730 ) ) ;
#3187 = FACE_OUTER_BOUND ( 'NONE', #37840, .T. ) ;
#3188 = CARTESIAN_POINT ( 'NONE',  ( -16.56761320685650318, -19.87745396966068157, 49.52966884056656482 ) ) ;
#3189 = ORIENTED_EDGE ( 'NONE', *, *, #40961, .T. ) ;
#3190 = LINE ( 'NONE', #29057, #27320 ) ;
#3191 = EDGE_CURVE ( 'NONE', #24967, #48035, #5864, .T. ) ;
#3192 = EDGE_CURVE ( 'NONE', #45223, #28690, #9572, .T. ) ;
#3193 = SHAPE_REPRESENTATION_RELATIONSHIP ( 'NONE' , 'NONE' ,  #11272, #48464 ) ;
#3194 = AXIS2_PLACEMENT_3D ( 'NONE', #30568, #11591, #37930 ) ;
#3195 = CARTESIAN_POINT ( 'NONE',  ( -19.92409385541305866, -14.80920654474411080, 75.49999999999998579 ) ) ;
#3196 = CARTESIAN_POINT ( 'NONE',  ( -13.57788044043476461, -8.959030902765807269, 60.66780251997597873 ) ) ;
#3197 = ORIENTED_EDGE ( 'NONE', *, *, #37500, .F. ) ;
#3198 = EDGE_CURVE ( 'NONE', #8796, #35282, #41543, .T. ) ;
#3199 = EDGE_CURVE ( 'NONE', #18527, #28383, #21124, .T. ) ;
#3200 = ORIENTED_EDGE ( 'NONE', *, *, #45025, .F. ) ;
#3201 = CARTESIAN_POINT ( 'NONE',  ( -11.46044050272623416, -11.04924139602722200, 57.20903212151935691 ) ) ;
#3202 = FILL_AREA_STYLE ('',( #18451 ) ) ;
#3203 = ADVANCED_FACE ( 'NONE', ( #43297 ), #18051, .T. ) ;
#3204 = DIRECTION ( 'NONE',  ( -1.000000000000000000, 0.000000000000000000, 0.000000000000000000 ) ) ;
#3205 = LINE ( 'NONE', #32751, #31154 ) ;
#3206 = AXIS2_PLACEMENT_3D ( 'NONE', #13898, #33092, #28940 ) ;
#3207 = ORIENTED_EDGE ( 'NONE', *, *, #41461, .F. ) ;
#3208 = CARTESIAN_POINT ( 'NONE',  ( -50.42609385541305755, -14.80920654474425291, 71.98235294117645822 ) ) ;
#3209 = CARTESIAN_POINT ( 'NONE',  ( -23.79049241923990721, -17.71949969818489379, 59.01880874247220987 ) ) ;
#3210 = EDGE_CURVE ( 'NONE', #26240, #37436, #40721, .T. ) ;
#3211 = ORIENTED_EDGE ( 'NONE', *, *, #39961, .T. ) ;
#3212 = CARTESIAN_POINT ( 'NONE',  ( -22.38280345442485242, -20.36932031849321589, 62.27793240076999126 ) ) ;
#3213 = CARTESIAN_POINT ( 'NONE',  ( -19.77436091090941517, -21.87886160397694368, 65.64981624214608757 ) ) ;
#3214 = DIRECTION ( 'NONE',  ( 1.000000000000000000, 2.866981220435666553E-17, 0.000000000000000000 ) ) ;
#3215 = ORIENTED_EDGE ( 'NONE', *, *, #16956, .T. ) ;
#3216 = DIRECTION ( 'NONE',  ( 0.8467008005855415353, -0.3141239757129648535, 0.4294460177601879258 ) ) ;
#3217 = ORIENTED_EDGE ( 'NONE', *, *, #47720, .F. ) ;
#3218 = CARTESIAN_POINT ( 'NONE',  ( -23.78282461406436710, -10.92707771475091150, 73.53910168191997343 ) ) ;
#3220 = FACE_OUTER_BOUND ( 'NONE', #9750, .T. ) ;
#3219 = AXIS2_PLACEMENT_3D ( 'NONE', #25851, #22167, #29797 ) ;
#3221 = B_SPLINE_CURVE_WITH_KNOTS ( 'NONE', 3,
 ( #32464, #3142, #36377, #33160, #2889, #2659, #48197, #17895, #32921, #40559 ),
 .UNSPECIFIED., .F., .F.,
 ( 4, 2, 2, 2, 4 ),
 ( 0.6272669072877943286, 0.7522669073073021684, 0.8772669073268100082, 1.002266907346317737, 1.127266907365825688 ),
 .UNSPECIFIED. ) ;
#3222 = ORIENTED_EDGE ( 'NONE', *, *, #1885, .T. ) ;
#3223 = CARTESIAN_POINT ( 'NONE',  ( -16.26195973558533581, -21.76306465430365122, 58.57113428431811997 ) ) ;
#3224 = CARTESIAN_POINT ( 'NONE',  ( -10.27391136003569905, -12.71670657087258327, 64.31190181376453552 ) ) ;
#3225 = CARTESIAN_POINT ( 'NONE',  ( -22.04909385650551457, -8.104110260919577868, 48.81699501597546487 ) ) ;
#3226 = AXIS2_PLACEMENT_3D ( 'NONE', #40066, #17639, #22564 ) ;
#3227 = CARTESIAN_POINT ( 'NONE',  ( -12.85925802207596114, -13.69662874518197171, 49.52966884056655772 ) ) ;
#3228 = CARTESIAN_POINT ( 'NONE',  ( -23.74985771237617627, -17.93965049410213197, 62.61793715156320417 ) ) ;
#3229 = FACE_OUTER_BOUND ( 'NONE', #21351, .T. ) ;
#3230 = CARTESIAN_POINT ( 'NONE',  ( -45.55409385541306477, -14.20920654474410760, 70.91501325280044910 ) ) ;
#3231 = EDGE_LOOP ( 'NONE', ( #25717, #29584, #23934, #15651 ) ) ;
#3232 = AXIS2_PLACEMENT_3D ( 'NONE', #3704, #20, #15003 ) ;
#3233 = CARTESIAN_POINT ( 'NONE',  ( -24.46146587544552276, -14.38248120490118609, 66.46820668217904426 ) ) ;
#3234 = FACE_OUTER_BOUND ( 'NONE', #10450, .T. ) ;
#3235 = FACE_OUTER_BOUND ( 'NONE', #13514, .T. ) ;
#3236 = CARTESIAN_POINT ( 'NONE',  ( -13.82836502510361854, -20.88256612802230450, 61.67213144371572042 ) ) ;
#3237 = LINE ( 'NONE', #36236, #20365 ) ;
#3238 = CARTESIAN_POINT ( 'NONE',  ( -41.66527032600129843, -14.90920654474423124, 69.07058823529411029 ) ) ;
#3239 = ORIENTED_EDGE ( 'NONE', *, *, #45854, .T. ) ;
#3240 = ORIENTED_EDGE ( 'NONE', *, *, #27152, .F. ) ;
#3241 = CARTESIAN_POINT ( 'NONE',  ( 23.52590614458706852, 1.890747609047893185, 50.53028072113869484 ) ) ;
#3242 = CARTESIAN_POINT ( 'NONE',  ( -20.98579777188748707, -20.83533835786949950, 65.58453944793343737 ) ) ;
#3243 = ORIENTED_EDGE ( 'NONE', *, *, #6757, .F. ) ;
#3245 = DIRECTION ( 'NONE',  ( 0.9180681052388950381, -0.3964226963016435068, 0.000000000000000000 ) ) ;
#3244 = CARTESIAN_POINT ( 'NONE',  ( -14.72778380697628187, -21.32322314059345558, 58.16617885012796307 ) ) ;
#3246 = CIRCLE ( 'NONE', #48063, 0.2400000000000006295 ) ;
#3247 = CARTESIAN_POINT ( 'NONE',  ( -24.17271927670314113, -12.95015993349377048, 66.30246741691458112 ) ) ;
#3248 = CARTESIAN_POINT ( 'NONE',  ( -12.36648897341435749, -9.886239853951966694, 64.17347106801278755 ) ) ;
#3249 = CARTESIAN_POINT ( 'NONE',  ( -14.53767063111817137, -21.24453063237525541, 58.58106478802027084 ) ) ;
#3250 =( BOUNDED_CURVE ( )  B_SPLINE_CURVE ( 3, ( #46075, #8901, #31541, #22960 ),
 .UNSPECIFIED., .F., .F. ) 
 B_SPLINE_CURVE_WITH_KNOTS ( ( 4, 4 ),
 ( 0.9074455897393663983, 1.000000000000000000 ),
 .UNSPECIFIED. ) 
 CURVE ( )  GEOMETRIC_REPRESENTATION_ITEM ( )  RATIONAL_B_SPLINE_CURVE ( ( 0.6983129098261016132, 0.7760317562607056407, 0.8765941196520050660, 1.000000000000000000 ) ) 
 REPRESENTATION_ITEM ( '' )  );
#3251 = CARTESIAN_POINT ( 'NONE',  ( -22.07016944540107062, -20.11663773636943731, 66.00421750868065374 ) ) ;
#3252 = LINE ( 'NONE', #2534, #14451 ) ;
#3253 = DIRECTION ( 'NONE',  ( 2.846534188916127659E-06, 1.189262794724463340E-05, 0.9999999999252312533 ) ) ;
#3254 = CARTESIAN_POINT ( 'NONE',  ( -22.51726279860821833, -19.68384809141796765, 72.64400547081167758 ) ) ;
#3255 = ADVANCED_FACE ( 'NONE', ( #42808 ), #9082, .T. ) ;
#3256 = VERTEX_POINT ( 'NONE', #17652 ) ;
#3257 = FACE_OUTER_BOUND ( 'NONE', #18674, .T. ) ;
#3258 = DIRECTION ( 'NONE',  ( 1.224646799147353207E-16, 1.000000000000000000, -1.912410701131276611E-32 ) ) ;
#3259 = CARTESIAN_POINT ( 'NONE',  ( -16.77411572588129118, -21.83219480353551134, 72.58031927177887610 ) ) ;
#3260 = CARTESIAN_POINT ( 'NONE',  ( -11.16720114480400383, -11.56054632708127450, 67.61864607954859707 ) ) ;
#3261 = CARTESIAN_POINT ( 'NONE',  ( -24.57849813159777597, -12.72878314728456850, 66.41591366067137869 ) ) ;
#3262 = CARTESIAN_POINT ( 'NONE',  ( -13.71293330176565384, -21.26916511146244915, 68.64120417180296840 ) ) ;
#3263 =( BOUNDED_CURVE ( )  B_SPLINE_CURVE ( 3, ( #11578, #25618, #3962, #15005 ),
 .UNSPECIFIED., .F., .F. ) 
 B_SPLINE_CURVE_WITH_KNOTS ( ( 4, 4 ),
 ( 0.000000000000000000, 0.4074455897393636783 ),
 .UNSPECIFIED. ) 
 CURVE ( )  GEOMETRIC_REPRESENTATION_ITEM ( )  RATIONAL_B_SPLINE_CURVE ( ( 1.000000000000000000, 0.4567392136813336889, 0.3561768502900309330, 0.6983129098260917322 ) ) 
 REPRESENTATION_ITEM ( '' )  );
#3264 = CARTESIAN_POINT ( 'NONE',  ( -22.16605834473193326, -9.587270374048046051, 60.02171285714800320 ) ) ;
#3265 =( BOUNDED_SURFACE ( )  B_SPLINE_SURFACE ( 3, 1, ( 
 ( #7759, #38241 ),
 ( #26451, #41466 ),
 ( #22775, #27420 ),
 ( #594, #4524 ),
 ( #37766, #34069 ),
 ( #15842, #1076 ),
 ( #20036, #362 ) ),
 .UNSPECIFIED., .T., .F., .F. ) 
 B_SPLINE_SURFACE_WITH_KNOTS ( ( 4, 3, 4 ),
 ( 2, 2 ),
 ( 0.000000000000000000, 0.5000000000000000000, 1.000000000000000000 ),
 ( 0.000000000000000000, 1.000000000000000000 ),
 .UNSPECIFIED. ) 
 GEOMETRIC_REPRESENTATION_ITEM ( )  RATIONAL_B_SPLINE_SURFACE ( (
 ( 1.000000000000000000, 1.000000000000000000),
 ( 0.3333333333333335369, 0.3333333333333330373),
 ( 0.3333333333333335369, 0.3333333333333330373),
 ( 1.000000000000000000, 1.000000000000000000),
 ( 0.3333333333333333703, 0.3333333333333333703),
 ( 0.3333333333333333703, 0.3333333333333333703),
 ( 1.000000000000000000, 1.000000000000000000) ) ) 
 REPRESENTATION_ITEM ( '' )  SURFACE ( )  );
#3266 = VERTEX_POINT ( 'NONE', #14414 ) ;
#3267 = VERTEX_POINT ( 'NONE', #7333 ) ;
#3268 = CARTESIAN_POINT ( 'NONE',  ( -14.70534385541304623, -7.595227055684746986, 51.75156210489594599 ) ) ;
#3269 = ADVANCED_FACE ( 'NONE', ( #40795 ), #22091, .T. ) ;
#3270 =( GEOMETRIC_REPRESENTATION_CONTEXT ( 3 ) GLOBAL_UNCERTAINTY_ASSIGNED_CONTEXT ( ( #31222 ) ) GLOBAL_UNIT_ASSIGNED_CONTEXT ( ( #11692, #16758, #26959 ) ) REPRESENTATION_CONTEXT ( 'NONE', 'WORKASPACE' ) );
#3271 = ORIENTED_EDGE ( 'NONE', *, *, #8686, .T. ) ;
#3272 = CARTESIAN_POINT ( 'NONE',  ( -23.54137353425661061, -19.06164953464739753, 65.94672567501233118 ) ) ;
#3273 = EDGE_CURVE ( 'NONE', #37009, #33767, #33383, .T. ) ;
#3274 = CARTESIAN_POINT ( 'NONE',  ( -20.02766381537926677, -8.311286447040620473, 74.02096589762064127 ) ) ;
#3275 = EDGE_CURVE ( 'NONE', #19030, #5150, #28945, .T. ) ;
#3276 =( BOUNDED_SURFACE ( )  B_SPLINE_SURFACE ( 3, 1, ( 
 ( #1403, #1657 ),
 ( #31210, #42553 ),
 ( #15935, #42056 ),
 ( #16664, #27033 ),
 ( #8570, #34896 ),
 ( #8823, #16420 ),
 ( #12965, #46488 ) ),
 .UNSPECIFIED., .T., .F., .F. ) 
 B_SPLINE_SURFACE_WITH_KNOTS ( ( 4, 3, 4 ),
 ( 2, 2 ),
 ( 0.000000000000000000, 0.5000000000000000000, 1.000000000000000000 ),
 ( 0.000000000000000000, 1.000000000000000000 ),
 .UNSPECIFIED. ) 
 GEOMETRIC_REPRESENTATION_ITEM ( )  RATIONAL_B_SPLINE_SURFACE ( (
 ( 1.000000000000000000, 1.000000000000000000),
 ( 0.3333333333333335369, 0.3333333333333330373),
 ( 0.3333333333333335369, 0.3333333333333330373),
 ( 1.000000000000000000, 1.000000000000000000),
 ( 0.3333333333333333703, 0.3333333333333333703),
 ( 0.3333333333333333703, 0.3333333333333333703),
 ( 1.000000000000000000, 1.000000000000000000) ) ) 
 REPRESENTATION_ITEM ( '' )  SURFACE ( )  );
#3277 = CARTESIAN_POINT ( 'NONE',  ( -18.29367245688808552, -17.15309925898211674, 47.99999999999994316 ) ) ;
#3278 = CARTESIAN_POINT ( 'NONE',  ( -10.37051006938303388, -14.56035623187037942, 74.94211941000891386 ) ) ;
#3279 = ORIENTED_EDGE ( 'NONE', *, *, #9605, .F. ) ;
#3280 = DIRECTION ( 'NONE',  ( 3.071710424422018668E-17, -6.404604876783312462E-16, -1.000000000000000000 ) ) ;
#3281 = VECTOR ( 'NONE', #9714, 1000.000000000000227 ) ;
#3282 = CARTESIAN_POINT ( 'NONE',  ( -22.48940708121607202, -20.36508298871479283, 53.76227901944322696 ) ) ;
#3283 = VERTEX_POINT ( 'NONE', #3368 ) ;
#3284 = CARTESIAN_POINT ( 'NONE',  ( -24.66730449611544529, -13.06573935865489844, 62.94768786448354092 ) ) ;
#3285 = LINE ( 'NONE', #29626, #22008 ) ;
#3286 = ORIENTED_EDGE ( 'NONE', *, *, #36696, .T. ) ;
#3287 = DIRECTION ( 'NONE',  ( -5.215802026392426595E-06, 6.671378403414619972E-06, 0.9999999999641440152 ) ) ;
#3288 = CARTESIAN_POINT ( 'NONE',  ( -15.06268261486706983, -8.219072439155830523, 56.86616596445847449 ) ) ;
#3289 = ORIENTED_EDGE ( 'NONE', *, *, #27097, .T. ) ;
#3290 = CARTESIAN_POINT ( 'NONE',  ( -11.96654139922548232, -19.88064104245263408, 58.04869629833985556 ) ) ;
#3291 = AXIS2_PLACEMENT_3D ( 'NONE', #17017, #17514, #28126 ) ;
#3292 = CARTESIAN_POINT ( 'NONE',  ( -24.44055745662519641, -14.11932379769929113, 73.13743607903229815 ) ) ;
#3293 = LINE ( 'NONE', #30142, #44747 ) ;
#3294 = CARTESIAN_POINT ( 'NONE',  ( -21.89264518680100835, -20.26253109894388160, 58.77915004610762395 ) ) ;
#3295 = ORIENTED_EDGE ( 'NONE', *, *, #21753, .F. ) ;
#3296 = DIRECTION ( 'NONE',  ( -1.000000000000000000, -2.866981220435666553E-17, -0.000000000000000000 ) ) ;
#3297 = DIRECTION ( 'NONE',  ( -0.5351595679979678222, -0.8447509909909716175, 0.000000000000000000 ) ) ;
#3298 = CARTESIAN_POINT ( 'NONE',  ( -16.68462913526379765, -22.29107483173095261, 53.76227901944321275 ) ) ;
#3299 = CARTESIAN_POINT ( 'NONE',  ( -21.96159385650551599, -9.295667164867525756, 49.30633214617472504 ) ) ;
#3300 = ORIENTED_EDGE ( 'NONE', *, *, #22565, .T. ) ;
#3301 = CARTESIAN_POINT ( 'NONE',  ( -24.25486363958986757, -13.06355980472538292, 63.11792038370487035 ) ) ;
#3302 = CARTESIAN_POINT ( 'NONE',  ( -19.04501905262167227, -19.80271247795941392, 52.02966884056656482 ) ) ;
#3303 = VERTEX_POINT ( 'NONE', #36592 ) ;
#3304 = DIRECTION ( 'NONE',  ( -0.3478314405900308492, -0.9375570856950864451, 0.000000000000000000 ) ) ;
#3305 = CARTESIAN_POINT ( 'NONE',  ( -21.82409385759798681, -9.359200813967568422, 50.49621490985803263 ) ) ;
#3306 = FACE_OUTER_BOUND ( 'NONE', #44471, .T. ) ;
#3307 = EDGE_CURVE ( 'NONE', #39007, #38050, #6825, .T. ) ;
#3308 = B_SPLINE_CURVE_WITH_KNOTS ( 'NONE', 3,
 ( #28783, #13506, #9609, #43575, #25572, #24621, #40577, #33181, #40350, #2674 ),
 .UNSPECIFIED., .F., .F.,
 ( 4, 2, 2, 2, 4 ),
 ( 0.000000000000000000, 0.2500000000000000000, 0.5000000000000000000, 0.7500000000000000000, 1.000000000000000000 ),
 .UNSPECIFIED. ) ;
#3309 = EDGE_LOOP ( 'NONE', ( #41914, #13118, #27432, #24464, #23819 ) ) ;
#3310 = CARTESIAN_POINT ( 'NONE',  ( -19.96994565995125015, -21.32983830779690848, 72.70478737306767414 ) ) ;
#3311 = ORIENTED_EDGE ( 'NONE', *, *, #42007, .T. ) ;
#3312 = ORIENTED_EDGE ( 'NONE', *, *, #25292, .T. ) ;
#3313 = EDGE_LOOP ( 'NONE', ( #7667, #1305, #8375, #45381 ) ) ;
#3314 = CARTESIAN_POINT ( 'NONE',  ( -13.46784385650551741, -6.428312510596451368, 51.20221977374900035 ) ) ;
#3315 = CARTESIAN_POINT ( 'NONE',  ( -11.18734459328334907, -11.50497870355291319, 60.83452645039198359 ) ) ;
#3316 = DIRECTION ( 'NONE',  ( 1.011289380940303784E-05, -7.260693215641691253E-06, 0.9999999999225058778 ) ) ;
#3317 = DIRECTION ( 'NONE',  ( -0.9687793358424822143, 0.2479245821708672415, 0.000000000000000000 ) ) ;
#3318 = CARTESIAN_POINT ( 'NONE',  ( -13.24261710015883864, -8.643249176123326549, 60.55454998173587455 ) ) ;
#3319 = ORIENTED_EDGE ( 'NONE', *, *, #26112, .F. ) ;
#3320 = ORIENTED_EDGE ( 'NONE', *, *, #42961, .T. ) ;
#3321 = CARTESIAN_POINT ( 'NONE',  ( -13.83659385650551776, -6.915538690918075382, 49.31353937987644542 ) ) ;
#3322 = EDGE_CURVE ( 'NONE', #1165, #33555, #19666, .T. ) ;
#3323 = CARTESIAN_POINT ( 'NONE',  ( 18.51825960693461681, 0.6497078700089738978, 50.35886518353169095 ) ) ;
#3324 = CARTESIAN_POINT ( 'NONE',  ( -42.93585856129541156, -14.90920654474411577, 58.90588235294116970 ) ) ;
#3325 = EDGE_CURVE ( 'NONE', #6697, #24590, #11429, .T. ) ;
#3326 = CARTESIAN_POINT ( 'NONE',  ( -20.13659385650551670, -6.915538690918075382, 49.31353937987644542 ) ) ;
#3327 = VERTEX_POINT ( 'NONE', #44758 ) ;
#3328 = EDGE_CURVE ( 'NONE', #14429, #38493, #11008, .T. ) ;
#3329 = CARTESIAN_POINT ( 'NONE',  ( -10.80526167902494805, -12.38110965600595215, 57.33417096153107195 ) ) ;
#3330 = DIRECTION ( 'NONE',  ( 0.5351595679979626041, 0.8447509909909748371, 0.000000000000000000 ) ) ;
#3331 = CARTESIAN_POINT ( 'NONE',  ( -11.56806251476610115, -18.73522173559940995, 65.03234934376791898 ) ) ;
#3332 = EDGE_CURVE ( 'NONE', #17746, #11974, #25307, .T. ) ;
#3333 = VERTEX_POINT ( 'NONE', #40076 ) ;
#3334 = LINE ( 'NONE', #4321, #34343 ) ;
#3335 = EDGE_CURVE ( 'NONE', #34669, #48317, #22329, .T. ) ;
#3336 = ORIENTED_EDGE ( 'NONE', *, *, #16877, .F. ) ;
#3337 = CARTESIAN_POINT ( 'NONE',  ( -13.22529448846758804, -9.145569705956512863, 64.19474388871357462 ) ) ;
#3338 = CARTESIAN_POINT ( 'NONE',  ( -10.12334741456209208, -16.29302180943733802, 71.64761590623798782 ) ) ;
#3339 = PRESENTATION_STYLE_ASSIGNMENT (( #5661 ) ) ;
#3340 = CARTESIAN_POINT ( 'NONE',  ( -13.65110067086344792, -21.23324738024127356, 68.57129742521463811 ) ) ;
#3341 = VERTEX_POINT ( 'NONE', #3615 ) ;
#3342 = CARTESIAN_POINT ( 'NONE',  ( -18.94833981748636376, -7.977060738621439384, 66.90071832655067396 ) ) ;
#3343 = CARTESIAN_POINT ( 'NONE',  ( -24.20884359724224311, -11.73171579724705005, 59.59740298356196320 ) ) ;
#3344 =( BOUNDED_CURVE ( )  B_SPLINE_CURVE ( 3, ( #20334, #31896, #17588, #9506 ),
 .UNSPECIFIED., .F., .F. ) 
 B_SPLINE_CURVE_WITH_KNOTS ( ( 4, 4 ),
 ( 0.4074455897393596260, 0.5000000000000000000 ),
 .UNSPECIFIED. ) 
 CURVE ( )  GEOMETRIC_REPRESENTATION_ITEM ( )  RATIONAL_B_SPLINE_CURVE ( ( 0.6983129098260822953, 0.7760317562606835473, 0.8765941196519878575, 0.9999999999999914513 ) ) 
 REPRESENTATION_ITEM ( '' )  );
#3345 = CARTESIAN_POINT ( 'NONE',  ( -12.18836193727821460, -19.53083876418623532, 57.94154444592973618 ) ) ;
#3346 = CARTESIAN_POINT ( 'NONE',  ( -10.07807850977444097, -16.05059584699720432, 68.13914376727996114 ) ) ;
#3347 = ORIENTED_EDGE ( 'NONE', *, *, #21881, .T. ) ;
#3348 = CARTESIAN_POINT ( 'NONE',  ( -10.37459419693011853, -14.72189344584419679, 71.62782694350063650 ) ) ;
#3349 = CARTESIAN_POINT ( 'NONE',  ( 18.57590614458706924, 3.149984814396892485, 50.78409494584673922 ) ) ;
#3350 = CARTESIAN_POINT ( 'NONE',  ( -17.39742543611924930, -7.759256981132186759, 67.32039592192056432 ) ) ;
#3351 = ORIENTED_EDGE ( 'NONE', *, *, #24060, .F. ) ;
#3352 = DIRECTION ( 'NONE',  ( -1.653275063147722522E-06, 1.135554159962570470E-05, 0.9999999999341591117 ) ) ;
#3353 = ORIENTED_EDGE ( 'NONE', *, *, #18963, .F. ) ;
#3354 = LINE ( 'NONE', #33130, #33658 ) ;
#3355 = CARTESIAN_POINT ( 'NONE',  ( -14.06084784944548716, -21.00867483325099982, 68.34136283933983691 ) ) ;
#3356 = CARTESIAN_POINT ( 'NONE',  ( -24.47354778464749003, -12.39902454472287197, 73.42720984402279782 ) ) ;
#3357 = CARTESIAN_POINT ( 'NONE',  ( -16.13263948075386978, -7.878200451182638453, 63.68483172840383588 ) ) ;
#3358 = ORIENTED_EDGE ( 'NONE', *, *, #3901, .T. ) ;
#3359 = DIRECTION ( 'NONE',  ( -3.071710424422018668E-17, 6.404604876783312462E-16, 1.000000000000000000 ) ) ;
#3360 = EDGE_LOOP ( 'NONE', ( #8963, #14168, #24898, #43631, #46606 ) ) ;
#3361 = CARTESIAN_POINT ( 'NONE',  ( -17.79084088774826000, -7.768752266068899459, 60.08060768310445354 ) ) ;
#3362 = EDGE_CURVE ( 'NONE', #39489, #13083, #27262, .T. ) ;
#3363 = ORIENTED_EDGE ( 'NONE', *, *, #1246, .T. ) ;
#3364 = CARTESIAN_POINT ( 'NONE',  ( -10.76785811675247118, -12.48515291162924434, 57.61385273545094066 ) ) ;
#3365 = CARTESIAN_POINT ( 'NONE',  ( -13.47672066442975236, -20.59013050379473952, 58.06152457431510072 ) ) ;
#3366 = VERTEX_POINT ( 'NONE', #36363 ) ;
#3367 = ORIENTED_EDGE ( 'NONE', *, *, #28770, .T. ) ;
#3368 = CARTESIAN_POINT ( 'NONE',  ( -16.78341213209640159, -22.23169296657789928, 68.88056055876903372 ) ) ;
#3369 = CARTESIAN_POINT ( 'NONE',  ( -18.31357888663954725, -21.80286911112441572, 69.11514702303101387 ) ) ;
#3370 = CARTESIAN_POINT ( 'NONE',  ( -23.43824811396329011, -19.20609618851374023, 62.45432639691269117 ) ) ;
#3371 = FACE_OUTER_BOUND ( 'NONE', #34261, .T. ) ;
#3372 = CARTESIAN_POINT ( 'NONE',  ( -23.73684003905821527, -18.76684476618103403, 72.95023626440647035 ) ) ;
#3373 = CARTESIAN_POINT ( 'NONE',  ( -14.06695675121984301, -8.606427752881131710, 70.61468953885895417 ) ) ;
#3374 = ADVANCED_FACE ( 'NONE', ( #2644 ), #11452, .T. ) ;
#3375 = CARTESIAN_POINT ( 'NONE',  ( -14.81397530905920235, -21.78719282451566386, 61.79633834696925732 ) ) ;
#3376 = VERTEX_POINT ( 'NONE', #37831 ) ;
#3377 = ORIENTED_EDGE ( 'NONE', *, *, #39188, .T. ) ;
#3378 = DIRECTION ( 'NONE',  ( -0.000000000000000000, 1.000000000000000000, -0.000000000000000000 ) ) ;
#3379 = B_SPLINE_CURVE_WITH_KNOTS ( 'NONE', 3,
 ( #36277, #39738, #9717, #29139, #28892, #43448, #2560, #13127, #43941, #44190 ),
 .UNSPECIFIED., .F., .F.,
 ( 4, 2, 2, 2, 4 ),
 ( 0.1272669073658177219, 0.2522669073463039702, 0.3772669073267902462, 0.5022669073072765222, 0.6272669072877627983 ),
 .UNSPECIFIED. ) ;
#3380 = CARTESIAN_POINT ( 'NONE',  ( -19.71801720247071543, -10.72249662993225883, 52.02966884056656482 ) ) ;
#3381 = CARTESIAN_POINT ( 'NONE',  ( -35.42409385541304800, -8.109206544743658540, 50.50000000000030553 ) ) ;
#3382 = DIRECTION ( 'NONE',  ( -0.3722980621098836984, -0.2477784351981131006, 0.8944271909999157444 ) ) ;
#3383 = VERTEX_POINT ( 'NONE', #41785 ) ;
#3384 = CARTESIAN_POINT ( 'NONE',  ( -17.74284385650551599, -8.811426318492348031, 52.18089403414751359 ) ) ;
#3385 = VERTEX_POINT ( 'NONE', #33630 ) ;
#3386 = EDGE_CURVE ( 'NONE', #21212, #29021, #3761, .T. ) ;
#3387 = CARTESIAN_POINT ( 'NONE',  ( -24.34625376782045336, -15.85315735139701587, 69.54924175052593682 ) ) ;
#3388 = CARTESIAN_POINT ( 'NONE',  ( -12.27604185553471616, -19.62628656662749549, 58.21210303282668264 ) ) ;
#3389 = CIRCLE ( 'NONE', #33237, 1.999999999999999112 ) ;
#3390 = EDGE_CURVE ( 'NONE', #39596, #18661, #11491, .T. ) ;
#3391 = CARTESIAN_POINT ( 'NONE',  ( -17.61266704711333375, -10.12650194148654137, 52.02966884056656482 ) ) ;
#3392 = EDGE_CURVE ( 'NONE', #47884, #9803, #13878, .T. ) ;
#3393 =( BOUNDED_CURVE ( )  B_SPLINE_CURVE ( 3, ( #6132, #32479, #2903, #6618 ),
 .UNSPECIFIED., .F., .F. ) 
 B_SPLINE_CURVE_WITH_KNOTS ( ( 4, 4 ),
 ( 0.000000000000000000, 0.4074455897393625126 ),
 .UNSPECIFIED. ) 
 CURVE ( )  GEOMETRIC_REPRESENTATION_ITEM ( )  RATIONAL_B_SPLINE_CURVE ( ( 1.000000000000000000, 0.4567392136813230863, 0.3561768502900269917, 0.6983129098261117162 ) ) 
 REPRESENTATION_ITEM ( '' )  );
#3394 = ORIENTED_EDGE ( 'NONE', *, *, #36523, .T. ) ;
#3395 = CARTESIAN_POINT ( 'NONE',  ( -21.62175721279969665, -9.207301523296434809, 66.96149954034976304 ) ) ;
#3396 = EDGE_LOOP ( 'NONE', ( #6813, #12285, #24784, #12192, #34139 ) ) ;
#3397 = CARTESIAN_POINT ( 'NONE',  ( -10.40888626530166405, -14.10966241957602207, 60.91821293886854249 ) ) ;
#3398 = ADVANCED_FACE ( 'NONE', ( #4126 ), #19125, .F. ) ;
#3399 = CARTESIAN_POINT ( 'NONE',  ( -10.40035142239662669, -15.50347837920617167, 64.65204674534754758 ) ) ;
#3400 = VERTEX_POINT ( 'NONE', #33895 ) ;
#3401 = DIRECTION ( 'NONE',  ( 3.534154189880001717E-15, -4.519331686442879103E-31, -1.000000000000000000 ) ) ;
#3402 =( BOUNDED_CURVE ( )  B_SPLINE_CURVE ( 3, ( #44978, #48155, #28955, #48639 ),
 .UNSPECIFIED., .F., .F. ) 
 B_SPLINE_CURVE_WITH_KNOTS ( ( 4, 4 ),
 ( 0.000000000000000000, 0.4074455897393629566 ),
 .UNSPECIFIED. ) 
 CURVE ( )  GEOMETRIC_REPRESENTATION_ITEM ( )  RATIONAL_B_SPLINE_CURVE ( ( 1.000000000000000000, 0.4567392136813334114, 0.3561768502900308775, 0.6983129098260923984 ) ) 
 REPRESENTATION_ITEM ( '' )  );
#3403 = EDGE_CURVE ( 'NONE', #25120, #17121, #41534, .T. ) ;
#3404 = ORIENTED_EDGE ( 'NONE', *, *, #37848, .F. ) ;
#3405 = CARTESIAN_POINT ( 'NONE',  ( -24.47423110178408479, -14.79660573996179451, 59.53740478059303598 ) ) ;
#3406 = CARTESIAN_POINT ( 'NONE',  ( -24.87123160714014958, -14.59964084223042491, 62.89791924484052998 ) ) ;
#3407 = ORIENTED_EDGE ( 'NONE', *, *, #35110, .T. ) ;
#3408 = ADVANCED_FACE ( 'NONE', ( #7821 ), #24709, .T. ) ;
#3409 = EDGE_CURVE ( 'NONE', #47072, #26020, #12954, .T. ) ;
#3410 = CARTESIAN_POINT ( 'NONE',  ( 18.46573386768564973, 1.637040139411225059, 51.75426295951076838 ) ) ;
#3411 = DIRECTION ( 'NONE',  ( 0.5097212845717493668, -0.8603395911234852367, 0.000000000000000000 ) ) ;
#3412 = B_SPLINE_CURVE_WITH_KNOTS ( 'NONE', 1,
 ( #40751, #33100 ),
 .UNSPECIFIED., .F., .F.,
 ( 2, 2 ),
 ( 0.000000000000000000, 1.000000000000000000 ),
 .UNSPECIFIED. ) ;
#3413 = ORIENTED_EDGE ( 'NONE', *, *, #39062, .F. ) ;
#3414 = LINE ( 'NONE', #33192, #43322 ) ;
#3415 = CARTESIAN_POINT ( 'NONE',  ( -19.29727288544221864, -21.61407024248036635, 65.60919142207177401 ) ) ;
#3416 = FACE_OUTER_BOUND ( 'NONE', #40906, .T. ) ;
#3417 = ORIENTED_EDGE ( 'NONE', *, *, #2315, .T. ) ;
#3418 = CARTESIAN_POINT ( 'NONE',  ( -13.52677154722849906, -21.15855052895092214, 65.17903009207861942 ) ) ;
#3419 = CARTESIAN_POINT ( 'NONE',  ( -10.78978129071826686, -12.42417052737943095, 57.32857332104951098 ) ) ;
#3420 = CARTESIAN_POINT ( 'NONE',  ( -24.72409385541305582, -14.90920654474427565, 73.99411764705880046 ) ) ;
#3421 = CIRCLE ( 'NONE', #19955, 4.686499999999999666 ) ;
#3422 = ORIENTED_EDGE ( 'NONE', *, *, #45348, .F. ) ;
#3423 = VERTEX_POINT ( 'NONE', #27982 ) ;
#3424 = CARTESIAN_POINT ( 'NONE',  ( -22.93742361178516731, -14.77499336254049922, 53.69233794759168887 ) ) ;
#3425 = DIRECTION ( 'NONE',  ( -0.003782665018460030538, -0.9999928456970870183, -9.532993539451315208E-09 ) ) ;
#3426 = CARTESIAN_POINT ( 'NONE',  ( -23.48344415125163565, -18.41350569598871090, 73.04896097104848707 ) ) ;
#3427 = CARTESIAN_POINT ( 'NONE',  ( -15.97409385759799072, -6.859212275519751323, 50.50378509014259265 ) ) ;
#3428 = DIRECTION ( 'NONE',  ( -0.7150252244155714809, 0.6990986543038555379, -2.983336731533474947E-17 ) ) ;
#3429 = DIRECTION ( 'NONE',  ( 0.000000000000000000, 0.007114381193220381018, -0.9999746924698831307 ) ) ;
#3430 = B_SPLINE_CURVE_WITH_KNOTS ( 'NONE', 3,
 ( #37914, #14999, #10603, #44580, #48258, #14496, #10840, #29552, #3446, #25860 ),
 .UNSPECIFIED., .F., .F.,
 ( 4, 2, 2, 2, 4 ),
 ( 0.6272669072877681273, 0.7522669073072665302, 0.8772669073267648221, 1.002266907346263114, 1.127266907365761517 ),
 .UNSPECIFIED. ) ;
#3431 = CARTESIAN_POINT ( 'NONE',  ( -14.34284385759798930, -7.587656875400192291, 49.25157356644813689 ) ) ;
#3432 = CARTESIAN_POINT ( 'NONE',  ( -14.62687775177895766, -8.392386291203132842, 63.78978840643812021 ) ) ;
#3433 = ORIENTED_EDGE ( 'NONE', *, *, #41305, .F. ) ;
#3434 = DIRECTION ( 'NONE',  ( 0.9640890753730593232, -0.2655790932026004803, 6.310348465037888425E-08 ) ) ;
#3435 = EDGE_CURVE ( 'NONE', #28807, #21655, #21535, .T. ) ;
#3436 = CARTESIAN_POINT ( 'NONE',  ( -17.63665770386090514, -10.11555421891856099, 49.52966884056655772 ) ) ;
#3437 = CARTESIAN_POINT ( 'NONE',  ( -12.10599200002982556, -20.02663609087960239, 61.58174067880212021 ) ) ;
#3438 = ORIENTED_EDGE ( 'NONE', *, *, #2290, .F. ) ;
#3439 = ORIENTED_EDGE ( 'NONE', *, *, #5687, .F. ) ;
#3440 = EDGE_CURVE ( 'NONE', #14812, #9213, #20235, .T. ) ;
#3441 = DIRECTION ( 'NONE',  ( -0.9345716196833626643, 0.3557750520798445559, 2.412542607589989711E-09 ) ) ;
#3442 = CARTESIAN_POINT ( 'NONE',  ( -24.45422819554991278, -14.24171526414585287, 66.06804100909725719 ) ) ;
#3443 = DIRECTION ( 'NONE',  ( 3.413470714839332458E-33, -1.190614954331866791E-16, 1.000000000000000000 ) ) ;
#3444 = CARTESIAN_POINT ( 'NONE',  ( -11.68391713028079515, -10.70246380009546527, 71.12460117624890188 ) ) ;
#3445 = EDGE_LOOP ( 'NONE', ( #42413, #47423 ) ) ;
#3446 = CARTESIAN_POINT ( 'NONE',  ( -24.49392389907278655, -12.45956950672031738, 73.34951415186112911 ) ) ;
#3447 = VECTOR ( 'NONE', #36524, 1000.000000000000000 ) ;
#3448 = B_SPLINE_CURVE_WITH_KNOTS ( 'NONE', 1,
 ( #48618, #26461 ),
 .UNSPECIFIED., .F., .F.,
 ( 2, 2 ),
 ( 0.000000000000000000, 1.000000000000000000 ),
 .UNSPECIFIED. ) ;
#3449 = TOROIDAL_SURFACE ( 'NONE', #16811, 1.000000000000001332, 0.5000000000000000000 ) ;
#3450 = VERTEX_POINT ( 'NONE', #23583 ) ;
#3451 = CARTESIAN_POINT ( 'NONE',  ( -16.16748626245079379, -22.20318634978239203, 47.99999999999994316 ) ) ;
#3452 = CARTESIAN_POINT ( 'NONE',  ( -13.60236376389480384, -20.73382277062339085, 61.80174179654961364 ) ) ;
#3453 = CARTESIAN_POINT ( 'NONE',  ( -10.82872618853034119, -17.15944597561106377, 64.81666377234489573 ) ) ;
#3454 = VERTEX_POINT ( 'NONE', #16886 ) ;
#3455 = CARTESIAN_POINT ( 'NONE',  ( -12.20309502476489882, -20.12380431889209831, 64.98179558605960437 ) ) ;
#3456 = ORIENTED_EDGE ( 'NONE', *, *, #1423, .F. ) ;
#3457 = CARTESIAN_POINT ( 'NONE',  ( -23.78315586890771982, -10.92762747184599625, 73.48380518477267742 ) ) ;
#3458 = ORIENTED_EDGE ( 'NONE', *, *, #39803, .F. ) ;
#3459 = LINE ( 'NONE', #28842, #27022 ) ;
#3460 = ADVANCED_FACE ( 'NONE', ( #16158 ), #24557, .T. ) ;
#3461 = EDGE_CURVE ( 'NONE', #15544, #20590, #26704, .T. ) ;
#3462 = DIRECTION ( 'NONE',  ( 0.9904243694481097426, 0.1380563957348939774, 6.973877024228147881E-08 ) ) ;
#3463 = CARTESIAN_POINT ( 'NONE',  ( -20.36159385650551812, -9.295667164867525756, 49.30633214617472504 ) ) ;
#3464 = CARTESIAN_POINT ( 'NONE',  ( -14.44809130310161471, -8.473323905341505480, 67.25975083863336579 ) ) ;
#3465 = CARTESIAN_POINT ( 'NONE',  ( -24.46146587544552276, -14.38248120490118787, 66.46820668217904426 ) ) ;
#3466 = CARTESIAN_POINT ( 'NONE',  ( -16.98027701540031487, -7.372437998827603423, 74.11018272214712965 ) ) ;
#3467 = CARTESIAN_POINT ( 'NONE',  ( -21.94239094699587511, -20.22099839777041907, 58.91442899523080001 ) ) ;
#3468 = ORIENTED_EDGE ( 'NONE', *, *, #4108, .F. ) ;
#3469 = CARTESIAN_POINT ( 'NONE',  ( -16.98991614605047218, -22.24663000551990777, 72.35038637723081933 ) ) ;
#3470 = CARTESIAN_POINT ( 'NONE',  ( -18.71756812234623979, -7.929749856837892352, 70.67068030594712980 ) ) ;
#3471 = CARTESIAN_POINT ( 'NONE',  ( -22.93140599106849464, -9.791786736557840598, 70.15032017024104505 ) ) ;
#3472 = EDGE_CURVE ( 'NONE', #12455, #16401, #16233, .T. ) ;
#3473 = ADVANCED_FACE ( 'NONE', ( #12730 ), #31201, .T. ) ;
#3474 = CARTESIAN_POINT ( 'NONE',  ( 10.57590614458695377, 1.890747609047612521, 50.53028072113853142 ) ) ;
#3475 = CARTESIAN_POINT ( 'NONE',  ( -16.40075914357782949, -21.78757426832101274, 58.17096681542334835 ) ) ;
#3476 = LINE ( 'NONE', #45114, #3564 ) ;
#3477 = VERTEX_POINT ( 'NONE', #39065 ) ;
#3478 = ORIENTED_EDGE ( 'NONE', *, *, #38491, .T. ) ;
#3479 = CARTESIAN_POINT ( 'NONE',  ( -15.03427660820159772, -21.44211488324610571, 65.12068745241758450 ) ) ;
#3480 = CARTESIAN_POINT ( 'NONE',  ( -14.84921296472849583, -8.299983211734243582, 56.95852036331775281 ) ) ;
#3481 = ORIENTED_EDGE ( 'NONE', *, *, #10775, .F. ) ;
#3483 = DIRECTION ( 'NONE',  ( 1.224646799147353207E-16, 1.000000000000000000, -1.912410701131276611E-32 ) ) ;
#3482 = CARTESIAN_POINT ( 'NONE',  ( -14.66790711817407278, -21.29843871104708342, 58.18089935161520287 ) ) ;
#3484 = CYLINDRICAL_SURFACE ( 'NONE', #46347, 0.1500000000000049349 ) ;
#3485 = CARTESIAN_POINT ( 'NONE',  ( -14.09463846823036981, -8.088735815341543400, 47.99999999999994316 ) ) ;
#3486 = CARTESIAN_POINT ( 'NONE',  ( -24.38391081516821401, -14.06024225110868464, 73.12271507915593816 ) ) ;
#3487 = CARTESIAN_POINT ( 'NONE',  ( -11.41081668282658157, -19.20748171390168579, 71.86498669792840133 ) ) ;
#3488 = CARTESIAN_POINT ( 'NONE',  ( -24.45670955521185164, -12.20012290887857098, 53.49999999999995026 ) ) ;
#3489 = AXIS2_PLACEMENT_3D ( 'NONE', #13287, #28581, #28341 ) ;
#3490 = CARTESIAN_POINT ( 'NONE',  ( -16.71068108117115969, -21.77319771387776726, 68.97944111337483264 ) ) ;
#3491 = EDGE_CURVE ( 'NONE', #7972, #33406, #40361, .T. ) ;
#3492 = ORIENTED_EDGE ( 'NONE', *, *, #16356, .T. ) ;
#3493 = VECTOR ( 'NONE', #31047, 1000.000000000000227 ) ;
#3494 = CYLINDRICAL_SURFACE ( 'NONE', #31398, 7.500000000000001776 ) ;
#3495 = CARTESIAN_POINT ( 'NONE',  ( -11.49054114279358885, -18.52332417048542013, 61.57710786629046140 ) ) ;
#3496 = CARTESIAN_POINT ( 'NONE',  ( -15.52409385759799143, -9.359200813967568422, 50.49621490985803263 ) ) ;
#3497 = CARTESIAN_POINT ( 'NONE',  ( -24.26595263201846109, -13.32969024507516309, 59.66267925069213618 ) ) ;
#3498 = CARTESIAN_POINT ( 'NONE',  ( -12.10131192688100477, -10.18592936015514638, 64.31442259820508411 ) ) ;
#3499 = PLANE ( 'NONE',  #36194 ) ;
#3500 = CARTESIAN_POINT ( 'NONE',  ( -18.19230087906959170, -22.21957251972233749, 65.38886231616686473 ) ) ;
#3501 = VERTEX_POINT ( 'NONE', #16656 ) ;
#3502 = VERTEX_POINT ( 'NONE', #34885 ) ;
#3503 = CARTESIAN_POINT ( 'NONE',  ( -13.63659385541304481, -8.995762431863214559, 51.38120296130585274 ) ) ;
#3504 = ORIENTED_EDGE ( 'NONE', *, *, #33188, .F. ) ;
#3505 = CARTESIAN_POINT ( 'NONE',  ( -23.53756504580003650, -19.06719683152477174, 65.96356102755147788 ) ) ;
#3506 = CARTESIAN_POINT ( 'NONE',  ( -10.42302287260171312, -13.97751933429587012, 57.73352905910142852 ) ) ;
#3507 = CARTESIAN_POINT ( 'NONE',  ( -15.70814931713893792, -7.971180294065260519, 70.60989868072361730 ) ) ;
#3508 = CARTESIAN_POINT ( 'NONE',  ( -15.56003183875577278, -7.596127455810019136, 70.71651511567537796 ) ) ;
#3509 = ORIENTED_EDGE ( 'NONE', *, *, #24161, .T. ) ;
#3510 = B_SPLINE_CURVE_WITH_KNOTS ( 'NONE', 1,
 ( #9490, #39513 ),
 .UNSPECIFIED., .F., .F.,
 ( 2, 2 ),
 ( 0.000000000000000000, 1.000000000000000000 ),
 .UNSPECIFIED. ) ;
#3511 = CARTESIAN_POINT ( 'NONE',  ( -23.13029420580725315, -10.01925251292537489, 66.66465368338731423 ) ) ;
#3512 = DIRECTION ( 'NONE',  ( -0.1847813031241906379, 0.9827796650397889744, -7.910442904995767160E-08 ) ) ;
#3513 = ORIENTED_EDGE ( 'NONE', *, *, #20645, .F. ) ;
#3514 = CARTESIAN_POINT ( 'NONE',  ( -46.47622156840087371, -14.20920654474410760, 70.13000000000000966 ) ) ;
#3515 = B_SPLINE_CURVE_WITH_KNOTS ( 'NONE', 1,
 ( #11785, #3653 ),
 .UNSPECIFIED., .F., .F.,
 ( 2, 2 ),
 ( 0.000000000000000000, 1.000000000000000000 ),
 .UNSPECIFIED. ) ;
#3516 = CARTESIAN_POINT ( 'NONE',  ( -24.35706328060247827, -15.77560928887050373, 69.53307488759497801 ) ) ;
#3517 = AXIS2_PLACEMENT_3D ( 'NONE', #32216, #35882, #2163 ) ;
#3518 = ORIENTED_EDGE ( 'NONE', *, *, #22100, .T. ) ;
#3519 = CARTESIAN_POINT ( 'NONE',  ( -10.98611580423108336, -17.68970554115635352, 67.98233349607527032 ) ) ;
#3520 = DIRECTION ( 'NONE',  ( -3.071710424422018668E-17, 6.404604876783312462E-16, 1.000000000000000000 ) ) ;
#3521 = CARTESIAN_POINT ( 'NONE',  ( -23.24618082141521214, -10.81943526098172548, 59.74636554153219237 ) ) ;
#3522 = ORIENTED_EDGE ( 'NONE', *, *, #41529, .T. ) ;
#3523 = CARTESIAN_POINT ( 'NONE',  ( -10.73343087151675590, -11.53221169192942597, 71.34506790255136366 ) ) ;
#3524 = EDGE_CURVE ( 'NONE', #29406, #22557, #4370, .T. ) ;
#3525 = AXIS2_PLACEMENT_3D ( 'NONE', #12335, #7692, #3989 ) ;
#3526 = LINE ( 'NONE', #7983, #41488 ) ;
#3527 =( BOUNDED_CURVE ( )  B_SPLINE_CURVE ( 3, ( #12326, #31772, #5912, #23911 ),
 .UNSPECIFIED., .F., .F. ) 
 B_SPLINE_CURVE_WITH_KNOTS ( ( 4, 4 ),
 ( 0.9074455897393642889, 1.000000000000000000 ),
 .UNSPECIFIED. ) 
 CURVE ( )  GEOMETRIC_REPRESENTATION_ITEM ( )  RATIONAL_B_SPLINE_CURVE ( ( 0.6983129098260905110, 0.7760317562606959818, 0.8765941196519991818, 1.000000000000000000 ) ) 
 REPRESENTATION_ITEM ( '' )  );
#3528 = CARTESIAN_POINT ( 'NONE',  ( -24.72409385541305582, -14.90920654474428630, 74.99999999999998579 ) ) ;
#3529 = CARTESIAN_POINT ( 'NONE',  ( -23.96395177782270380, -17.30542690858300503, 66.17030669039861834 ) ) ;
#3530 = EDGE_LOOP ( 'NONE', ( #38837, #3924, #30214, #38755, #4332 ) ) ;
#3531 = CARTESIAN_POINT ( 'NONE',  ( -9.979603215878100286, -14.52052451035377345, 68.04295550616701860 ) ) ;
#3532 = DIRECTION ( 'NONE',  ( -3.071710424422018668E-17, 6.404604876783312462E-16, 1.000000000000000000 ) ) ;
#3533 = DIRECTION ( 'NONE',  ( 0.3964226963016399541, 0.9180681052388965924, 0.000000000000000000 ) ) ;
#3534 = CARTESIAN_POINT ( 'NONE',  ( -17.91839958824308709, -21.79173199888728263, 61.87535923606637311 ) ) ;
#3535 = EDGE_CURVE ( 'NONE', #5056, #6304, #31687, .T. ) ;
#3536 = ADVANCED_FACE ( 'NONE', ( #46943 ), #13185, .T. ) ;
#3537 = CARTESIAN_POINT ( 'NONE',  ( -19.54284385650551670, -8.811426318492348031, 52.18089403414751359 ) ) ;
#3539 = ADVANCED_FACE ( 'NONE', ( #30971 ), #45986, .T. ) ;
#3538 = ORIENTED_EDGE ( 'NONE', *, *, #32461, .F. ) ;
#3540 = CYLINDRICAL_SURFACE ( 'NONE', #7843, 2.500000000000001332 ) ;
#3541 = CARTESIAN_POINT ( 'NONE',  ( -20.92409385759799179, -9.359200813967568422, 50.49621490985803263 ) ) ;
#3542 = ORIENTED_EDGE ( 'NONE', *, *, #35910, .T. ) ;
#3543 = CARTESIAN_POINT ( 'NONE',  ( 18.57590614458706924, 1.903197776136028807, 48.78032500931639959 ) ) ;
#3544 = EDGE_CURVE ( 'NONE', #29528, #40648, #7040, .T. ) ;
#3545 = CARTESIAN_POINT ( 'NONE',  ( -22.55199052693725648, -10.04362092364324255, 73.76544497664282574 ) ) ;
#3546 = LINE ( 'NONE', #25713, #7764 ) ;
#3547 =( BOUNDED_CURVE ( )  B_SPLINE_CURVE ( 3, ( #14512, #6925, #21945, #7924 ),
 .UNSPECIFIED., .F., .F. ) 
 B_SPLINE_CURVE_WITH_KNOTS ( ( 4, 4 ),
 ( 0.5000000000000000000, 0.9074455897393648440 ),
 .UNSPECIFIED. ) 
 CURVE ( )  GEOMETRIC_REPRESENTATION_ITEM ( )  RATIONAL_B_SPLINE_CURVE ( ( 1.000000000000029310, 0.4567392136813408499, 0.3561768502900130584, 0.6983129098260774104 ) ) 
 REPRESENTATION_ITEM ( '' )  );
#3548 = VERTEX_POINT ( 'NONE', #29200 ) ;
#3549 =( BOUNDED_CURVE ( )  B_SPLINE_CURVE ( 3, ( #23117, #4388, #38345, #15942 ),
 .UNSPECIFIED., .F., .F. ) 
 B_SPLINE_CURVE_WITH_KNOTS ( ( 4, 4 ),
 ( 0.9074455897393562953, 1.000000000000000000 ),
 .UNSPECIFIED. ) 
 CURVE ( )  GEOMETRIC_REPRESENTATION_ITEM ( )  RATIONAL_B_SPLINE_CURVE ( ( 0.6983129098260636436, 0.7760317562606728892, 0.8765941196519849710, 1.000000000000000000 ) ) 
 REPRESENTATION_ITEM ( '' )  );
#3550 = CARTESIAN_POINT ( 'NONE',  ( -46.92409385541305511, -17.80920654474410370, 61.49999999999999289 ) ) ;
#3551 = CARTESIAN_POINT ( 'NONE',  ( -23.42858231244642297, -18.40751668988569634, 73.06368185858580944 ) ) ;
#3552 = VERTEX_POINT ( 'NONE', #44240 ) ;
#3553 = ADVANCED_FACE ( 'NONE', ( #18093 ), #36799, .T. ) ;
#3554 = EDGE_LOOP ( 'NONE', ( #39142, #3633, #2694, #16363, #24608 ) ) ;
#3555 = CARTESIAN_POINT ( 'NONE',  ( -13.80534385650551776, -8.801233750844183135, 48.81488406609782515 ) ) ;
#3556 = LINE ( 'NONE', #18073, #26339 ) ;
#3557 = FACE_OUTER_BOUND ( 'NONE', #125, .T. ) ;
#3558 = CARTESIAN_POINT ( 'NONE',  ( -24.85470879995478199, -14.26980839996429040, 69.81421776232033949 ) ) ;
#3559 = CARTESIAN_POINT ( 'NONE',  ( -13.18362886651731358, -8.683667069837246899, 60.62445550483372614 ) ) ;
#3560 =( BOUNDED_SURFACE ( )  B_SPLINE_SURFACE ( 3, 1, ( 
 ( #23002, #37746 ),
 ( #15088, #15327 ),
 ( #3787, #44927 ),
 ( #36347, #22254 ),
 ( #32663, #44672 ),
 ( #30387, #22755 ),
 ( #18797, #11655 ) ),
 .UNSPECIFIED., .T., .F., .F. ) 
 B_SPLINE_SURFACE_WITH_KNOTS ( ( 4, 3, 4 ),
 ( 2, 2 ),
 ( 0.000000000000000000, 0.5000000000000000000, 1.000000000000000000 ),
 ( 0.000000000000000000, 1.000000000000000000 ),
 .UNSPECIFIED. ) 
 GEOMETRIC_REPRESENTATION_ITEM ( )  RATIONAL_B_SPLINE_SURFACE ( (
 ( 1.000000000000000000, 1.000000000000000000),
 ( 0.3333333333333335369, 0.3333333333333330373),
 ( 0.3333333333333335369, 0.3333333333333330373),
 ( 1.000000000000000000, 1.000000000000000000),
 ( 0.3333333333333333703, 0.3333333333333333703),
 ( 0.3333333333333333703, 0.3333333333333333703),
 ( 1.000000000000000000, 1.000000000000000000) ) ) 
 REPRESENTATION_ITEM ( '' )  SURFACE ( )  );
#3561 = ORIENTED_EDGE ( 'NONE', *, *, #31459, .T. ) ;
#3562 = VERTEX_POINT ( 'NONE', #10493 ) ;
#3563 = CARTESIAN_POINT ( 'NONE',  ( -15.91784385650552025, -9.790100578890868377, 49.79778022625163203 ) ) ;
#3564 = VECTOR ( 'NONE', #14522, 1000.000000000000114 ) ;
#3565 = DIRECTION ( 'NONE',  ( -3.071710424422018668E-17, 6.404604876783312462E-16, 1.000000000000000000 ) ) ;
#3566 = DIRECTION ( 'NONE',  ( -1.000000000000000000, -1.669677910507523057E-21, -6.493791346278465266E-22 ) ) ;
#3567 = CARTESIAN_POINT ( 'NONE',  ( -15.18659385650551386, -9.302874398569244363, 51.68646062012417985 ) ) ;
#3568 = ORIENTED_EDGE ( 'NONE', *, *, #41520, .F. ) ;
#3569 = FACE_OUTER_BOUND ( 'NONE', #12241, .T. ) ;
#3570 = CARTESIAN_POINT ( 'NONE',  ( -10.12326195556307695, -13.32541703369907893, 74.86313051124790263 ) ) ;
#3571 = EDGE_CURVE ( 'NONE', #29274, #42743, #35490, .T. ) ;
#3572 = ORIENTED_EDGE ( 'NONE', *, *, #36367, .T. ) ;
#3573 = DIRECTION ( 'NONE',  ( 3.071710424422018668E-17, -6.404604876783312462E-16, -1.000000000000000000 ) ) ;
#3574 = ORIENTED_EDGE ( 'NONE', *, *, #42354, .F. ) ;
#3575 = B_SPLINE_CURVE_WITH_KNOTS ( 'NONE', 3,
 ( #5186, #40588, #17932, #21888, #25347, #2454, #47993, #36888, #7129, #11060 ),
 .UNSPECIFIED., .F., .F.,
 ( 4, 2, 2, 2, 4 ),
 ( 0.6272669072877600227, 0.7522669073072842938, 0.8772669073268084539, 1.002266907346332836, 1.127266907365856996 ),
 .UNSPECIFIED. ) ;
#3576 = CARTESIAN_POINT ( 'NONE',  ( -22.27817835350360909, -9.157512823226451104, 59.83675901011532261 ) ) ;
#3577 = CARTESIAN_POINT ( 'NONE',  ( -18.15846757210552553, -21.77219414362900807, 68.92587836579659211 ) ) ;
#3578 = CARTESIAN_POINT ( 'NONE',  ( -17.42409385541300892, -14.80920654474439324, 54.49999999999995026 ) ) ;
#3579 = CARTESIAN_POINT ( 'NONE',  ( -21.53281191010185935, -21.02392799970474258, 72.70259218005269020 ) ) ;
#3580 = EDGE_CURVE ( 'NONE', #48493, #10239, #43746, .T. ) ;
#3581 = ORIENTED_EDGE ( 'NONE', *, *, #44647, .F. ) ;
#3582 = CARTESIAN_POINT ( 'NONE',  ( -17.98657259272421172, -21.83703102787368167, 62.16063850355641307 ) ) ;
#3583 = CARTESIAN_POINT ( 'NONE',  ( -24.18913222791875484, -11.68880796321081661, 59.68224518730406203 ) ) ;
#3584 = LINE ( 'NONE', #19098, #27397 ) ;
#3585 = CARTESIAN_POINT ( 'NONE',  ( -10.09291391017891115, -16.13494330055838333, 68.16263215882007387 ) ) ;
#3586 = EDGE_LOOP ( 'NONE', ( #36254, #16648, #13382, #36993, #35217 ) ) ;
#3587 = LINE ( 'NONE', #167, #7934 ) ;
#3588 = CARTESIAN_POINT ( 'NONE',  ( -17.13698961087219175, -7.364572068746518596, 70.65069232833010915 ) ) ;
#3589 = CARTESIAN_POINT ( 'NONE',  ( -17.42409385541299471, -14.80920654474435771, 49.52966884056655772 ) ) ;
#3590 = VECTOR ( 'NONE', #43857, 1000.000000000000000 ) ;
#3591 = FACE_BOUND ( 'NONE', #14029, .T. ) ;
#3592 = B_SPLINE_CURVE_WITH_KNOTS ( 'NONE', 3,
 ( #8653, #1488, #774, #30825, #23185, #30342, #19970, #11604, #41649, #12332 ),
 .UNSPECIFIED., .F., .F.,
 ( 4, 2, 2, 2, 4 ),
 ( 0.000000000000000000, 0.2500000000000000000, 0.5000000000000000000, 0.7500000000000000000, 1.000000000000000000 ),
 .UNSPECIFIED. ) ;
#3593 = ORIENTED_EDGE ( 'NONE', *, *, #39131, .F. ) ;
#3594 = CARTESIAN_POINT ( 'NONE',  ( -18.31357764725860093, -21.80286926110680668, 68.96514702303620936 ) ) ;
#3595 = CARTESIAN_POINT ( 'NONE',  ( -14.25534385541286397, -8.623186033802699768, 49.24843789510436665 ) ) ;
#3596 = CARTESIAN_POINT ( 'NONE',  ( -16.95565408849980216, -21.84366694028823730, 72.16543230909471163 ) ) ;
#3597 = ADVANCED_FACE ( 'NONE', ( #32871 ), #36555, .T. ) ;
#3598 = APPLICATION_CONTEXT ( 'automotive_design' ) ;
#3599 = B_SPLINE_CURVE_WITH_KNOTS ( 'NONE', 1,
 ( #15858, #30906 ),
 .UNSPECIFIED., .F., .F.,
 ( 2, 2 ),
 ( 0.000000000000000000, 1.000000000000000000 ),
 .UNSPECIFIED. ) ;
#3600 = CARTESIAN_POINT ( 'NONE',  ( -15.86712703025682103, -7.930203392541469221, 63.55522141739008646 ) ) ;
#3601 = ORIENTED_EDGE ( 'NONE', *, *, #34070, .T. ) ;
#3602 = CARTESIAN_POINT ( 'NONE',  ( -10.45160174785924312, -14.17496227992596580, 64.61633729656794856 ) ) ;
#3603 = EDGE_CURVE ( 'NONE', #47392, #27894, #17614, .T. ) ;
#3604 = ORIENTED_EDGE ( 'NONE', *, *, #29594, .F. ) ;
#3605 = CARTESIAN_POINT ( 'NONE',  ( -12.20772386052854408, -10.14112062039578532, 64.02914330961903033 ) ) ;
#3606 = CARTESIAN_POINT ( 'NONE',  ( -10.98437665993992596, -18.55522755060170681, 58.00703366852174980 ) ) ;
#3607 = CARTESIAN_POINT ( 'NONE',  ( -22.60922486080212934, -15.63195587288279320, 50.77966884056655772 ) ) ;
#3608 = EDGE_LOOP ( 'NONE', ( #25055, #15354, #3279, #37136, #40266 ) ) ;
#3609 = CARTESIAN_POINT ( 'NONE',  ( -21.59804090337381410, -20.98026344205569771, 72.70941702861115630 ) ) ;
#3610 = ADVANCED_FACE ( 'NONE', ( #21088 ), #21338, .T. ) ;
#3611 = CARTESIAN_POINT ( 'NONE',  ( -18.35379419424621972, -22.20097654771712570, 69.01525906027519852 ) ) ;
#3612 = ORIENTED_EDGE ( 'NONE', *, *, #7248, .F. ) ;
#3613 = ORIENTED_EDGE ( 'NONE', *, *, #16880, .T. ) ;
#3614 = ORIENTED_EDGE ( 'NONE', *, *, #43918, .F. ) ;
#3615 = CARTESIAN_POINT ( 'NONE',  ( -14.92764478915313653, -21.34891159457319532, 61.63600440564275829 ) ) ;
#3616 = CARTESIAN_POINT ( 'NONE',  ( -20.57278596605185683, -8.057205637650621810, 66.89608763938375091 ) ) ;
#3617 = CARTESIAN_POINT ( 'NONE',  ( -19.36518065869528726, -8.031383756764064685, 59.97565108339750850 ) ) ;
#3619 = EDGE_CURVE ( 'NONE', #26610, #45033, #14381, .T. ) ;
#3618 = CARTESIAN_POINT ( 'NONE',  ( -20.85039448910245241, -8.638677133180788559, 63.45554403117525055 ) ) ;
#3620 = LINE ( 'NONE', #23082, #37748 ) ;
#3621 = CARTESIAN_POINT ( 'NONE',  ( -14.43441977789444763, -8.421195553735145722, 71.14446303425738449 ) ) ;
#3622 = CARTESIAN_POINT ( 'NONE',  ( -14.74088078129247137, -21.75928990931933527, 61.74326270667029348 ) ) ;
#3623 = ORIENTED_EDGE ( 'NONE', *, *, #33387, .T. ) ;
#3624 = ORIENTED_EDGE ( 'NONE', *, *, #27377, .T. ) ;
#3625 = B_SPLINE_CURVE_WITH_KNOTS ( 'NONE', 3,
 ( #16092, #8255, #14435, #27439, #34574, #33170, #4081, #46156, #30183, #45201 ),
 .UNSPECIFIED., .F., .F.,
 ( 4, 2, 2, 2, 4 ),
 ( 0.000000000000000000, 0.2500000000000000000, 0.5000000000000000000, 0.7500000000000000000, 1.000000000000000000 ),
 .UNSPECIFIED. ) ;
#3626 = CARTESIAN_POINT ( 'NONE',  ( -16.32575768948312600, -7.844986739114469643, 60.21500614002425777 ) ) ;
#3627 = DIRECTION ( 'NONE',  ( 0.2393306345705741855, 0.3777841279832264143, 0.8944271909999157444 ) ) ;
#3628 = CARTESIAN_POINT ( 'NONE',  ( -14.90981263331598328, -21.39562362703504306, 61.93600440604522817 ) ) ;
#3629 = PLANE ( 'NONE',  #44132 ) ;
#3630 = VERTEX_POINT ( 'NONE', #17122 ) ;
#3631 = CARTESIAN_POINT ( 'NONE',  ( -15.04284385650551670, -8.811426318492348031, 52.18089403414752070 ) ) ;
#3632 = VECTOR ( 'NONE', #10931, 1000.000000000000000 ) ;
#3633 = ORIENTED_EDGE ( 'NONE', *, *, #20792, .T. ) ;
#3634 = CARTESIAN_POINT ( 'NONE',  ( -24.35164231460261064, -15.81449975624289728, 69.83307533819942137 ) ) ;
#3635 = CARTESIAN_POINT ( 'NONE',  ( -13.35550429318260512, -8.568184490765622385, 57.15463139269148485 ) ) ;
#3636 = LINE ( 'NONE', #14938, #15779 ) ;
#3637 =( BOUNDED_SURFACE ( )  B_SPLINE_SURFACE ( 3, 1, ( 
 ( #23451, #38446 ),
 ( #34763, #47311 ),
 ( #43865, #16521 ),
 ( #13297, #20717 ),
 ( #13545, #24662 ),
 ( #31557, #1763 ),
 ( #6178, #2482 ) ),
 .UNSPECIFIED., .T., .F., .F. ) 
 B_SPLINE_SURFACE_WITH_KNOTS ( ( 4, 3, 4 ),
 ( 2, 2 ),
 ( 0.000000000000000000, 0.5000000000000000000, 1.000000000000000000 ),
 ( 0.000000000000000000, 1.000000000000000000 ),
 .UNSPECIFIED. ) 
 GEOMETRIC_REPRESENTATION_ITEM ( )  RATIONAL_B_SPLINE_SURFACE ( (
 ( 1.000000000000000000, 1.000000000000000000),
 ( 0.3333333333333335369, 0.3333333333333330373),
 ( 0.3333333333333335369, 0.3333333333333330373),
 ( 1.000000000000000000, 1.000000000000000000),
 ( 0.3333333333333333703, 0.3333333333333333703),
 ( 0.3333333333333333703, 0.3333333333333333703),
 ( 1.000000000000000000, 1.000000000000000000) ) ) 
 REPRESENTATION_ITEM ( '' )  SURFACE ( )  );
#3638 = EDGE_CURVE ( 'NONE', #36414, #48232, #2611, .T. ) ;
#3639 = ORIENTED_EDGE ( 'NONE', *, *, #23925, .T. ) ;
#3640 = CARTESIAN_POINT ( 'NONE',  ( -20.38226146016681994, -7.971588334861294811, 70.36604906519886526 ) ) ;
#3641 = DIRECTION ( 'NONE',  ( -0.9687793358424822143, 0.2479245821708672415, 0.000000000000000000 ) ) ;
#3642 = CARTESIAN_POINT ( 'NONE',  ( -13.41327373486474883, -20.54621981236622830, 58.04650078084816300 ) ) ;
#3643 = ORIENTED_EDGE ( 'NONE', *, *, #27487, .F. ) ;
#3644 = LINE ( 'NONE', #26542, #30478 ) ;
#3645 = CARTESIAN_POINT ( 'NONE',  ( -10.03804196927290882, -15.78895246822652076, 64.69426957934942379 ) ) ;
#3646 = PLANE ( 'NONE',  #15794 ) ;
#3647 = VERTEX_POINT ( 'NONE', #44470 ) ;
#3648 = PLANE ( 'NONE',  #35390 ) ;
#3649 = ORIENTED_EDGE ( 'NONE', *, *, #1506, .F. ) ;
#3650 = CARTESIAN_POINT ( 'NONE',  ( -36.42409385541304800, -8.109206544743658540, 50.50000000000030553 ) ) ;
#3651 = CARTESIAN_POINT ( 'NONE',  ( -12.36756753426621813, -9.896138138887707214, 57.37463480816234096 ) ) ;
#3652 = VERTEX_POINT ( 'NONE', #17380 ) ;
#3653 = CARTESIAN_POINT ( 'NONE',  ( -24.77723895724858494, -16.00713575449774595, 66.24820309305337673 ) ) ;
#3654 = DIRECTION ( 'NONE',  ( -0.9990515194385544140, -0.04354378839186318073, 1.103613758316041049E-08 ) ) ;
#3655 = EDGE_CURVE ( 'NONE', #44694, #12297, #28439, .T. ) ;
#3656 = ORIENTED_EDGE ( 'NONE', *, *, #33432, .T. ) ;
#3657 = CARTESIAN_POINT ( 'NONE',  ( -22.06352374043166265, -8.980015506435984562, 63.37649162950052784 ) ) ;
#3658 = CARTESIAN_POINT ( 'NONE',  ( -16.41802950720715160, -7.880257431743621588, 60.38955644688196855 ) ) ;
#3659 = CARTESIAN_POINT ( 'NONE',  ( -24.32752796592761158, -15.96791130369872391, 66.06324927019940674 ) ) ;
#3660 = ORIENTED_EDGE ( 'NONE', *, *, #4163, .T. ) ;
#3661 = CARTESIAN_POINT ( 'NONE',  ( -45.92409385541306222, -14.20920654474410760, 70.50000000000000000 ) ) ;
#3662 = AXIS2_PLACEMENT_3D ( 'NONE', #12276, #35160, #9083 ) ;
#3663 = CIRCLE ( 'NONE', #11509, 1.250000000000001110 ) ;
#3664 = ADVANCED_FACE ( 'NONE', ( #25024 ), #2126, .T. ) ;
#3665 = CARTESIAN_POINT ( 'NONE',  ( -20.95545100651803594, -20.91135505560678354, 65.59926067308570907 ) ) ;
#3666 = PLANE ( 'NONE',  #37356 ) ;
#3667 = ORIENTED_EDGE ( 'NONE', *, *, #34327, .F. ) ;
#3668 = ORIENTED_EDGE ( 'NONE', *, *, #35060, .T. ) ;
#3669 = CARTESIAN_POINT ( 'NONE',  ( -22.30326020397728115, -9.709333660337318150, 73.63728338005337548 ) ) ;
#3670 = FACE_OUTER_BOUND ( 'NONE', #8068, .T. ) ;
#3671 = CARTESIAN_POINT ( 'NONE',  ( -23.32045150837215175, -18.68837265512984303, 62.50973769122266788 ) ) ;
#3672 = PLANE ( 'NONE',  #47239 ) ;
#3673 = EDGE_CURVE ( 'NONE', #10295, #4829, #43506, .T. ) ;
#3674 = AXIS2_PLACEMENT_3D ( 'NONE', #39586, #35875, #24592 ) ;
#3675 = CARTESIAN_POINT ( 'NONE',  ( -16.14284385759799534, -7.587656875400192291, 49.25157356644813689 ) ) ;
#3676 = CARTESIAN_POINT ( 'NONE',  ( -20.13271805750754595, -8.299978134201072777, 70.53628287813307907 ) ) ;
#3677 = CARTESIAN_POINT ( 'NONE',  ( -24.10584550580110985, -12.56049697540380095, 73.54225570139644219 ) ) ;
#3678 = CARTESIAN_POINT ( 'NONE',  ( -24.29205067375949056, -17.69794899492463713, 66.13012485676826202 ) ) ;
#3679 = CARTESIAN_POINT ( 'NONE',  ( -14.69865266434688955, -8.361098232125304008, 63.80595424419050232 ) ) ;
#3680 = EDGE_LOOP ( 'NONE', ( #23347, #40733 ) ) ;
#3681 = B_SPLINE_CURVE_WITH_KNOTS ( 'NONE', 3,
 ( #41374, #34723, #3713, #18716, #4689, #30561, #34222, #7669, #41880, #11346 ),
 .UNSPECIFIED., .F., .F.,
 ( 4, 2, 2, 2, 4 ),
 ( 0.000000000000000000, 0.2500000000000000000, 0.5000000000000000000, 0.7500000000000000000, 1.000000000000000000 ),
 .UNSPECIFIED. ) ;
#3682 = FACE_OUTER_BOUND ( 'NONE', #6869, .T. ) ;
#3683 =( NAMED_UNIT ( * ) SI_UNIT ( $, .STERADIAN. ) SOLID_ANGLE_UNIT ( ) );
#3684 = CYLINDRICAL_SURFACE ( 'NONE', #7549, 0.1500000000000005218 ) ;
#3685 = CARTESIAN_POINT ( 'NONE',  ( -14.66790711817407278, -21.29843871104708342, 58.18089935161520287 ) ) ;
#3686 =( BOUNDED_CURVE ( )  B_SPLINE_CURVE ( 2, ( #44512, #44280, #25540, #25313, #33390, #18623, #33637, #25786, #29242 ),
 .UNSPECIFIED., .F., .F. ) 
 B_SPLINE_CURVE_WITH_KNOTS ( ( 3, 2, 2, 2, 3 ),
 ( 0.8750000000000000000, 0.8854166666666666297, 0.8958333333333333703, 0.9062500000000000000, 0.9166666666666666297 ),
 .UNSPECIFIED. ) 
 CURVE ( )  GEOMETRIC_REPRESENTATION_ITEM ( )  RATIONAL_B_SPLINE_CURVE ( ( 1.000000000000000000, 0.9238795325112867385, 1.000000000000000000, 0.9238795325112867385, 1.000000000000000000, 0.9238795325112867385, 1.000000000000000000, 0.9238795325112867385, 1.000000000000000000 ) ) 
 REPRESENTATION_ITEM ( '' )  );
#3687 = EDGE_CURVE ( 'NONE', #19987, #31666, #40285, .T. ) ;
#3688 = ORIENTED_EDGE ( 'NONE', *, *, #19369, .F. ) ;
#3689 = EDGE_CURVE ( 'NONE', #18786, #26541, #33115, .T. ) ;
#3690 = B_SPLINE_CURVE_WITH_KNOTS ( 'NONE', 3,
 ( #42909, #31822, #35263, #47339, #20980, #35982, #28125, #2510, #28613, #39931 ),
 .UNSPECIFIED., .F., .F.,
 ( 4, 2, 2, 2, 4 ),
 ( 0.000000000000000000, 0.2500000000000000000, 0.5000000000000000000, 0.7500000000000000000, 1.000000000000000000 ),
 .UNSPECIFIED. ) ;
#3691 = ORIENTED_EDGE ( 'NONE', *, *, #20048, .F. ) ;
#3692 = EDGE_CURVE ( 'NONE', #10012, #40467, #3334, .T. ) ;
#3693 = FACE_OUTER_BOUND ( 'NONE', #45163, .T. ) ;
#3694 = CARTESIAN_POINT ( 'NONE',  ( -10.63166622156590790, -13.11537716526513186, 71.22445270976328402 ) ) ;
#3695 = B_SPLINE_CURVE_WITH_KNOTS ( 'NONE', 3,
 ( #2707, #5704, #14007, #16750, #13057, #47052, #28088, #13292, #43373, #24888 ),
 .UNSPECIFIED., .F., .F.,
 ( 4, 2, 2, 2, 4 ),
 ( 0.000000000000000000, 0.2500000000000000000, 0.5000000000000000000, 0.7500000000000000000, 1.000000000000000000 ),
 .UNSPECIFIED. ) ;
#3696 = DIRECTION ( 'NONE',  ( 1.000000000000000000, 2.866981220435666553E-17, 0.000000000000000000 ) ) ;
#3697 = CARTESIAN_POINT ( 'NONE',  ( -10.18562964238619806, -13.04598147208188053, 71.38641367950162930 ) ) ;
#3698 = ORIENTED_EDGE ( 'NONE', *, *, #13348, .F. ) ;
#3699 =( BOUNDED_SURFACE ( )  B_SPLINE_SURFACE ( 3, 1, ( 
 ( #35061, #1324 ),
 ( #45202, #26471 ),
 ( #45442, #41486 ),
 ( #7777, #22795 ),
 ( #37789, #378 ),
 ( #26723, #15361 ),
 ( #30427, #23039 ) ),
 .UNSPECIFIED., .T., .F., .F. ) 
 B_SPLINE_SURFACE_WITH_KNOTS ( ( 4, 3, 4 ),
 ( 2, 2 ),
 ( 0.000000000000000000, 0.5000000000000000000, 1.000000000000000000 ),
 ( 0.000000000000000000, 1.000000000000000000 ),
 .UNSPECIFIED. ) 
 GEOMETRIC_REPRESENTATION_ITEM ( )  RATIONAL_B_SPLINE_SURFACE ( (
 ( 1.000000000000000000, 1.000000000000000000),
 ( 0.3333333333333335369, 0.3333333333333330373),
 ( 0.3333333333333335369, 0.3333333333333330373),
 ( 1.000000000000000000, 1.000000000000000000),
 ( 0.3333333333333333703, 0.3333333333333333703),
 ( 0.3333333333333333703, 0.3333333333333333703),
 ( 1.000000000000000000, 1.000000000000000000) ) ) 
 REPRESENTATION_ITEM ( '' )  SURFACE ( )  );
#3700 = DIRECTION ( 'NONE',  ( 0.3964226963016398431, 0.9180681052388965924, 0.000000000000000000 ) ) ;
#3701 = AXIS2_PLACEMENT_3D ( 'NONE', #45812, #38147, #38389 ) ;
#3702 = CARTESIAN_POINT ( 'NONE',  ( -14.36817892824948650, -8.455618309860652104, 67.54503025475185041 ) ) ;
#3703 = ORIENTED_EDGE ( 'NONE', *, *, #8514, .T. ) ;
#3704 = CARTESIAN_POINT ( 'NONE',  ( -17.42409385541306222, -15.20920654474411116, 75.49999999999998579 ) ) ;
#3705 = AXIS2_PLACEMENT_3D ( 'NONE', #27574, #8870, #46293 ) ;
#3706 = CARTESIAN_POINT ( 'NONE',  ( -10.99582063857411995, -11.91441743271276366, 74.55840195587596497 ) ) ;
#3707 = CARTESIAN_POINT ( 'NONE',  ( -14.05440619237976385, -8.616608212056021898, 74.49954658714564459 ) ) ;
#3708 = ORIENTED_EDGE ( 'NONE', *, *, #26564, .T. ) ;
#3709 = B_SPLINE_CURVE_WITH_KNOTS ( 'NONE', 3,
 ( #35428, #741, #15739, #13015, #44468, #9349, #44716, #18334, #48148, #48381 ),
 .UNSPECIFIED., .F., .F.,
 ( 4, 2, 2, 2, 4 ),
 ( 0.000000000000000000, 0.2500000000000000000, 0.5000000000000000000, 0.7500000000000000000, 1.000000000000000000 ),
 .UNSPECIFIED. ) ;
#3710 = CARTESIAN_POINT ( 'NONE',  ( -12.25319814409069252, -20.17255476956438542, 64.91028984507975963 ) ) ;
#3711 = ORIENTED_EDGE ( 'NONE', *, *, #28339, .F. ) ;
#3712 = CARTESIAN_POINT ( 'NONE',  ( -17.42409385541299471, -14.80920654474435771, 49.52966884056655772 ) ) ;
#3713 = CARTESIAN_POINT ( 'NONE',  ( -20.45830450918359489, -8.500926063925801301, 63.32623952627614017 ) ) ;
#3714 = EDGE_LOOP ( 'NONE', ( #37591, #22018, #30444, #11654, #6115 ) ) ;
#3715 = CARTESIAN_POINT ( 'NONE',  ( -17.42409385541299471, -14.80920654474435594, 52.02966884056656482 ) ) ;
#3716 = PLANE ( 'NONE',  #43067 ) ;
#3717 = CARTESIAN_POINT ( 'NONE',  ( -21.93659385650551741, -6.915538690918074494, 49.31353937987644542 ) ) ;
#3718 = CYLINDRICAL_SURFACE ( 'NONE', #39370, 0.4000000000000011879 ) ;
#3719 = CARTESIAN_POINT ( 'NONE',  ( -24.29299122354570883, -17.69571185755203757, 62.58705726155704951 ) ) ;
#3720 = DIRECTION ( 'NONE',  ( -1.000000000000000000, -1.669677910507523057E-21, -6.493791346278465266E-22 ) ) ;
#3721 = CARTESIAN_POINT ( 'NONE',  ( -46.92409385541305511, -15.80920654474410725, 62.75000000000000000 ) ) ;
#3722 = ORIENTED_EDGE ( 'NONE', *, *, #11329, .F. ) ;
#3723 = CARTESIAN_POINT ( 'NONE',  ( -10.43906310151734651, -14.34979072177226911, 64.68803843020796762 ) ) ;
#3724 = CARTESIAN_POINT ( 'NONE',  ( -15.68503317936312236, -7.977064329016500643, 70.60989839961001735 ) ) ;
#3725 = CARTESIAN_POINT ( 'NONE',  ( -18.11396590982544197, -21.77512906430638040, 65.64532159443497505 ) ) ;
#3726 = CARTESIAN_POINT ( 'NONE',  ( -10.70566809389435647, -16.94585225683366048, 57.68760548748759476 ) ) ;
#3727 = EDGE_CURVE ( 'NONE', #24420, #15891, #29934, .T. ) ;
#3728 = DIRECTION ( 'NONE',  ( -3.071710424422018668E-17, 6.404604876783312462E-16, 1.000000000000000000 ) ) ;
#3729 = CARTESIAN_POINT ( 'NONE',  ( -13.12613380977788147, -20.89454282643029259, 58.16154686733092660 ) ) ;
#3730 = ORIENTED_EDGE ( 'NONE', *, *, #43738, .T. ) ;
#3731 = ORIENTED_EDGE ( 'NONE', *, *, #8386, .F. ) ;
#3732 = CARTESIAN_POINT ( 'NONE',  ( -21.68499379980493558, -9.192514338196573931, 66.96149992326067490 ) ) ;
#3733 = ORIENTED_EDGE ( 'NONE', *, *, #25222, .T. ) ;
#3735 = CARTESIAN_POINT ( 'NONE',  ( -21.02603828283602283, -21.33060232236718434, 62.31482603073411042 ) ) ;
#3734 = CARTESIAN_POINT ( 'NONE',  ( -15.37275756075460365, -7.647176670682967803, 74.17962025520618852 ) ) ;
#3736 = CARTESIAN_POINT ( 'NONE',  ( -15.30563816890515660, -21.53343246974097625, 68.87592909656478923 ) ) ;
#3737 = CARTESIAN_POINT ( 'NONE',  ( -11.59700437785899574, -18.68821983113924645, 64.74707024157237356 ) ) ;
#3738 = FACE_OUTER_BOUND ( 'NONE', #37025, .T. ) ;
#3739 = FACE_BOUND ( 'NONE', #25058, .T. ) ;
#3740 = CARTESIAN_POINT ( 'NONE',  ( -11.42008220035761923, -19.21999808210960836, 71.88024208098950396 ) ) ;
#3741 = DIRECTION ( 'NONE',  ( 0.7029450532227031756, 0.7112441579020041260, -7.405715380709556396E-09 ) ) ;
#3742 = DIRECTION ( 'NONE',  ( 1.000000000000000000, 0.000000000000000000, 0.000000000000000000 ) ) ;
#3743 = EDGE_LOOP ( 'NONE', ( #21317, #36870, #18935, #3927, #36844 ) ) ;
#3744 = CARTESIAN_POINT ( 'NONE',  ( -17.52853272358826686, -7.759682304905023642, 63.83584969886392457 ) ) ;
#3745 = FACE_OUTER_BOUND ( 'NONE', #38121, .T. ) ;
#3746 = CARTESIAN_POINT ( 'NONE',  ( -12.82148049030644366, -13.86501071932494789, 52.02966884056656482 ) ) ;
#3747 = AXIS2_PLACEMENT_3D ( 'NONE', #36224, #47336, #10618 ) ;
#3748 = DIRECTION ( 'NONE',  ( 0.000000000000000000, 0.000000000000000000, 1.000000000000000000 ) ) ;
#3749 = CARTESIAN_POINT ( 'NONE',  ( -24.20371252810814866, -12.87440185077122834, 66.58774614429587757 ) ) ;
#3750 = CARTESIAN_POINT ( 'NONE',  ( -14.78766009005058812, -21.34800739930362568, 58.45145834864037937 ) ) ;
#3751 = CARTESIAN_POINT ( 'NONE',  ( -18.18338144371267617, -21.81849904615365432, 65.63060065626805795 ) ) ;
#3752 = VECTOR ( 'NONE', #25357, 1000.000000000000114 ) ;
#3754 = ORIENTED_EDGE ( 'NONE', *, *, #47592, .T. ) ;
#3753 = EDGE_CURVE ( 'NONE', #19773, #8811, #47716, .T. ) ;
#3755 = ORIENTED_EDGE ( 'NONE', *, *, #3524, .F. ) ;
#3756 = CARTESIAN_POINT ( 'NONE',  ( -16.11159385541304445, -8.990409506049202193, 49.61344411288074951 ) ) ;
#3757 = EDGE_LOOP ( 'NONE', ( #22338, #9402, #2962, #36549 ) ) ;
#3758 = ADVANCED_FACE ( 'NONE', ( #14620 ), #8260, .T. ) ;
#3759 = EDGE_CURVE ( 'NONE', #32800, #37610, #44835, .T. ) ;
#3760 = CARTESIAN_POINT ( 'NONE',  ( -17.36874312174564139, -7.359362613910461093, 67.12701303326514335 ) ) ;
#3761 = B_SPLINE_CURVE_WITH_KNOTS ( 'NONE', 1,
 ( #15404, #45249 ),
 .UNSPECIFIED., .F., .F.,
 ( 2, 2 ),
 ( 0.000000000000000000, 1.000000000000000000 ),
 .UNSPECIFIED. ) ;
#3762 = CARTESIAN_POINT ( 'NONE',  ( -14.23827708255551627, -10.77544123782542407, 49.52966884056655772 ) ) ;
#3763 = B_SPLINE_CURVE_WITH_KNOTS ( 'NONE', 3,
 ( #3981, #45835, #12090, #18993, #33996, #27103, #8397, #38417, #4703, #35933 ),
 .UNSPECIFIED., .F., .F.,
 ( 4, 2, 2, 2, 4 ),
 ( 0.000000000000000000, 0.2500000000000000000, 0.5000000000000000000, 0.7500000000000000000, 1.000000000000000000 ),
 .UNSPECIFIED. ) ;
#3764 = CARTESIAN_POINT ( 'NONE',  ( -13.33034385759799001, -6.857644439848016304, 49.98602051094140819 ) ) ;
#3765 = CARTESIAN_POINT ( 'NONE',  ( -18.12574864353739201, -7.786197982121914052, 60.22493603095571046 ) ) ;
#3766 = EDGE_LOOP ( 'NONE', ( #33173, #19959, #8479, #30937 ) ) ;
#3767 = CARTESIAN_POINT ( 'NONE',  ( -20.49170831689750472, -8.461258797198503601, 63.59649424907593129 ) ) ;
#3768 = VECTOR ( 'NONE', #41992, 1000.000000000000114 ) ;
#3769 = DIRECTION ( 'NONE',  ( 1.000000000000000000, -0.000000000000000000, -2.406186529621654511E-16 ) ) ;
#3770 = ORIENTED_EDGE ( 'NONE', *, *, #33455, .T. ) ;
#3771 = CARTESIAN_POINT ( 'NONE',  ( -14.90981300391231024, -21.39562377109201208, 61.63600440604547970 ) ) ;
#3772 = CARTESIAN_POINT ( 'NONE',  ( -10.37141135217074961, -14.92372438906622811, 71.53602713937311819 ) ) ;
#3773 = CIRCLE ( 'NONE', #47805, 2.000000000000001776 ) ;
#3774 = AXIS2_PLACEMENT_3D ( 'NONE', #35735, #38041, #8940 ) ;
#3775 = ORIENTED_EDGE ( 'NONE', *, *, #30141, .T. ) ;
#3776 = CARTESIAN_POINT ( 'NONE',  ( -19.50844099596679371, -21.96177777289817357, 62.11008350414853396 ) ) ;
#3777 = CARTESIAN_POINT ( 'NONE',  ( -15.48424059001683339, -21.53504990492328375, 72.04575460974366763 ) ) ;
#3778 = CARTESIAN_POINT ( 'NONE',  ( -9.979977042000861331, -14.51194761097949382, 67.96461827199280492 ) ) ;
#3779 = ORIENTED_EDGE ( 'NONE', *, *, #21152, .T. ) ;
#3780 = CARTESIAN_POINT ( 'NONE',  ( -10.68551981713787136, -12.73596763222149164, 64.28308208171728211 ) ) ;
#3781 = ADVANCED_FACE ( 'NONE', ( #33345, #38029 ), #44972, .F. ) ;
#3782 = CARTESIAN_POINT ( 'NONE',  ( -24.34138212120913991, -16.17068457824029792, 62.74328676669021831 ) ) ;
#3783 = AXIS2_PLACEMENT_3D ( 'NONE', #10743, #30211, #48410 ) ;
#3784 = CARTESIAN_POINT ( 'NONE',  ( -24.68345461824787890, -13.13130818398968103, 59.47612521039077649 ) ) ;
#3785 = CARTESIAN_POINT ( 'NONE',  ( -10.93232766038821424, -17.55941949638709687, 68.38249893951126523 ) ) ;
#3786 = ORIENTED_EDGE ( 'NONE', *, *, #13151, .T. ) ;
#3787 = CARTESIAN_POINT ( 'NONE',  ( -24.34586551078590233, -16.16342498662110572, 59.00843562520186936 ) ) ;
#3788 = DIRECTION ( 'NONE',  ( 0.9997277805376392212, -0.02333162706040292633, -9.101776391673708383E-09 ) ) ;
#3789 = VECTOR ( 'NONE', #2751, 999.9999999999998863 ) ;
#3790 = DIRECTION ( 'NONE',  ( -3.413470714839332458E-33, 1.190614954331866791E-16, -1.000000000000000000 ) ) ;
#3791 = CARTESIAN_POINT ( 'NONE',  ( -19.45281838860202228, -9.697037067072807659, 53.49999999999995026 ) ) ;
#3792 = CARTESIAN_POINT ( 'NONE',  ( -23.51785832295892931, -11.36449550514380036, 69.89210750611785272 ) ) ;
#3793 = CARTESIAN_POINT ( 'NONE',  ( -10.49291259435924673, -15.78913940232298785, 64.50771630042218874 ) ) ;
#3794 = CARTESIAN_POINT ( 'NONE',  ( -19.59909385650551883, -8.114302828567740988, 52.18300498402516041 ) ) ;
#3795 = EDGE_LOOP ( 'NONE', ( #28513, #48162, #21774, #2345, #32422 ) ) ;
#3796 = EDGE_CURVE ( 'NONE', #18177, #21199, #14871, .T. ) ;
#3797 = DIRECTION ( 'NONE',  ( -0.3688590060343601151, 0.9294853595766551235, -9.484706316669577488E-17 ) ) ;
#3798 = CARTESIAN_POINT ( 'NONE',  ( -24.69856829750257177, -13.20119948815759159, 59.40621968628075678 ) ) ;
#3799 = ORIENTED_EDGE ( 'NONE', *, *, #1828, .F. ) ;
#3800 = CARTESIAN_POINT ( 'NONE',  ( 18.07590614458695200, 2.137415583567194854, 51.63103269608403423 ) ) ;
#3801 = CARTESIAN_POINT ( 'NONE',  ( -21.65534385759799818, -8.623186033802570094, 49.24843789510466507 ) ) ;
#3802 = DIRECTION ( 'NONE',  ( 3.549360974554993999E-17, -6.371834667797928663E-18, -1.000000000000000000 ) ) ;
#3803 = ORIENTED_EDGE ( 'NONE', *, *, #21440, .F. ) ;
#3804 = CARTESIAN_POINT ( 'NONE',  ( -18.10946867608448940, -21.82882885753907942, 69.23003497527133732 ) ) ;
#3805 = CARTESIAN_POINT ( 'NONE',  ( -18.41353416428395917, -22.19337852133874023, 68.95368170273926012 ) ) ;
#3806 = ORIENTED_EDGE ( 'NONE', *, *, #9765, .T. ) ;
#3807 = CARTESIAN_POINT ( 'NONE',  ( -15.94284385650552238, -8.811426318492348031, 52.18089403414752070 ) ) ;
#3808 = AXIS2_PLACEMENT_3D ( 'NONE', #10988, #18354, #10507 ) ;
#3809 = CARTESIAN_POINT ( 'NONE',  ( -12.83571665415373708, -8.939642480694315552, 67.51796240912459268 ) ) ;
#3810 = VECTOR ( 'NONE', #13222, 1000.000000000000000 ) ;
#3811 = CARTESIAN_POINT ( 'NONE',  ( -24.79781836340079337, -15.87314503134675014, 69.64812095075065201 ) ) ;
#3812 = CARTESIAN_POINT ( 'NONE',  ( -18.92057448382017881, -7.919863665830077615, 67.20071783788056052 ) ) ;
#3813 = FACE_OUTER_BOUND ( 'NONE', #10196, .T. ) ;
#3814 = VECTOR ( 'NONE', #9796, 1000.000000000000000 ) ;
#3815 = CIRCLE ( 'NONE', #26626, 1.700000000000001954 ) ;
#3816 = ORIENTED_EDGE ( 'NONE', *, *, #47032, .T. ) ;
#3817 = ORIENTED_EDGE ( 'NONE', *, *, #35766, .T. ) ;
#3818 = CARTESIAN_POINT ( 'NONE',  ( -15.41159385650551705, -6.922745924619793101, 51.69366785382590024 ) ) ;
#3819 = EDGE_CURVE ( 'NONE', #18099, #25345, #36597, .T. ) ;
#3820 = ADVANCED_FACE ( 'NONE', ( #30674 ), #45697, .T. ) ;
#3821 = CARTESIAN_POINT ( 'NONE',  ( -23.41977899678227004, -11.19648470850049904, 73.36193302072521760 ) ) ;
#3822 = CIRCLE ( 'NONE', #46286, 1.500000000000001332 ) ;
#3823 = DIRECTION ( 'NONE',  ( 0.000000000000000000, 0.000000000000000000, -1.000000000000000000 ) ) ;
#3824 = CARTESIAN_POINT ( 'NONE',  ( -14.68034385650551599, -6.424090610841176385, 49.80797279389977916 ) ) ;
#3825 = EDGE_CURVE ( 'NONE', #41834, #27306, #21987, .T. ) ;
#3827 = ORIENTED_EDGE ( 'NONE', *, *, #29669, .T. ) ;
#3826 = EDGE_CURVE ( 'NONE', #34652, #19690, #19421, .T. ) ;
#3828 = DIRECTION ( 'NONE',  ( 3.071710424422018668E-17, -6.404604876783312462E-16, -1.000000000000000000 ) ) ;
#3829 = EDGE_CURVE ( 'NONE', #8929, #31196, #38989, .T. ) ;
#3830 = CARTESIAN_POINT ( 'NONE',  ( -12.44869033171645611, -9.885248809711741913, 57.38935532200543577 ) ) ;
#3831 = EDGE_CURVE ( 'NONE', #12002, #2683, #8426, .T. ) ;
#3832 = CARTESIAN_POINT ( 'NONE',  ( -24.43235039625237803, -15.64544980915412431, 66.21891754810816622 ) ) ;
#3833 =( BOUNDED_SURFACE ( )  B_SPLINE_SURFACE ( 3, 1, ( 
 ( #30779, #19429 ),
 ( #38369, #34435 ),
 ( #729, #15722 ),
 ( #45800, #34692 ),
 ( #26099, #16693 ),
 ( #42593, #31008 ),
 ( #46028, #24350 ) ),
 .UNSPECIFIED., .T., .F., .F. ) 
 B_SPLINE_SURFACE_WITH_KNOTS ( ( 4, 3, 4 ),
 ( 2, 2 ),
 ( 0.000000000000000000, 0.5000000000000000000, 1.000000000000000000 ),
 ( 0.000000000000000000, 1.000000000000000000 ),
 .UNSPECIFIED. ) 
 GEOMETRIC_REPRESENTATION_ITEM ( )  RATIONAL_B_SPLINE_SURFACE ( (
 ( 1.000000000000000000, 1.000000000000000000),
 ( 0.3333333333333335369, 0.3333333333333330373),
 ( 0.3333333333333335369, 0.3333333333333330373),
 ( 1.000000000000000000, 1.000000000000000000),
 ( 0.3333333333333333703, 0.3333333333333333703),
 ( 0.3333333333333333703, 0.3333333333333333703),
 ( 1.000000000000000000, 1.000000000000000000) ) ) 
 REPRESENTATION_ITEM ( '' )  SURFACE ( )  );
#3834 = ORIENTED_EDGE ( 'NONE', *, *, #35709, .T. ) ;
#3835 = B_SPLINE_CURVE_WITH_KNOTS ( 'NONE', 3,
 ( #45782, #19408, #7865, #30271, #18665, #29768, #15211, #22886, #7373, #4392 ),
 .UNSPECIFIED., .F., .F.,
 ( 4, 2, 2, 2, 4 ),
 ( 0.000000000000000000, 0.2500000000000000000, 0.5000000000000000000, 0.7500000000000000000, 1.000000000000000000 ),
 .UNSPECIFIED. ) ;
#3836 = ORIENTED_EDGE ( 'NONE', *, *, #34330, .F. ) ;
#3837 = DIRECTION ( 'NONE',  ( -8.719004481856245202E-07, 8.513143972389065227E-07, -0.9999999999992574828 ) ) ;
#3838 = CARTESIAN_POINT ( 'NONE',  ( -18.30727046116018286, -21.75326869042403288, 69.11514702556002021 ) ) ;
#3839 = CARTESIAN_POINT ( 'NONE',  ( -24.42163167104895294, -17.36632341347029751, 69.59056710591525530 ) ) ;
#3840 = CARTESIAN_POINT ( 'NONE',  ( -16.92014803599858652, -22.24222107688192196, 72.42189142509964483 ) ) ;
#3841 = ADVANCED_FACE ( 'NONE', ( #37532 ), #45208, .T. ) ;
#3842 = VERTEX_POINT ( 'NONE', #46659 ) ;
#3843 = LINE ( 'NONE', #18588, #13906 ) ;
#3844 = AXIS2_PLACEMENT_3D ( 'NONE', #25632, #2978, #17989 ) ;
#3845 = CARTESIAN_POINT ( 'NONE',  ( -15.38656303155622673, -21.97522069389735222, 72.23849606682514946 ) ) ;
#3846 = AXIS2_PLACEMENT_3D ( 'NONE', #37091, #10528, #33148 ) ;
#3847 = CARTESIAN_POINT ( 'NONE',  ( -12.84690951644825851, -8.931012861620404308, 67.56438176077992352 ) ) ;
#3848 = CARTESIAN_POINT ( 'NONE',  ( -19.80301260837064703, -21.44571507605098404, 69.23482476707422961 ) ) ;
#3849 = ORIENTED_EDGE ( 'NONE', *, *, #40961, .F. ) ;
#3850 = CARTESIAN_POINT ( 'NONE',  ( -19.50112608350124788, -21.96394757316516433, 62.11786765711682534 ) ) ;
#3851 = DIRECTION ( 'NONE',  ( -3.071710424422018668E-17, 6.404604876783312462E-16, 1.000000000000000000 ) ) ;
#3852 =( BOUNDED_CURVE ( )  B_SPLINE_CURVE ( 3, ( #17480, #17710, #10585, #32279 ),
 .UNSPECIFIED., .F., .F. ) 
 B_SPLINE_CURVE_WITH_KNOTS ( ( 4, 4 ),
 ( 0.5000000000000000000, 0.9074455897393656212 ),
 .UNSPECIFIED. ) 
 CURVE ( )  GEOMETRIC_REPRESENTATION_ITEM ( )  RATIONAL_B_SPLINE_CURVE ( ( 0.9999999999999958922, 0.4567392136813264170, 0.3561768502900310995, 0.6983129098261053880 ) ) 
 REPRESENTATION_ITEM ( '' )  );
#3853 = CIRCLE ( 'NONE', #36815, 0.5000000000000004441 ) ;
#3855 = LINE ( 'NONE', #3350, #37224 ) ;
#3854 = AXIS2_PLACEMENT_3D ( 'NONE', #42661, #9160, #4740 ) ;
#3856 = FACE_BOUND ( 'NONE', #24866, .T. ) ;
#3857 = ORIENTED_EDGE ( 'NONE', *, *, #33166, .T. ) ;
#3858 = CARTESIAN_POINT ( 'NONE',  ( -13.13317054870913125, -20.89946229583447135, 58.23988401356517386 ) ) ;
#3859 = DIRECTION ( 'NONE',  ( -3.071710424422018668E-17, 6.404604876783312462E-16, 1.000000000000000000 ) ) ;
#3860 = DIRECTION ( 'NONE',  ( -3.071710424422018668E-17, 6.404604876783312462E-16, 1.000000000000000000 ) ) ;
#3861 = CARTESIAN_POINT ( 'NONE',  ( -14.87409385541153917, -6.859212275519794844, 50.50378509015643402 ) ) ;
#3862 = ORIENTED_EDGE ( 'NONE', *, *, #39003, .T. ) ;
#3863 = CARTESIAN_POINT ( 'NONE',  ( -10.13258914451759019, -16.33817228489381179, 71.63245656337019796 ) ) ;
#3864 = CIRCLE ( 'NONE', #37648, 1.999999999999999778 ) ;
#3865 = VERTEX_POINT ( 'NONE', #34826 ) ;
#3866 = DIRECTION ( 'NONE',  ( 0.7150252244155669290, -0.6990986543038600898, 2.983336731533460772E-17 ) ) ;
#3867 = CARTESIAN_POINT ( 'NONE',  ( -10.99273270719357498, -18.56964325624270273, 57.99988733456820000 ) ) ;
#3868 = VERTEX_POINT ( 'NONE', #45925 ) ;
#3869 = CARTESIAN_POINT ( 'NONE',  ( -21.62450594022013206, -20.48119921038467695, 72.68013252948732372 ) ) ;
#3870 =( BOUNDED_CURVE ( )  B_SPLINE_CURVE ( 3, ( #33231, #14275, #41138, #21465 ),
 .UNSPECIFIED., .F., .F. ) 
 B_SPLINE_CURVE_WITH_KNOTS ( ( 4, 4 ),
 ( 0.9074455897393656212, 1.000000000000000000 ),
 .UNSPECIFIED. ) 
 CURVE ( )  GEOMETRIC_REPRESENTATION_ITEM ( )  RATIONAL_B_SPLINE_CURVE ( ( 0.6983129098261039447, 0.7760317562607076392, 0.8765941196520062872, 1.000000000000000000 ) ) 
 REPRESENTATION_ITEM ( '' )  );
#3871 = CARTESIAN_POINT ( 'NONE',  ( -17.42409385541299471, -14.80920654474435594, 52.02966884056656482 ) ) ;
#3872 = ORIENTED_EDGE ( 'NONE', *, *, #23253, .F. ) ;
#3873 = VERTEX_POINT ( 'NONE', #23523 ) ;
#3874 = ORIENTED_EDGE ( 'NONE', *, *, #39353, .T. ) ;
#3875 = CARTESIAN_POINT ( 'NONE',  ( -15.32518410995109193, -21.95751795911967008, 72.16080160551160816 ) ) ;
#3876 = CARTESIAN_POINT ( 'NONE',  ( -20.43185948505062299, -8.432683554863363184, 66.79576150497511833 ) ) ;
#3877 = CARTESIAN_POINT ( 'NONE',  ( -21.15336504700141163, -20.73310185707507713, 69.05450185101547333 ) ) ;
#3878 = CARTESIAN_POINT ( 'NONE',  ( -10.03993391926675116, -13.82001047774868496, 57.62637814497484356 ) ) ;
#3879 = ADVANCED_FACE ( 'NONE', ( #1100 ), #13301, .T. ) ;
#3880 = CARTESIAN_POINT ( 'NONE',  ( -19.37409385541300111, -6.859212275519753099, 50.50378509014300477 ) ) ;
#3881 = CARTESIAN_POINT ( 'NONE',  ( -14.16804786125913118, -8.612086647834459541, 74.48338047236791226 ) ) ;
#3882 = CARTESIAN_POINT ( 'NONE',  ( -13.47466815348274594, -9.357823189459171687, 50.04126597187295289 ) ) ;
#3883 = ORIENTED_EDGE ( 'NONE', *, *, #22351, .T. ) ;
#3884 = EDGE_LOOP ( 'NONE', ( #33436, #19522, #7565, #28926, #14538 ) ) ;
#3885 = CARTESIAN_POINT ( 'NONE',  ( -16.16063142123006813, -7.467037929575190525, 60.38523757159160965 ) ) ;
#3886 = EDGE_CURVE ( 'NONE', #42514, #2110, #20305, .T. ) ;
#3887 = CARTESIAN_POINT ( 'NONE',  ( -13.62460154206902807, -8.321601493802987193, 53.76227901944321985 ) ) ;
#3888 = CARTESIAN_POINT ( 'NONE',  ( -10.90759844528708911, -17.49952021360972765, 68.24721944423116327 ) ) ;
#3889 = CARTESIAN_POINT ( 'NONE',  ( -21.56413130975026959, -4.978830828776663608, 54.49999999999995026 ) ) ;
#3890 = AXIS2_PLACEMENT_3D ( 'NONE', #16696, #43312, #39599 ) ;
#3891 = ORIENTED_EDGE ( 'NONE', *, *, #10977, .T. ) ;
#3892 = CARTESIAN_POINT ( 'NONE',  ( -16.44909385650551670, -8.104110260919579645, 48.81699501597546487 ) ) ;
#3893 = AXIS2_PLACEMENT_3D ( 'NONE', #2047, #25194, #32093 ) ;
#3894 = AXIS2_PLACEMENT_3D ( 'NONE', #39149, #4954, #16728 ) ;
#3895 = VERTEX_POINT ( 'NONE', #16097 ) ;
#3896 = CARTESIAN_POINT ( 'NONE',  ( -10.63004074901718532, -12.92571453866564823, 67.75304464120749515 ) ) ;
#3897 = CARTESIAN_POINT ( 'NONE',  ( -12.45907596150898300, -19.82553632194446180, 58.08249573729000304 ) ) ;
#3898 = EDGE_CURVE ( 'NONE', #2764, #21586, #14880, .T. ) ;
#3899 = CARTESIAN_POINT ( 'NONE',  ( -10.42302287260171312, -13.97751933429587012, 57.73352905910142852 ) ) ;
#3900 = AXIS2_PLACEMENT_3D ( 'NONE', #3241, #36697, #6699 ) ;
#3901 = EDGE_CURVE ( 'NONE', #16737, #11137, #43713, .T. ) ;
#3902 = ORIENTED_EDGE ( 'NONE', *, *, #13741, .F. ) ;
#3903 = CARTESIAN_POINT ( 'NONE',  ( -20.38927765283500904, -7.974583868351674099, 70.37383423426267370 ) ) ;
#3904 = B_SPLINE_CURVE_WITH_KNOTS ( 'NONE', 3,
 ( #17533, #43907, #10160, #33257, #29590, #25181, #40428, #29351, #44621, #6471 ),
 .UNSPECIFIED., .F., .F.,
 ( 4, 2, 2, 2, 4 ),
 ( 0.000000000000000000, 0.2500000000000000000, 0.5000000000000000000, 0.7500000000000000000, 1.000000000000000000 ),
 .UNSPECIFIED. ) ;
#3905 = CARTESIAN_POINT ( 'NONE',  ( -14.56495137627929637, -8.364837042462607286, 64.08419083274510797 ) ) ;
#3906 = ORIENTED_EDGE ( 'NONE', *, *, #21440, .T. ) ;
#3907 = ADVANCED_FACE ( 'NONE', ( #39258 ), #38492, .T. ) ;
#3908 = CARTESIAN_POINT ( 'NONE',  ( -19.30128557755455532, -21.60500301973953086, 58.81035253397666196 ) ) ;
#3909 = DIRECTION ( 'NONE',  ( -6.493791346278467147E-22, 1.224646799147353207E-16, 1.000000000000000000 ) ) ;
#3910 = ORIENTED_EDGE ( 'NONE', *, *, #44313, .T. ) ;
#3911 = CARTESIAN_POINT ( 'NONE',  ( -24.43362360091611052, -14.05489060867666495, 73.42271507725004653 ) ) ;
#3912 = VERTEX_POINT ( 'NONE', #31872 ) ;
#3913 = CYLINDRICAL_SURFACE ( 'NONE', #46235, 1.249999999999998668 ) ;
#3914 = CARTESIAN_POINT ( 'NONE',  ( -24.87140955007623333, -14.60726545267721121, 62.90570658404245563 ) ) ;
#3915 = EDGE_LOOP ( 'NONE', ( #39075, #32708, #30699, #40497, #32037 ) ) ;
#3916 = CARTESIAN_POINT ( 'NONE',  ( -13.28240554951661245, -9.100331501070346718, 67.79431631125400770 ) ) ;
#3917 = CARTESIAN_POINT ( 'NONE',  ( -24.18470913683765389, -12.80901137141652768, 69.78715111652664405 ) ) ;
#3918 = PLANE ( 'NONE',  #11620 ) ;
#3919 = VECTOR ( 'NONE', #19701, 1000.000000000000000 ) ;
#3920 = VERTEX_POINT ( 'NONE', #23279 ) ;
#3921 = DIRECTION ( 'NONE',  ( -1.000000000000000000, 0.000000000000000000, -2.181982678098338148E-16 ) ) ;
#3922 = DIRECTION ( 'NONE',  ( 3.549360974554993999E-17, -6.371834667797928663E-18, -1.000000000000000000 ) ) ;
#3923 = CARTESIAN_POINT ( 'NONE',  ( -19.80301260837064703, -21.44571507605098404, 69.23482476707422961 ) ) ;
#3924 = ORIENTED_EDGE ( 'NONE', *, *, #12671, .F. ) ;
#3925 = CARTESIAN_POINT ( 'NONE',  ( -12.50776634899986384, -20.40684016789016297, 71.92158251742569064 ) ) ;
#3926 = CARTESIAN_POINT ( 'NONE',  ( -23.56138519289638822, -11.33989039198723248, 69.89210750373884196 ) ) ;
#3927 = ORIENTED_EDGE ( 'NONE', *, *, #6598, .T. ) ;
#3928 = EDGE_LOOP ( 'NONE', ( #9167, #36625, #48192, #24682, #2797, #15200, #46207, #43881, #1183, #45781, #28563, #23263 ) ) ;
#3929 = FACE_OUTER_BOUND ( 'NONE', #11304, .T. ) ;
#3930 = CARTESIAN_POINT ( 'NONE',  ( -19.24190894175819366, -7.584296403803404196, 63.54593838833191910 ) ) ;
#3931 = DIRECTION ( 'NONE',  ( 0.8788484374452892878, -0.3260506722428099247, -0.3483050145059431446 ) ) ;
#3932 = AXIS2_PLACEMENT_3D ( 'NONE', #22458, #10886, #25908 ) ;
#3933 = CARTESIAN_POINT ( 'NONE',  ( -13.49909385759798930, -8.105421454601382081, 49.25000573077640098 ) ) ;
#3934 = CARTESIAN_POINT ( 'NONE',  ( -24.39774143530919304, -13.72145442755526545, 73.27838554735291154 ) ) ;
#3935 = EDGE_CURVE ( 'NONE', #42856, #25718, #36605, .T. ) ;
#3936 = CARTESIAN_POINT ( 'NONE',  ( -15.92409385541305333, -14.80920654474410547, 47.99999999999998579 ) ) ;
#3937 = CARTESIAN_POINT ( 'NONE',  ( -16.93047781583662470, -7.375409967019452395, 74.09871763077661910 ) ) ;
#3938 = CARTESIAN_POINT ( 'NONE',  ( -17.13503149044196761, -7.764836982087094164, 70.77563787455143540 ) ) ;
#3939 = ORIENTED_EDGE ( 'NONE', *, *, #14171, .F. ) ;
#3940 = CARTESIAN_POINT ( 'NONE',  ( -20.52762743779272014, -8.534807845156915818, 63.31121513079826713 ) ) ;
#3941 = DIRECTION ( 'NONE',  ( 0.9687793358424819923, -0.2479245821708678243, 0.000000000000000000 ) ) ;
#3942 = CARTESIAN_POINT ( 'NONE',  ( -17.42409385541299471, -14.80920654474435771, 49.52966884056655772 ) ) ;
#3943 = VERTEX_POINT ( 'NONE', #10200 ) ;
#3944 = ORIENTED_EDGE ( 'NONE', *, *, #12913, .T. ) ;
#3945 = CARTESIAN_POINT ( 'NONE',  ( -41.92997620835424044, -14.80920654474420139, 66.95294117647057419 ) ) ;
#3946 = CARTESIAN_POINT ( 'NONE',  ( -10.62264639038924408, -13.15335193860895302, 71.50828630683409415 ) ) ;
#3947 = EDGE_CURVE ( 'NONE', #37009, #3647, #28896, .T. ) ;
#3948 = CARTESIAN_POINT ( 'NONE',  ( -16.75933984047804515, -20.01695097968237036, 49.52966884056656482 ) ) ;
#3949 = CARTESIAN_POINT ( 'NONE',  ( -13.85341075922988985, -21.34777127333467561, 72.12618907608873542 ) ) ;
#3950 = AXIS2_PLACEMENT_3D ( 'NONE', #4500, #568, #19520 ) ;
#3951 = EDGE_CURVE ( 'NONE', #12784, #31348, #23131, .T. ) ;
#3952 = ORIENTED_EDGE ( 'NONE', *, *, #45569, .T. ) ;
#3953 = CIRCLE ( 'NONE', #25952, 4.686499999999999666 ) ;
#3954 = DIRECTION ( 'NONE',  ( -0.3303050442826436783, 0.9438742382973703826, 3.829623549872328964E-09 ) ) ;
#3955 = EDGE_CURVE ( 'NONE', #39108, #36314, #2563, .T. ) ;
#3956 = CARTESIAN_POINT ( 'NONE',  ( -22.23733827145997566, -19.96043728507621395, 65.70421731380814379 ) ) ;
#3957 = VERTEX_POINT ( 'NONE', #14093 ) ;
#3958 = CARTESIAN_POINT ( 'NONE',  ( -24.65023647254185590, -12.99629722456026393, 63.01759562046499497 ) ) ;
#3959 = CIRCLE ( 'NONE', #7127, 0.5000000000000004441 ) ;
#3960 = DIRECTION ( 'NONE',  ( -5.551115123125782702E-17, -1.232595164407830946E-32, -1.000000000000000000 ) ) ;
#3961 = EDGE_CURVE ( 'NONE', #3303, #19706, #44194, .T. ) ;
#3962 = CARTESIAN_POINT ( 'NONE',  ( -22.90552330334707420, -10.36975038659888249, 59.60203168817258046 ) ) ;
#3963 = ORIENTED_EDGE ( 'NONE', *, *, #11242, .F. ) ;
#3964 = CARTESIAN_POINT ( 'NONE',  ( -17.43688419659117983, -7.809108078509128248, 67.32039585984551877 ) ) ;
#3965 = ORIENTED_EDGE ( 'NONE', *, *, #41951, .T. ) ;
#3966 = FACE_OUTER_BOUND ( 'NONE', #11525, .T. ) ;
#3967 = CARTESIAN_POINT ( 'NONE',  ( -17.77658133828675702, -19.49442885748621990, 49.52966884056656482 ) ) ;
#3968 = B_SPLINE_CURVE_WITH_KNOTS ( 'NONE', 3,
 ( #7784, #7534, #45211, #22541, #18583, #37796, #26968, #4092, #33855, #15620 ),
 .UNSPECIFIED., .F., .F.,
 ( 4, 2, 2, 2, 4 ),
 ( 0.1272669073658358463, 0.2522669073463222333, 0.3772669073268086759, 0.5022669073072950630, 0.6272669072877814500 ),
 .UNSPECIFIED. ) ;
#3969 = ORIENTED_EDGE ( 'NONE', *, *, #32677, .F. ) ;
#3970 = CARTESIAN_POINT ( 'NONE',  ( -13.42948644998191732, -8.996466925491649391, 56.85478874482843992 ) ) ;
#3971 = CARTESIAN_POINT ( 'NONE',  ( -19.34909385650551883, -8.104110260919579645, 48.81699501597546487 ) ) ;
#3972 = DIRECTION ( 'NONE',  ( 3.549360974551883545E-17, -6.371834667872732552E-18, -1.000000000000000000 ) ) ;
#3973 = CARTESIAN_POINT ( 'NONE',  ( -10.52030486862438430, -16.25576698781496887, 67.97767553346105274 ) ) ;
#3974 = CARTESIAN_POINT ( 'NONE',  ( -18.92057809895272058, -7.919864474132485732, 66.90071783790342863 ) ) ;
#3975 = ORIENTED_EDGE ( 'NONE', *, *, #4504, .T. ) ;
#3976 = CARTESIAN_POINT ( 'NONE',  ( -22.52409385541004383, -9.359200813967481380, 50.49621490983041383 ) ) ;
#3977 = ADVANCED_FACE ( 'NONE', ( #17320 ), #17562, .T. ) ;
#3978 = CARTESIAN_POINT ( 'NONE',  ( -20.72450927900464634, -21.03929139025763106, 58.93003081252663833 ) ) ;
#3979 = CARTESIAN_POINT ( 'NONE',  ( -18.15520726479059022, -21.77104471536384267, 65.64532137700102510 ) ) ;
#3980 = CARTESIAN_POINT ( 'NONE',  ( -22.39459439135063334, -20.35890138417862261, 62.37292654065244335 ) ) ;
#3981 = CARTESIAN_POINT ( 'NONE',  ( -18.30726797983150789, -21.75326897020822514, 68.81514702557041119 ) ) ;
#3982 = CARTESIAN_POINT ( 'NONE',  ( -23.76567461856301122, -18.71936826787876740, 72.90334907938832032 ) ) ;
#3983 = ORIENTED_EDGE ( 'NONE', *, *, #3619, .T. ) ;
#3984 = EDGE_LOOP ( 'NONE', ( #16935, #43466, #37026, #20839 ) ) ;
#3985 = CARTESIAN_POINT ( 'NONE',  ( -11.10470733248389230, -18.75498039752055490, 61.46206112672981448 ) ) ;
#3986 = CARTESIAN_POINT ( 'NONE',  ( -14.91739522418961350, -8.273357693606131491, 57.13534681401838355 ) ) ;
#3987 = ORIENTED_EDGE ( 'NONE', *, *, #21722, .F. ) ;
#3988 = CARTESIAN_POINT ( 'NONE',  ( -21.06635048418738165, -21.30826373965517817, 62.29966805574095901 ) ) ;
#3989 = DIRECTION ( 'NONE',  ( 0.000000000000000000, 1.000000000000000000, 0.000000000000000000 ) ) ;
#3990 = CARTESIAN_POINT ( 'NONE',  ( -11.64964760867527538, -18.76605229218658621, 64.97380311690855592 ) ) ;
#3991 = CARTESIAN_POINT ( 'NONE',  ( -27.42409385541305511, -10.60920654474410618, 79.49999999999998579 ) ) ;
#3992 =( BOUNDED_SURFACE ( )  B_SPLINE_SURFACE ( 3, 1, ( 
 ( #25291, #1666 ),
 ( #32666, #44021 ),
 ( #43768, #16908 ),
 ( #6080, #21361 ),
 ( #5368, #46958 ),
 ( #13205, #20386 ),
 ( #39814, #24806 ) ),
 .UNSPECIFIED., .T., .F., .F. ) 
 B_SPLINE_SURFACE_WITH_KNOTS ( ( 4, 3, 4 ),
 ( 2, 2 ),
 ( 0.000000000000000000, 0.5000000000000000000, 1.000000000000000000 ),
 ( 0.000000000000000000, 1.000000000000000000 ),
 .UNSPECIFIED. ) 
 GEOMETRIC_REPRESENTATION_ITEM ( )  RATIONAL_B_SPLINE_SURFACE ( (
 ( 1.000000000000000000, 1.000000000000000000),
 ( 0.3333333333333335369, 0.3333333333333330373),
 ( 0.3333333333333335369, 0.3333333333333330373),
 ( 1.000000000000000000, 1.000000000000000000),
 ( 0.3333333333333333703, 0.3333333333333333703),
 ( 0.3333333333333333703, 0.3333333333333333703),
 ( 1.000000000000000000, 1.000000000000000000) ) ) 
 REPRESENTATION_ITEM ( '' )  SURFACE ( )  );
#3993 = EDGE_CURVE ( 'NONE', #14949, #28015, #31881, .T. ) ;
#3994 = CARTESIAN_POINT ( 'NONE',  ( -21.59804182614902146, -20.98026282434625500, 72.70941811628220819 ) ) ;
#3995 = LINE ( 'NONE', #37447, #34141 ) ;
#3996 = AXIS2_PLACEMENT_3D ( 'NONE', #37215, #19927, #22466 ) ;
#3997 = CARTESIAN_POINT ( 'NONE',  ( -14.03142060029363236, -8.686249327000295395, 74.21457139832153871 ) ) ;
#3998 = PRODUCT_DEFINITION_SHAPE ( 'NONE', 'NONE',  #48738 ) ;
#3999 = CARTESIAN_POINT ( 'NONE',  ( -16.06050865347321732, -9.480920197610746669, 54.07175714974878389 ) ) ;
#4000 = CARTESIAN_POINT ( 'NONE',  ( -24.38954374850577267, -15.50445147885005071, 73.28838359349398957 ) ) ;
#4001 = CARTESIAN_POINT ( 'NONE',  ( -45.55409385541305767, -14.20920654474410760, 69.94787228701220272 ) ) ;
#4002 = AXIS2_PLACEMENT_3D ( 'NONE', #42528, #203, #45260 ) ;
#4003 = LINE ( 'NONE', #30840, #11372 ) ;
#4004 = DIRECTION ( 'NONE',  ( 2.866981220435666553E-17, -1.000000000000000000, -1.190614954331866791E-16 ) ) ;
#4005 = LINE ( 'NONE', #30357, #14266 ) ;
#4006 = DIRECTION ( 'NONE',  ( -1.000000000000000000, -1.669677910507523057E-21, -6.493791346278465266E-22 ) ) ;
#4007 = EDGE_CURVE ( 'NONE', #4227, #5788, #2788, .T. ) ;
#4008 =( BOUNDED_CURVE ( )  B_SPLINE_CURVE ( 3, ( #26581, #1193, #34193, #16198 ),
 .UNSPECIFIED., .F., .F. ) 
 B_SPLINE_CURVE_WITH_KNOTS ( ( 4, 4 ),
 ( 0.9074455897393631787, 1.000000000000000000 ),
 .UNSPECIFIED. ) 
 CURVE ( )  GEOMETRIC_REPRESENTATION_ITEM ( )  RATIONAL_B_SPLINE_CURVE ( ( 0.6983129098260822953, 0.7760317562606889874, 0.8765941196519948519, 1.000000000000000000 ) ) 
 REPRESENTATION_ITEM ( '' )  );
#4009 = ORIENTED_EDGE ( 'NONE', *, *, #16489, .F. ) ;
#4010 = ORIENTED_EDGE ( 'NONE', *, *, #2376, .F. ) ;
#4011 = CARTESIAN_POINT ( 'NONE',  ( -15.21159385541304410, -8.990409506049202193, 49.61344411288074951 ) ) ;
#4012 = ORIENTED_EDGE ( 'NONE', *, *, #29262, .F. ) ;
#4013 = DIRECTION ( 'NONE',  ( -1.000000000000000000, 0.000000000000000000, 0.000000000000000000 ) ) ;
#4014 = AXIS2_PLACEMENT_3D ( 'NONE', #18043, #18787, #3287 ) ;
#4015 = CARTESIAN_POINT ( 'NONE',  ( -22.07022430586338402, -11.86582892075562157, 53.49999999999995026 ) ) ;
#4016 = EDGE_CURVE ( 'NONE', #21230, #40125, #21752, .T. ) ;
#4017 = AXIS2_PLACEMENT_3D ( 'NONE', #38633, #5155, #16458 ) ;
#4018 = PLANE ( 'NONE',  #38680 ) ;
#4019 = CARTESIAN_POINT ( 'NONE',  ( -17.72612443559818018, -7.765381109175947927, 60.36588690973874094 ) ) ;
#4020 = ORIENTED_EDGE ( 'NONE', *, *, #39997, .T. ) ;
#4021 = ADVANCED_FACE ( 'NONE', ( #24502 ), #20788, .T. ) ;
#4022 = AXIS2_PLACEMENT_3D ( 'NONE', #42502, #4830, #12924 ) ;
#4023 = CARTESIAN_POINT ( 'NONE',  ( -24.36668204746468902, -15.71385111637027165, 73.07474071338100430 ) ) ;
#4024 = CARTESIAN_POINT ( 'NONE',  ( -21.95370832667365235, -13.56094844357179596, 52.02966884056656482 ) ) ;
#4025 = ORIENTED_EDGE ( 'NONE', *, *, #11707, .F. ) ;
#4026 = DIRECTION ( 'NONE',  ( 7.623677598973384647E-06, 4.209792897500673425E-06, -0.9999999999620786673 ) ) ;
#4027 = VECTOR ( 'NONE', #41306, 1000.000000000000000 ) ;
#4028 = DIRECTION ( 'NONE',  ( -1.053901171479178877E-05, 6.708308826365502595E-06, -0.9999999999219638669 ) ) ;
#4029 = EDGE_LOOP ( 'NONE', ( #6997, #34854, #3733, #46267 ) ) ;
#4030 = DIRECTION ( 'NONE',  ( 1.000000000000000000, 2.866981220435666553E-17, 0.000000000000000000 ) ) ;
#4031 = DIRECTION ( 'NONE',  ( 0.02843338833657542419, -0.4463087971659328024, 0.8944271909999157444 ) ) ;
#4032 = CARTESIAN_POINT ( 'NONE',  ( -12.23160957677214178, -12.95553921741658243, 53.88362224778187226 ) ) ;
#4033 = ORIENTED_EDGE ( 'NONE', *, *, #591, .F. ) ;
#4034 = CARTESIAN_POINT ( 'NONE',  ( -19.74917416150487171, -21.41189869944521362, 69.23482485975905831 ) ) ;
#4035 = LINE ( 'NONE', #26680, #15536 ) ;
#4036 = AXIS2_PLACEMENT_3D ( 'NONE', #41677, #15065, #45146 ) ;
#4037 = EDGE_CURVE ( 'NONE', #22481, #28514, #6504, .T. ) ;
#4038 = FACE_OUTER_BOUND ( 'NONE', #2610, .T. ) ;
#4039 = PLANE ( 'NONE',  #145 ) ;
#4040 = VERTEX_POINT ( 'NONE', #43945 ) ;
#4041 = CARTESIAN_POINT ( 'NONE',  ( -21.32332200014554857, -12.20934075487643966, 49.52966884056655772 ) ) ;
#4042 = CARTESIAN_POINT ( 'NONE',  ( -17.42409385541300892, -14.80920654474439679, 47.99999999999994316 ) ) ;
#4043 = CARTESIAN_POINT ( 'NONE',  ( -16.13263948075386978, -7.878200451182638453, 63.68483172840383588 ) ) ;
#4044 = ADVANCED_FACE ( 'NONE', ( #33054 ), #5781, .T. ) ;
#4045 = DIRECTION ( 'NONE',  ( 1.616182858256118783E-16, 0.003028072113822189229, -0.9999954153791275058 ) ) ;
#4046 = CARTESIAN_POINT ( 'NONE',  ( -17.65810221059773610, -7.762793303104816189, 63.56529088875731759 ) ) ;
#4047 = CARTESIAN_POINT ( 'NONE',  ( -22.63674339536608926, -20.13198319316658313, 69.43063894133570102 ) ) ;
#4048 = EDGE_CURVE ( 'NONE', #30036, #14018, #22591, .T. ) ;
#4049 = ADVANCED_FACE ( 'NONE', ( #9478 ), #13379, .T. ) ;
#4050 = CARTESIAN_POINT ( 'NONE',  ( -19.37409385650551741, -9.792211528768504536, 50.49490371617623197 ) ) ;
#4051 = EDGE_CURVE ( 'NONE', #34971, #27190, #42486, .T. ) ;
#4052 = VECTOR ( 'NONE', #4155, 1000.000000000000000 ) ;
#4053 = ORIENTED_EDGE ( 'NONE', *, *, #46462, .F. ) ;
#4054 = B_SPLINE_CURVE_WITH_KNOTS ( 'NONE', 1,
 ( #34100, #5057 ),
 .UNSPECIFIED., .F., .F.,
 ( 2, 2 ),
 ( 0.000000000000000000, 1.000000000000000000 ),
 .UNSPECIFIED. ) ;
#4055 = CARTESIAN_POINT ( 'NONE',  ( -24.35037712455101655, -13.45216126592925754, 62.97697330661279835 ) ) ;
#4056 = CARTESIAN_POINT ( 'NONE',  ( -21.09284385759799108, -8.630756214087126565, 51.74842643355248129 ) ) ;
#4057 = VERTEX_POINT ( 'NONE', #3284 ) ;
#4058 = CARTESIAN_POINT ( 'NONE',  ( -11.33476867595667770, -19.10151316506851416, 68.40185013497388411 ) ) ;
#4059 = CARTESIAN_POINT ( 'NONE',  ( -24.47507746028116671, -14.61665733240941378, 59.45120272392967564 ) ) ;
#4060 = CARTESIAN_POINT ( 'NONE',  ( -14.71062180296534017, -21.26200528251204247, 58.46617879205846435 ) ) ;
#4061 = ORIENTED_EDGE ( 'NONE', *, *, #37204, .T. ) ;
#4062 = DIRECTION ( 'NONE',  ( 3.071710424422018668E-17, -6.404604876783312462E-16, -1.000000000000000000 ) ) ;
#4063 = CARTESIAN_POINT ( 'NONE',  ( -24.42340909951234096, -14.70711335020210520, 59.31588370434493385 ) ) ;
#4064 = STYLED_ITEM ( 'NONE', ( #7403 ), #32048 ) ;
#4065 = DIRECTION ( 'NONE',  ( 2.866981220435666553E-17, -1.000000000000000000, -1.190614954331866791E-16 ) ) ;
#4066 = VERTEX_POINT ( 'NONE', #29879 ) ;
#4067 = CARTESIAN_POINT ( 'NONE',  ( -13.91784385650551670, -9.790100578890868377, 49.79778022625163203 ) ) ;
#4068 = AXIS2_PLACEMENT_3D ( 'NONE', #38487, #35277, #20029 ) ;
#4069 = DIRECTION ( 'NONE',  ( -3.071710424422018668E-17, 6.404604876783312462E-16, 1.000000000000000000 ) ) ;
#4070 = CARTESIAN_POINT ( 'NONE',  ( -21.37409385759799108, -6.859212275519751323, 50.50378509014259265 ) ) ;
#4071 = FACE_OUTER_BOUND ( 'NONE', #19356, .T. ) ;
#4072 = CARTESIAN_POINT ( 'NONE',  ( -13.62949042321701398, -8.926946430974666669, 56.96967755885751217 ) ) ;
#4073 = VECTOR ( 'NONE', #48266, 1000.000000000000000 ) ;
#4074 = ORIENTED_EDGE ( 'NONE', *, *, #30635, .T. ) ;
#4075 = VERTEX_POINT ( 'NONE', #11638 ) ;
#4076 = CARTESIAN_POINT ( 'NONE',  ( -15.18659385650551386, -9.302874398569244363, 51.68646062012417985 ) ) ;
#4077 = EDGE_CURVE ( 'NONE', #41843, #9176, #45417, .T. ) ;
#4078 = CARTESIAN_POINT ( 'NONE',  ( -10.44532783130100562, -14.26439015257133924, 61.10924436523676917 ) ) ;
#4079 = AXIS2_PLACEMENT_3D ( 'NONE', #4309, #857, #15608 ) ;
#4080 = CARTESIAN_POINT ( 'NONE',  ( -15.35534385650551847, -7.417179338643134834, 52.18511593390279302 ) ) ;
#4081 = CARTESIAN_POINT ( 'NONE',  ( -10.77075480930259133, -16.98888344060621947, 61.38572962699099378 ) ) ;
#4082 = CARTESIAN_POINT ( 'NONE',  ( -15.25801600794807555, -21.93814553200309092, 72.23230793488828283 ) ) ;
#4083 = CIRCLE ( 'NONE', #45778, 2.000000000000000444 ) ;
#4085 = CARTESIAN_POINT ( 'NONE',  ( -15.62222905942471840, -7.993050613273783966, 70.89517703929612935 ) ) ;
#4084 = B_SPLINE_CURVE_WITH_KNOTS ( 'NONE', 3,
 ( #40145, #18198, #33205, #2222, #13769, #20945, #32508, #9638, #17233, #43850 ),
 .UNSPECIFIED., .F., .F.,
 ( 4, 2, 2, 2, 4 ),
 ( 0.000000000000000000, 0.2500000000000000000, 0.5000000000000000000, 0.7500000000000000000, 1.000000000000000000 ),
 .UNSPECIFIED. ) ;
#4086 = CARTESIAN_POINT ( 'NONE',  ( -13.73677046600794149, -20.82228291470529058, 61.72466036792861388 ) ) ;
#4087 = ORIENTED_EDGE ( 'NONE', *, *, #36552, .T. ) ;
#4088 = DIRECTION ( 'NONE',  ( 2.584300424743464895E-08, 1.497441459180121760E-06, -0.9999999999988785637 ) ) ;
#4089 = B_SPLINE_CURVE_WITH_KNOTS ( 'NONE', 3,
 ( #46272, #47240, #13000, #5880, #9817, #1442, #16456, #24833, #1931, #43556 ),
 .UNSPECIFIED., .F., .F.,
 ( 4, 2, 2, 2, 4 ),
 ( 0.000000000000000000, 0.2500000000000000000, 0.5000000000000000000, 0.7500000000000000000, 1.000000000000000000 ),
 .UNSPECIFIED. ) ;
#4090 = VERTEX_POINT ( 'NONE', #45156 ) ;
#4091 =( GEOMETRIC_REPRESENTATION_CONTEXT ( 3 ) GLOBAL_UNCERTAINTY_ASSIGNED_CONTEXT ( ( #6084 ) ) GLOBAL_UNIT_ASSIGNED_CONTEXT ( ( #6365, #25083, #31981 ) ) REPRESENTATION_CONTEXT ( 'NONE', 'WORKASPACE' ) );
#4092 = CARTESIAN_POINT ( 'NONE',  ( -12.54429422870864741, -9.179802802619546398, 74.51911777589955932 ) ) ;
#4093 = CARTESIAN_POINT ( 'NONE',  ( -20.28216670725803894, -8.419192670066959039, 67.06638753379743889 ) ) ;
#4094 = CARTESIAN_POINT ( 'NONE',  ( -19.18086540149941399, -19.15397765319887569, 52.02966884056656482 ) ) ;
#4095 = CARTESIAN_POINT ( 'NONE',  ( -46.47622156840087371, -14.20920654474410760, 70.13000000000000966 ) ) ;
#4096 = AXIS2_PLACEMENT_3D ( 'NONE', #18266, #14315, #33271 ) ;
#4097 = ORIENTED_EDGE ( 'NONE', *, *, #44078, .F. ) ;
#4098 = CARTESIAN_POINT ( 'NONE',  ( -10.35611353805053980, -12.45393147150008772, 61.05499485166044593 ) ) ;
#4099 = DIRECTION ( 'NONE',  ( 0.7971031148784507581, -0.6038432116460915600, 6.916509187980650173E-08 ) ) ;
#4100 = CARTESIAN_POINT ( 'NONE',  ( -19.83890857264518104, -18.82566669410956806, 49.52966884056656482 ) ) ;
#4101 = ORIENTED_EDGE ( 'NONE', *, *, #3409, .F. ) ;
#4102 = CARTESIAN_POINT ( 'NONE',  ( -19.56968442187927693, -21.94361132924262492, 62.18777784925811147 ) ) ;
#4103 = LINE ( 'NONE', #41508, #10098 ) ;
#4104 = DIRECTION ( 'NONE',  ( -3.071710424422018668E-17, 6.404604876783312462E-16, 1.000000000000000000 ) ) ;
#4105 = FACE_OUTER_BOUND ( 'NONE', #3928, .T. ) ;
#4106 = PRODUCT_CONTEXT ( 'NONE', #18033, 'mechanical' ) ;
#4107 = ORIENTED_EDGE ( 'NONE', *, *, #1319, .F. ) ;
#4108 = EDGE_CURVE ( 'NONE', #9874, #48505, #21012, .T. ) ;
#4109 = ADVANCED_FACE ( 'NONE', ( #30131 ), #41195, .F. ) ;
#4110 = DIRECTION ( 'NONE',  ( 0.9087012777736581670, -0.4174469879787382487, -4.853707507795077342E-09 ) ) ;
#4111 = DIRECTION ( 'NONE',  ( -3.071710424422018668E-17, 6.404604876783312462E-16, 1.000000000000000000 ) ) ;
#4112 = CARTESIAN_POINT ( 'NONE',  ( -15.20275948037936864, -21.92046911484317917, 68.75309815756419596 ) ) ;
#4113 = CARTESIAN_POINT ( 'NONE',  ( -42.30718209070717961, -14.80920654474416764, 63.93529411764704662 ) ) ;
#4114 = ORIENTED_EDGE ( 'NONE', *, *, #28826, .F. ) ;
#4115 = FACE_OUTER_BOUND ( 'NONE', #30233, .T. ) ;
#4116 = VERTEX_POINT ( 'NONE', #26420 ) ;
#4117 = LINE ( 'NONE', #30703, #47847 ) ;
#4118 = CARTESIAN_POINT ( 'NONE',  ( -12.26752988409003287, -16.72227946798956211, 53.49899999999994549 ) ) ;
#4119 = CARTESIAN_POINT ( 'NONE',  ( -10.61330258792943226, -12.98832159324076052, 68.03832347271725212 ) ) ;
#4120 = EDGE_LOOP ( 'NONE', ( #808, #33790, #24335, #44301 ) ) ;
#4121 = EDGE_CURVE ( 'NONE', #11700, #14807, #22242, .T. ) ;
#4122 = EDGE_CURVE ( 'NONE', #16141, #10355, #24979, .T. ) ;
#4123 = ORIENTED_EDGE ( 'NONE', *, *, #20671, .T. ) ;
#4124 = ORIENTED_EDGE ( 'NONE', *, *, #37879, .T. ) ;
#4125 = VERTEX_POINT ( 'NONE', #40699 ) ;
#4126 = FACE_OUTER_BOUND ( 'NONE', #42816, .T. ) ;
#4127 = CARTESIAN_POINT ( 'NONE',  ( -23.34481640033245853, -18.63641755246779752, 69.59371984262205046 ) ) ;
#4128 = CARTESIAN_POINT ( 'NONE',  ( -12.95250271175661183, -20.26353575427058828, 71.69165012371371404 ) ) ;
#4129 = CYLINDRICAL_SURFACE ( 'NONE', #8288, 0.1500000000000031586 ) ;
#4130 = CARTESIAN_POINT ( 'NONE',  ( -19.09284385541296558, -8.630756214087181633, 51.74842643355260918 ) ) ;
#4131 = CARTESIAN_POINT ( 'NONE',  ( -14.04013919049901560, -8.171999524408169790, 70.77311711151845941 ) ) ;
#4132 = CARTESIAN_POINT ( 'NONE',  ( -12.51424385636291170, -20.41247444060362071, 71.99991975137920974 ) ) ;
#4133 = ORIENTED_EDGE ( 'NONE', *, *, #28391, .T. ) ;
#4134 = ORIENTED_EDGE ( 'NONE', *, *, #41325, .F. ) ;
#4135 = CARTESIAN_POINT ( 'NONE',  ( -17.52853272358826686, -7.759682304905023642, 63.83584969886392457 ) ) ;
#4136 = EDGE_CURVE ( 'NONE', #46865, #24126, #45385, .T. ) ;
#4137 = CARTESIAN_POINT ( 'NONE',  ( -22.54704564128305222, -20.21849264563443782, 65.86455114034160374 ) ) ;
#4138 = CARTESIAN_POINT ( 'NONE',  ( -10.51635384603322976, -15.94466201910895897, 67.99384522443050116 ) ) ;
#4139 = CARTESIAN_POINT ( 'NONE',  ( -23.37999588001404661, -18.58199455739222827, 69.57899840282863124 ) ) ;
#4140 = ORIENTED_EDGE ( 'NONE', *, *, #45296, .F. ) ;
#4141 =( BOUNDED_CURVE ( )  B_SPLINE_CURVE ( 3, ( #32381, #47401, #13637, #28677 ),
 .UNSPECIFIED., .F., .F. ) 
 B_SPLINE_CURVE_WITH_KNOTS ( ( 4, 4 ),
 ( 0.4074455897393696180, 0.5000000000000000000 ),
 .UNSPECIFIED. ) 
 CURVE ( )  GEOMETRIC_REPRESENTATION_ITEM ( )  RATIONAL_B_SPLINE_CURVE ( ( 0.6983129098261098289, 0.7760317562606982023, 0.8765941196519907441, 0.9999999999999770184 ) ) 
 REPRESENTATION_ITEM ( '' )  );
#4142 = CARTESIAN_POINT ( 'NONE',  ( -17.34909385650551883, -8.104110260919579645, 48.81699501597546487 ) ) ;
#4143 = EDGE_LOOP ( 'NONE', ( #30258, #16228, #22628, #21162, #7820 ) ) ;
#4144 = CARTESIAN_POINT ( 'NONE',  ( -15.00927913818083859, -10.79274639537912606, 52.02966884056656482 ) ) ;
#4145 = CARTESIAN_POINT ( 'NONE',  ( -10.47141612868932192, -15.99879407189726699, 71.74750680274701153 ) ) ;
#4146 = CARTESIAN_POINT ( 'NONE',  ( -22.01964724813734620, -15.72799447708766962, 49.52966884056655772 ) ) ;
#4147 = ORIENTED_EDGE ( 'NONE', *, *, #32968, .T. ) ;
#4148 = CARTESIAN_POINT ( 'NONE',  ( -20.31649657898477912, -7.943510300654241796, 70.43595776394847974 ) ) ;
#4149 =( BOUNDED_CURVE ( )  B_SPLINE_CURVE ( 2, ( #25431, #10892, #11143, #30112, #33270, #15053, #18265, #29607, #22464 ),
 .UNSPECIFIED., .F., .F. ) 
 B_SPLINE_CURVE_WITH_KNOTS ( ( 3, 2, 2, 2, 3 ),
 ( 0.1666666666666666297, 0.1770833333333332871, 0.1874999999999998890, 0.1979166666666665186, 0.2083333333333331761 ),
 .UNSPECIFIED. ) 
 CURVE ( )  GEOMETRIC_REPRESENTATION_ITEM ( )  RATIONAL_B_SPLINE_CURVE ( ( 1.000000000000000222, 0.9238795325112865164, 1.000000000000000000, 0.9238795325112867385, 1.000000000000000000, 0.9238795325112867385, 1.000000000000000000, 0.9238795325112879597, 0.9999999999999987788 ) ) 
 REPRESENTATION_ITEM ( '' )  );
#4150 = DIRECTION ( 'NONE',  ( 1.000000000000000000, -4.164305804376849172E-17, 1.614929280266638808E-16 ) ) ;
#4151 = CARTESIAN_POINT ( 'NONE',  ( -14.24626305875727184, -11.36469298288595731, 49.52966884056655772 ) ) ;
#4152 = ORIENTED_EDGE ( 'NONE', *, *, #35530, .T. ) ;
#4153 = DIRECTION ( 'NONE',  ( -0.6172023957221239865, -0.7799807200343535918, 0.1033986416233890343 ) ) ;
#4154 = DIRECTION ( 'NONE',  ( 0.000000000000000000, 0.000000000000000000, -1.000000000000000000 ) ) ;
#4155 = DIRECTION ( 'NONE',  ( 1.000000000000000000, 2.866981220435666553E-17, 0.000000000000000000 ) ) ;
#4156 = ORIENTED_EDGE ( 'NONE', *, *, #27277, .T. ) ;
#4157 = CARTESIAN_POINT ( 'NONE',  ( -10.49862840407593367, -15.82799419795606966, 64.80771590052736997 ) ) ;
#4158 =( BOUNDED_CURVE ( )  B_SPLINE_CURVE ( 3, ( #9233, #12428, #12190, #27697 ),
 .UNSPECIFIED., .F., .F. ) 
 B_SPLINE_CURVE_WITH_KNOTS ( ( 4, 4 ),
 ( 0.9074455897393693959, 1.000000000000000000 ),
 .UNSPECIFIED. ) 
 CURVE ( )  GEOMETRIC_REPRESENTATION_ITEM ( )  RATIONAL_B_SPLINE_CURVE ( ( 0.6983129098261139367, 0.7760317562607162989, 0.8765941196520116163, 1.000000000000000000 ) ) 
 REPRESENTATION_ITEM ( '' )  );
#4159 = EDGE_LOOP ( 'NONE', ( #37727, #16692 ) ) ;
#4160 = CARTESIAN_POINT ( 'NONE',  ( -10.54994933093899867, -13.24305344519376959, 71.49356453765415154 ) ) ;
#4161 = CARTESIAN_POINT ( 'NONE',  ( -23.84743916260113039, -11.89450597454958114, 63.25218314574954093 ) ) ;
#4162 = VERTEX_POINT ( 'NONE', #21998 ) ;
#4163 = EDGE_CURVE ( 'NONE', #15682, #37990, #15414, .T. ) ;
#4164 = CARTESIAN_POINT ( 'NONE',  ( 18.57132275349405504, 1.971407400791296949, 51.78906405069922414 ) ) ;
#4165 = CARTESIAN_POINT ( 'NONE',  ( -23.78500256881436314, -11.88707711785523635, 59.48235732566631384 ) ) ;
#4166 = CARTESIAN_POINT ( 'NONE',  ( -12.45873566688477929, -9.804017486950373339, 57.10407583662104258 ) ) ;
#4167 = VERTEX_POINT ( 'NONE', #19271 ) ;
#4168 = CARTESIAN_POINT ( 'NONE',  ( -11.29134393598116937, -11.33126488396075260, 64.16354160640879911 ) ) ;
#4169 = CARTESIAN_POINT ( 'NONE',  ( -22.79960237261627398, -9.650942640399760464, 73.66656521964461035 ) ) ;
#4170 = CARTESIAN_POINT ( 'NONE',  ( -11.96671518932367029, -9.737692337828448785, 60.66579796421850546 ) ) ;
#4171 = VERTEX_POINT ( 'NONE', #34276 ) ;
#4172 = CARTESIAN_POINT ( 'NONE',  ( -19.22943344864035353, -8.044691675300194689, 63.65919177093534387 ) ) ;
#4173 = EDGE_CURVE ( 'NONE', #43582, #4699, #23122, .T. ) ;
#4174 = CARTESIAN_POINT ( 'NONE',  ( -23.57312343282865896, -11.36065554106722786, 69.89210769048611382 ) ) ;
#4175 = EDGE_LOOP ( 'NONE', ( #41006, #28427 ) ) ;
#4176 = ORIENTED_EDGE ( 'NONE', *, *, #43070, .T. ) ;
#4177 = EDGE_CURVE ( 'NONE', #12172, #20147, #46980, .T. ) ;
#4178 = CARTESIAN_POINT ( 'NONE',  ( -24.84861529636215849, -14.19299288461673747, 69.75936971009964793 ) ) ;
#4179 = CARTESIAN_POINT ( 'NONE',  ( -19.17437844398820701, -7.979623566120205957, 63.44561363416070776 ) ) ;
#4180 = CARTESIAN_POINT ( 'NONE',  ( -14.07761608144266674, -20.95746532167037302, 71.92607703845176559 ) ) ;
#4181 = VERTEX_POINT ( 'NONE', #14813 ) ;
#4182 = CARTESIAN_POINT ( 'NONE',  ( -21.28659385650551528, -9.302874398569244363, 51.68646062012417985 ) ) ;
#4183 = EDGE_CURVE ( 'NONE', #28650, #44593, #38358, .T. ) ;
#4184 = CARTESIAN_POINT ( 'NONE',  ( -10.40257400440372315, -14.13711964566031654, 57.65644799979391166 ) ) ;
#4185 = CARTESIAN_POINT ( 'NONE',  ( -14.17409385759798823, -6.859212275519751323, 50.50378509014259265 ) ) ;
#4186 = DIRECTION ( 'NONE',  ( -0.7150252244155669290, 0.6990986543038602008, -7.133781456731120165E-17 ) ) ;
#4187 = ORIENTED_EDGE ( 'NONE', *, *, #31377, .F. ) ;
#4188 = LINE ( 'NONE', #19685, #17876 ) ;
#4189 = VECTOR ( 'NONE', #3080, 1000.000000000000000 ) ;
#4190 = CARTESIAN_POINT ( 'NONE',  ( -10.57550014152487705, -13.13548074022098433, 71.21388402457256461 ) ) ;
#4191 = LINE ( 'NONE', #34934, #1647 ) ;
#4192 = ORIENTED_EDGE ( 'NONE', *, *, #45315, .F. ) ;
#4193 = ORIENTED_EDGE ( 'NONE', *, *, #20444, .F. ) ;
#4194 = DIRECTION ( 'NONE',  ( 3.913797943140854342E-06, 1.965591624649253694E-06, 0.9999999999904093384 ) ) ;
#4195 = FACE_OUTER_BOUND ( 'NONE', #36114, .T. ) ;
#4196 = CARTESIAN_POINT ( 'NONE',  ( -22.56207008003183745, -19.63703213565221617, 72.92928497383269359 ) ) ;
#4197 = CARTESIAN_POINT ( 'NONE',  ( -20.03282965983824226, -21.84088468745754597, 47.99999999999994316 ) ) ;
#4198 = VERTEX_POINT ( 'NONE', #806 ) ;
#4199 = CARTESIAN_POINT ( 'NONE',  ( -23.54066400932483205, -11.40515459557274447, 66.53100539013419734 ) ) ;
#4200 = CARTESIAN_POINT ( 'NONE',  ( -14.24059955017480306, -8.515543114936868108, 67.14486463900426827 ) ) ;
#4201 = ORIENTED_EDGE ( 'NONE', *, *, #34363, .T. ) ;
#4202 = CARTESIAN_POINT ( 'NONE',  ( -22.67603917253425294, -10.10156321767594179, 73.89649722025401957 ) ) ;
#4203 = CARTESIAN_POINT ( 'NONE',  ( -21.29196722032537537, -20.70380199363842877, 72.53918572867779346 ) ) ;
#4204 = CARTESIAN_POINT ( 'NONE',  ( -13.85534475943383370, -8.269504983759647487, 74.24308752109034515 ) ) ;
#4205 = EDGE_CURVE ( 'NONE', #39884, #41525, #35926, .T. ) ;
#4206 = VERTEX_POINT ( 'NONE', #4747 ) ;
#4207 = CARTESIAN_POINT ( 'NONE',  ( -21.76140000860026191, -9.313236413093783028, 66.88979917059124602 ) ) ;
#4208 = ORIENTED_EDGE ( 'NONE', *, *, #22295, .T. ) ;
#4209 = CARTESIAN_POINT ( 'NONE',  ( -45.92409385541305511, -14.80920654474410725, 70.50000000000000000 ) ) ;
#4210 = B_SPLINE_CURVE_WITH_KNOTS ( 'NONE', 3,
 ( #22145, #10571, #6873, #41092, #28794, #47747, #44317, #2921, #25824, #29033 ),
 .UNSPECIFIED., .F., .F.,
 ( 4, 2, 2, 2, 4 ),
 ( 0.1272669073658634353, 0.2522669073463360001, 0.3772669073268085649, 0.5022669073072811852, 0.6272669072877536944 ),
 .UNSPECIFIED. ) ;
#4211 = CARTESIAN_POINT ( 'NONE',  ( -19.22579631480732587, -21.57336711704104104, 58.82507384991394872 ) ) ;
#4212 = EDGE_LOOP ( 'NONE', ( #44413, #23588, #26598, #14037, #39097 ) ) ;
#4213 = FACE_OUTER_BOUND ( 'NONE', #7648, .T. ) ;
#4214 = CARTESIAN_POINT ( 'NONE',  ( 8.575906144586951996, -8.109963562772117385, 50.74999885384509923 ) ) ;
#4215 = AXIS2_PLACEMENT_3D ( 'NONE', #30627, #11904, #23474 ) ;
#4216 = CARTESIAN_POINT ( 'NONE',  ( -19.91159385650551528, -6.922745924619793101, 51.69366785382590024 ) ) ;
#4217 = CARTESIAN_POINT ( 'NONE',  ( -17.59048613883335932, -21.80850830400060403, 58.63383171954600215 ) ) ;
#4218 = LINE ( 'NONE', #45596, #10366 ) ;
#4219 = DIRECTION ( 'NONE',  ( 3.413470714839332458E-33, -1.190614954331866791E-16, 1.000000000000000000 ) ) ;
#4220 = ORIENTED_EDGE ( 'NONE', *, *, #37408, .F. ) ;
#4221 = CARTESIAN_POINT ( 'NONE',  ( -23.19916440516392697, -19.59445054535707698, 47.99999999999994316 ) ) ;
#4222 = CARTESIAN_POINT ( 'NONE',  ( -13.18473975798692877, -20.93551490194142062, 58.23145353898504339 ) ) ;
#4223 = DIRECTION ( 'NONE',  ( -1.000000000000000000, 0.000000000000000000, 0.000000000000000000 ) ) ;
#4224 = DIRECTION ( 'NONE',  ( 1.000000000000000000, -4.164305804376849172E-17, 1.614929280266638808E-16 ) ) ;
#4225 = CARTESIAN_POINT ( 'NONE',  ( -17.58219478024370730, -20.05682544264153933, 52.02966884056656482 ) ) ;
#4226 = ORIENTED_EDGE ( 'NONE', *, *, #31002, .F. ) ;
#4227 = VERTEX_POINT ( 'NONE', #38951 ) ;
#4228 = ADVANCED_FACE ( 'NONE', ( #12131 ), #6130, .T. ) ;
#4229 = CARTESIAN_POINT ( 'NONE',  ( -24.48129518141919903, -12.42204491826083590, 73.44214348908371903 ) ) ;
#4230 = CARTESIAN_POINT ( 'NONE',  ( -14.72744631621160494, -8.295007313424175521, 60.60524229057013201 ) ) ;
#4231 = ORIENTED_EDGE ( 'NONE', *, *, #1889, .T. ) ;
#4232 = LINE ( 'NONE', #33756, #6022 ) ;
#4233 = CARTESIAN_POINT ( 'NONE',  ( -15.19548991633585011, -21.91815178685365595, 68.76088227238139439 ) ) ;
#4234 = CARTESIAN_POINT ( 'NONE',  ( -21.26159385759799036, -7.228003583438117552, 51.38655588711986155 ) ) ;
#4235 = EDGE_CURVE ( 'NONE', #31166, #20442, #16532, .T. ) ;
#4236 = CARTESIAN_POINT ( 'NONE',  ( -45.92409385541306222, -14.38986189584960051, 70.50000000000000000 ) ) ;
#4237 = CARTESIAN_POINT ( 'NONE',  ( -24.39823031370633544, -14.19330659245935422, 73.35101391479588528 ) ) ;
#4238 = CARTESIAN_POINT ( 'NONE',  ( -23.59011972508282895, -18.99064774873246009, 65.94576636911624234 ) ) ;
#4239 = CARTESIAN_POINT ( 'NONE',  ( -14.06269433208033171, -8.668953365929850108, 74.19954661247773231 ) ) ;
#4240 = EDGE_CURVE ( 'NONE', #12698, #19689, #2918, .T. ) ;
#4241 = CARTESIAN_POINT ( 'NONE',  ( -22.75539019595754908, -10.19575032747719412, 66.82710158566565894 ) ) ;
#4242 = SURFACE_SIDE_STYLE ('',( #23437 ) ) ;
#4243 = CARTESIAN_POINT ( 'NONE',  ( -24.12651600458584511, -12.62191667979047338, 73.25697658996379857 ) ) ;
#4244 = DIRECTION ( 'NONE',  ( 6.059369597461991776E-06, -3.309764069070163182E-06, -0.9999999999761647329 ) ) ;
#4245 = CARTESIAN_POINT ( 'NONE',  ( -11.92202137443377907, -10.38855435516889081, 64.18481546414660954 ) ) ;
#4246 = EDGE_CURVE ( 'NONE', #39133, #47884, #5298, .T. ) ;
#4247 = CARTESIAN_POINT ( 'NONE',  ( -23.78676244964941233, -10.93361294341921131, 73.54688584860882372 ) ) ;
#4248 = ORIENTED_EDGE ( 'NONE', *, *, #38402, .F. ) ;
#4249 = ORIENTED_EDGE ( 'NONE', *, *, #21501, .T. ) ;
#4250 = CARTESIAN_POINT ( 'NONE',  ( -12.12884284833700299, -9.568708778729794417, 57.23935532548082961 ) ) ;
#4251 = B_SPLINE_CURVE_WITH_KNOTS ( 'NONE', 3,
 ( #46765, #4673, #27800, #8621, #19935, #13009, #42828, #9101, #5162, #31253 ),
 .UNSPECIFIED., .F., .F.,
 ( 4, 2, 2, 2, 4 ),
 ( 0.000000000000000000, 0.2500000000000000000, 0.5000000000000000000, 0.7500000000000000000, 1.000000000000000000 ),
 .UNSPECIFIED. ) ;
#4252 = ORIENTED_EDGE ( 'NONE', *, *, #4988, .F. ) ;
#4253 = DIRECTION ( 'NONE',  ( -3.071710424422018668E-17, 6.404604876783312462E-16, 1.000000000000000000 ) ) ;
#4254 = AXIS2_PLACEMENT_3D ( 'NONE', #39696, #28617, #43647 ) ;
#4255 = CARTESIAN_POINT ( 'NONE',  ( -13.67313477037754232, -20.71991182390168618, 65.27012384153809421 ) ) ;
#4256 = CARTESIAN_POINT ( 'NONE',  ( -16.64476583608805882, -21.82402065185451079, 72.30976097999173646 ) ) ;
#4257 = EDGE_LOOP ( 'NONE', ( #5905, #13126, #4709 ) ) ;
#4258 = B_SPLINE_CURVE_WITH_KNOTS ( 'NONE', 3,
 ( #31204, #19151, #26792, #46227, #12488, #5109, #41817, #8093, #23103, #38095 ),
 .UNSPECIFIED., .F., .F.,
 ( 4, 2, 2, 2, 4 ),
 ( 0.6272669072877604668, 0.7522669073072876245, 0.8772669073268148932, 1.002266907346342162, 1.127266907365869208 ),
 .UNSPECIFIED. ) ;
#4259 = PLANE ( 'NONE',  #38308 ) ;
#4260 = ORIENTED_EDGE ( 'NONE', *, *, #44885, .T. ) ;
#4261 = CARTESIAN_POINT ( 'NONE',  ( -11.46044050272623416, -11.04924139602722200, 57.20903212151936401 ) ) ;
#4262 = EDGE_CURVE ( 'NONE', #16853, #24967, #27148, .T. ) ;
#4263 = CARTESIAN_POINT ( 'NONE',  ( -10.37394849890712401, -14.76283852923608286, 71.61310637325181006 ) ) ;
#4264 = ORIENTED_EDGE ( 'NONE', *, *, #22170, .F. ) ;
#4265 = DIRECTION ( 'NONE',  ( 0.9687793358424821033, -0.2479245821708679909, 0.000000000000000000 ) ) ;
#4266 = CARTESIAN_POINT ( 'NONE',  ( -11.09636497276514966, -11.81291589161553901, 74.63010272337737661 ) ) ;
#4267 = CARTESIAN_POINT ( 'NONE',  ( -10.41569439578338496, -15.57669382292980131, 61.05261153187079515 ) ) ;
#4268 = EDGE_LOOP ( 'NONE', ( #25808, #7829 ) ) ;
#4269 = CARTESIAN_POINT ( 'NONE',  ( -22.28468842640967651, -19.91619389767071269, 65.98949666203347419 ) ) ;
#4270 = CARTESIAN_POINT ( 'NONE',  ( -50.42509385541305988, -8.109206544744111511, 51.54999999999998295 ) ) ;
#4271 =( BOUNDED_CURVE ( )  B_SPLINE_CURVE ( 2, ( #13801, #40180, #6452, #17742, #32772, #29087, #10392, #43403, #19224, #29826, #6920, #44600, #21939, #7920, #14509, #18230, #36940, #15015, #514, #40894, #3225, #29569, #3717, #30567, #22940, #34227, #22429, #26365, #41635, #7424, #37929, #22192, #37422, #33479, #45593, #44854, #11350, #45103, #30326, #284, #10854, #25879, #25628, #18720, #7183, #33238, #31, #15262, #33986, #37177, #3463, #15502, #18472, #48519, #14754, #30079, #11108, #18981, #4216, #26131, #41143, #40642, #33734, #41380, #48278, #7673, #22678, #37679, #3971, #45337, #11590, #26616, #8387, #27338, #23411, #4445, #5424, #35201, #41884, #12316, #38404, #23662, #12561, #761, #31042, #15755, #42121, #1226, #15996, #16721, #12797, #27822, #46056, #34958, #42851, #42367, #12083, #20446, #8640, #20189, #30809, #45826, #31763, #35445, #9119, #16231, #19461, #38664, #24137, #5181, #27583, #31522, #4693, #19956, #4947, #38162, #1469, #16485, #19718, #42621, #27095, #39141, #1729, #31274, #8158, #34727, #23171, #11843, #1000, #34470, #46304, #8882, #26870, #23902, #38902, #46556, #5675, #17459, #16960, #32003, #43341, #47514, #13981, #28558, #29027, #9615, #43586, #5903, #17927, #2200, #32486, #13747, #2682, #21417, #35677, #28790, #9363, #43828, #9845, #47018, #17205, #36401, #6387, #28320, #1959, #40356, #13262, #24629, #39632, #36161, #20921, #40124, #44080, #35923, #32257, #47274, #10080, #17690, #24860 ),
 .UNSPECIFIED., .F., .F. ) 
 B_SPLINE_CURVE_WITH_KNOTS ( ( 3, 2, 2, 2, 2, 2, 2, 2, 2, 2, 2, 2, 2, 2, 2, 2, 2, 2, 2, 2, 2, 2, 2, 2, 2, 2, 2, 2, 2, 2, 2, 2, 2, 2, 2, 2, 2, 2, 2, 2, 2, 2, 2, 2, 2, 2, 2, 2, 2, 2, 2, 2, 2, 2, 2, 2, 2, 2, 2, 2, 2, 2, 2, 2, 2, 2, 2, 2, 2, 2, 2, 2, 2, 2, 2, 2, 2, 2, 2, 2, 2, 2, 2, 2, 2, 2, 2, 2, 2, 3 ),
 ( 0.000000000000000000, 0.01125025289161911933, 0.02250050578323823866, 0.03375075867485735626, 0.04500101156647647732, 0.05625126445809559839, 0.06750151734971471251, 0.07875177024133384052, 0.09000202313295295464, 0.1012522760245720688, 0.1125025289161911968, 0.1237527818078103109, 0.1350030346994294250, 0.1462532875910485530, 0.1575035404826676810, 0.1687537933742867813, 0.1800040462659059093, 0.1912542991575250373, 0.2025045520491441375, 0.2137548049407632655, 0.2250050578323823935, 0.2362553107240014938, 0.2475055636156206218, 0.2587558165072397776, 0.2700060693988588501, 0.2812563222904779781, 0.2925065751820971061, 0.3037568280737162341, 0.3150070809653353621, 0.3262573338569544346, 0.3375075867485735626, 0.3487578396401927461, 0.3600080925318118186, 0.3712583454234309466, 0.3825085983150500746, 0.3937588512066691471, 0.4050091040982882751, 0.4162593569899074586, 0.4275096098815265311, 0.4387598627731456591, 0.4500101156647647871, 0.4612603685563838596, 0.4725106214480029876, 0.4837608743396221711, 0.4950111272312412436, 0.5062613801228603716, 0.5175116330144795551, 0.5287618859060986276, 0.5400121387977177001, 0.5512623916893367726, 0.5625126445809559561, 0.5737628974725751396, 0.5850131503641942121, 0.5962634032558133956, 0.6075136561474324681, 0.6187639090390515406, 0.6300141619306707241, 0.6412644148222897966, 0.6525146677139088691, 0.6637649206055280526, 0.6750151734971471251, 0.6862654263887661976, 0.6975156792803854922, 0.7087659321720045646, 0.7200161850636236371, 0.7312664379552428207, 0.7425166908468618931, 0.7537669437384809656, 0.7650171966301001492, 0.7762674495217192217, 0.7875177024133382941, 0.7987679553049574777, 0.8100182081965765502, 0.8212684610881956226, 0.8325187139798149172, 0.8437689668714339897, 0.8550192197630530622, 0.8662694726546722457, 0.8775197255462913182, 0.8887699784379103907, 0.9000202313295295742, 0.9112704842211486467, 0.9225207371127677192, 0.9337709900043869027, 0.9450212428960059752, 0.9562714957876251587, 0.9675217486792443422, 0.9787720015708634147, 0.9900222544624824872, 1.000000000000000000 ),
 .UNSPECIFIED. ) 
 CURVE ( )  GEOMETRIC_REPRESENTATION_ITEM ( )  RATIONAL_B_SPLINE_CURVE ( ( 1.000000000000000000, 0.9238795325112867385, 1.000000000000000000, 0.9238795325112867385, 1.000000000000000000, 0.9238795325112867385, 1.000000000000000000, 0.9238795325112867385, 1.000000000000000000, 0.9238795325112867385, 1.000000000000000000, 0.9238795325112867385, 1.000000000000000000, 0.9238795325112867385, 1.000000000000000000, 0.9238795325112867385, 1.000000000000000000, 0.9238795325112867385, 1.000000000000000000, 0.9238795325112867385, 1.000000000000000000, 0.9238795325112867385, 1.000000000000000000, 0.9238795325112867385, 1.000000000000000000, 0.9238795325112867385, 1.000000000000000000, 0.9238795325112867385, 1.000000000000000000, 0.9238795325112867385, 1.000000000000000000, 0.9238795325112867385, 1.000000000000000000, 0.9238795325112867385, 1.000000000000000000, 0.9238795325112867385, 1.000000000000000000, 0.9238795325112867385, 1.000000000000000000, 0.9238795325112867385, 1.000000000000000000, 0.9238795325112867385, 1.000000000000000000, 0.9238795325112867385, 1.000000000000000000, 0.9238795325112867385, 1.000000000000000000, 0.9238795325112867385, 1.000000000000000000, 0.9238795325112867385, 1.000000000000000000, 0.9238795325112867385, 1.000000000000000000, 0.9238795325112867385, 1.000000000000000000, 0.9238795325112867385, 1.000000000000000000, 0.9238795325112867385, 1.000000000000000000, 0.9238795325112867385, 1.000000000000000000, 0.9238795325112867385, 1.000000000000000000, 0.9238795325112867385, 1.000000000000000000, 0.9238795325112867385, 1.000000000000000000, 0.9238795325112867385, 1.000000000000000000, 0.9238795325112867385, 1.000000000000000000, 0.9238795325112867385, 1.000000000000000000, 0.9238795325112867385, 1.000000000000000000, 0.9238795325112867385, 1.000000000000000000, 0.9238795325112867385, 1.000000000000000000, 0.9238795325112867385, 1.000000000000000000, 0.9238795325112867385, 1.000000000000000000, 0.9238795325112867385, 1.000000000000000000, 0.9238795325112867385, 1.000000000000000000, 0.9238795325112867385, 1.000000000000000000, 0.9238795325112867385, 1.000000000000000000, 0.9238795325112867385, 1.000000000000000000, 0.9238795325112867385, 1.000000000000000000, 0.9238795325112867385, 1.000000000000000000, 0.9238795325112867385, 1.000000000000000000, 0.9238795325112867385, 1.000000000000000000, 0.9238795325112867385, 1.000000000000000000, 0.9238795325112867385, 1.000000000000000000, 0.9238795325112867385, 1.000000000000000000, 0.9238795325112867385, 1.000000000000000000, 0.9238795325112867385, 1.000000000000000000, 0.9238795325112867385, 1.000000000000000000, 0.9238795325112867385, 1.000000000000000000, 0.9238795325112867385, 1.000000000000000000, 0.9238795325112867385, 1.000000000000000000, 0.9238795325112867385, 1.000000000000000000, 0.9238795325112867385, 1.000000000000000000, 0.9238795325112867385, 1.000000000000000000, 0.9238795325112867385, 1.000000000000000000, 0.9238795325112867385, 1.000000000000000000, 0.9238795325112867385, 1.000000000000000000, 0.9238795325112867385, 1.000000000000000000, 0.9238795325112867385, 1.000000000000000000, 0.9238795325112867385, 1.000000000000000000, 0.9238795325112867385, 1.000000000000000000, 0.9238795325112867385, 1.000000000000000000, 0.9238795325112867385, 1.000000000000000000, 0.9238795325112867385, 1.000000000000000000, 0.9238795325112867385, 1.000000000000000000, 0.9238795325112867385, 1.000000000000000000, 0.9238795325112867385, 1.000000000000000000, 0.9238795325112867385, 1.000000000000000000, 0.9238795325112867385, 1.000000000000000000, 0.9238795325112867385, 1.000000000000000000, 0.9238795325112867385, 1.000000000000000000, 0.9238795325112867385, 1.000000000000000000, 0.9238795325112867385, 1.000000000000000000, 0.9238795325112867385, 1.000000000000000000, 0.9238795325112867385, 1.000000000000000000, 0.9238795325112867385, 1.000000000000000000, 0.9238795325112867385, 1.000000000000000000, 0.9238795325112867385, 1.000000000000000000, 0.9238795325112867385, 1.000000000000000000, 0.9238795325112867385, 1.000000000000000000, 0.9324894593822820044, 0.9847278705211290895 ) ) 
 REPRESENTATION_ITEM ( '' )  );
#4272 = CARTESIAN_POINT ( 'NONE',  ( -16.20999260610575377, -7.914000153054798758, 63.74181402343131708 ) ) ;
#4273 = CARTESIAN_POINT ( 'NONE',  ( -41.16232914953070576, -14.80920654474410725, 73.09411764705880898 ) ) ;
#4274 = ORIENTED_EDGE ( 'NONE', *, *, #38727, .T. ) ;
#4275 = FACE_OUTER_BOUND ( 'NONE', #16659, .T. ) ;
#4276 = CARTESIAN_POINT ( 'NONE',  ( -24.37529183752970141, -13.98356525902160463, 73.13773933009861139 ) ) ;
#4277 = ADVANCED_FACE ( 'NONE', ( #23719 ), #31570, .T. ) ;
#4278 = CARTESIAN_POINT ( 'NONE',  ( -17.42409385541299471, -14.80920654474435594, 52.02966884056656482 ) ) ;
#4279 = CARTESIAN_POINT ( 'NONE',  ( -10.41569439578338496, -15.57669382292980131, 61.05261153187079515 ) ) ;
#4280 = CIRCLE ( 'NONE', #40436, 1.250000000000007994 ) ;
#4281 = CARTESIAN_POINT ( 'NONE',  ( -12.21634942047498384, -14.14445252980938683, 52.02966884056656482 ) ) ;
#4282 = CARTESIAN_POINT ( 'NONE',  ( -20.04909385650551457, -8.104110260919579645, 48.81699501597546487 ) ) ;
#4283 = AXIS2_PLACEMENT_3D ( 'NONE', #19465, #26371, #12323 ) ;
#4284 = EDGE_LOOP ( 'NONE', ( #9682, #1703, #13145, #5546, #20447 ) ) ;
#4285 = EDGE_CURVE ( 'NONE', #1012, #34613, #38463, .T. ) ;
#4286 = DIRECTION ( 'NONE',  ( -3.071710424422018668E-17, 6.404604876783312462E-16, 1.000000000000000000 ) ) ;
#4287 = CARTESIAN_POINT ( 'NONE',  ( -11.00824494338232284, -11.02245153356902030, 60.87874549475150587 ) ) ;
#4288 = ORIENTED_EDGE ( 'NONE', *, *, #17444, .T. ) ;
#4289 = DIRECTION ( 'NONE',  ( 0.9687793358424817702, -0.2479245821708686570, 0.000000000000000000 ) ) ;
#4290 = CARTESIAN_POINT ( 'NONE',  ( -15.30848412986786578, -21.53807271814892843, 65.31416673886597835 ) ) ;
#4291 = CARTESIAN_POINT ( 'NONE',  ( -18.46801905451614090, -7.836623195388690455, 74.12592262855558545 ) ) ;
#4292 = EDGE_LOOP ( 'NONE', ( #14622, #26408, #44641, #1898, #23574 ) ) ;
#4293 = DIRECTION ( 'NONE',  ( 0.8705373987491421550, -0.4921022631314296292, 4.758021987246392057E-08 ) ) ;
#4294 =( BOUNDED_CURVE ( )  B_SPLINE_CURVE ( 3, ( #31601, #27412, #38233, #11923 ),
 .UNSPECIFIED., .F., .F. ) 
 B_SPLINE_CURVE_WITH_KNOTS ( ( 4, 4 ),
 ( 0.9074455897393672865, 1.000000000000000000 ),
 .UNSPECIFIED. ) 
 CURVE ( )  GEOMETRIC_REPRESENTATION_ITEM ( )  RATIONAL_B_SPLINE_CURVE ( ( 0.6983129098260997258, 0.7760317562607039754, 0.8765941196520040668, 1.000000000000000000 ) ) 
 REPRESENTATION_ITEM ( '' )  );
#4295 = EDGE_CURVE ( 'NONE', #43099, #7039, #47188, .T. ) ;
#4296 = DIRECTION ( 'NONE',  ( -8.339041841313433703E-07, -7.401745998521586792E-06, 0.9999999999722594124 ) ) ;
#4297 = EDGE_LOOP ( 'NONE', ( #26550, #23859, #20775, #40130, #44836 ) ) ;
#4298 = CARTESIAN_POINT ( 'NONE',  ( -15.32409385650551670, -6.426201560718813433, 50.50509628382439331 ) ) ;
#4299 = EDGE_CURVE ( 'NONE', #6587, #15782, #32803, .T. ) ;
#4300 = CARTESIAN_POINT ( 'NONE',  ( -33.52409385541305653, -8.109206544744111511, 50.49999999999998579 ) ) ;
#4301 = CARTESIAN_POINT ( 'NONE',  ( -24.79583619959666763, -15.88736519870960784, 69.67274155994940088 ) ) ;
#4302 = CARTESIAN_POINT ( 'NONE',  ( -10.52991759648590531, -16.02177972226642311, 68.27767831073917648 ) ) ;
#4303 = B_SPLINE_CURVE_WITH_KNOTS ( 'NONE', 3,
 ( #24637, #38669, #16966, #16493, #32010, #47024, #31527, #20196, #35208, #31769 ),
 .UNSPECIFIED., .F., .F.,
 ( 4, 2, 2, 2, 4 ),
 ( 0.000000000000000000, 0.2500000000000000000, 0.5000000000000000000, 0.7500000000000000000, 1.000000000000000000 ),
 .UNSPECIFIED. ) ;
#4304 = DIRECTION ( 'NONE',  ( -0.2189141945955536406, 0.9757441136919965397, 0.000000000000000000 ) ) ;
#4305 = ORIENTED_EDGE ( 'NONE', *, *, #44467, .F. ) ;
#4306 = EDGE_LOOP ( 'NONE', ( #26160, #28478, #28027, #38915, #13793 ) ) ;
#4307 = CARTESIAN_POINT ( 'NONE',  ( -16.31159385650551386, -6.922745924619793101, 51.69366785382590024 ) ) ;
#4308 = CARTESIAN_POINT ( 'NONE',  ( -22.98865756656685022, -9.855479763439479512, 70.12683098403445570 ) ) ;
#4309 = CARTESIAN_POINT ( 'NONE',  ( -17.42409385541299471, -14.80920654474435771, 49.52966884056655772 ) ) ;
#4310 = CARTESIAN_POINT ( 'NONE',  ( 18.57590614458706924, 1.878297441959757785, 52.28023643296099010 ) ) ;
#4312 = EDGE_CURVE ( 'NONE', #2748, #38065, #32301, .T. ) ;
#4311 = CARTESIAN_POINT ( 'NONE',  ( -16.93034385650552309, -9.794322478646142471, 51.19202720610083901 ) ) ;
#4313 = EDGE_CURVE ( 'NONE', #26935, #35691, #7257, .T. ) ;
#4314 = VECTOR ( 'NONE', #4658, 1000.000000000000000 ) ;
#4315 = CARTESIAN_POINT ( 'NONE',  ( -23.00441852451001523, -19.11762575345012749, 58.88410642058938294 ) ) ;
#4316 = EDGE_CURVE ( 'NONE', #44852, #37303, #41665, .T. ) ;
#4317 = CARTESIAN_POINT ( 'NONE',  ( -20.94465692579565896, -8.243430592510261334, 59.95629952546280350 ) ) ;
#4318 = CARTESIAN_POINT ( 'NONE',  ( -18.86948588052436904, -7.959932294928454333, 66.90071733017600764 ) ) ;
#4319 = FACE_OUTER_BOUND ( 'NONE', #43939, .T. ) ;
#4320 = ORIENTED_EDGE ( 'NONE', *, *, #37251, .T. ) ;
#4321 = CARTESIAN_POINT ( 'NONE',  ( -24.72409385541305582, -14.90920654474421170, 67.05882352941175384 ) ) ;
#4322 = ORIENTED_EDGE ( 'NONE', *, *, #48349, .F. ) ;
#4323 = CARTESIAN_POINT ( 'NONE',  ( -22.33142775017075010, -9.202805011845722305, 59.90826508960974195 ) ) ;
#4324 = CARTESIAN_POINT ( 'NONE',  ( -20.21484531253453198, -8.389572098386633314, 66.97207325640498254 ) ) ;
#4325 = CYLINDRICAL_SURFACE ( 'NONE', #37014, 4.686499999999997002 ) ;
#4326 = PLANE ( 'NONE',  #35612 ) ;
#4327 = ORIENTED_EDGE ( 'NONE', *, *, #4641, .T. ) ;
#4328 = CARTESIAN_POINT ( 'NONE',  ( -20.21944967009625671, -8.333140613769380423, 73.81276534411087198 ) ) ;
#4329 = CARTESIAN_POINT ( 'NONE',  ( -21.36489355414517988, -8.963473290115421932, 73.90128753234840531 ) ) ;
#4330 = CARTESIAN_POINT ( 'NONE',  ( -24.72409385541305582, -14.90920654474424190, 70.07647058823528141 ) ) ;
#4331 = FACE_OUTER_BOUND ( 'NONE', #30439, .T. ) ;
#4332 = ORIENTED_EDGE ( 'NONE', *, *, #29601, .F. ) ;
#4333 = CYLINDRICAL_SURFACE ( 'NONE', #17356, 0.1500000000000015488 ) ;
#4334 = CARTESIAN_POINT ( 'NONE',  ( -24.22092332596094977, -12.93687947476191269, 66.45246741375130739 ) ) ;
#4335 = PLANE ( 'NONE',  #23098 ) ;
#4336 = PLANE ( 'NONE',  #10065 ) ;
#4337 = APPLICATION_PROTOCOL_DEFINITION ( 'draft international standard', 'automotive_design', 1998, #10515 ) ;
#4338 = ORIENTED_EDGE ( 'NONE', *, *, #44462, .T. ) ;
#4339 = CARTESIAN_POINT ( 'NONE',  ( -11.38873422713818684, -18.35549357326604891, 58.10714557467345998 ) ) ;
#4340 = CARTESIAN_POINT ( 'NONE',  ( -15.20214831426356739, -21.92027429138432026, 68.69780165605466493 ) ) ;
#4341 = CARTESIAN_POINT ( 'NONE',  ( -21.67609690912980014, -8.690862426448951794, 73.78784151156415305 ) ) ;
#4342 = ORIENTED_EDGE ( 'NONE', *, *, #21348, .T. ) ;
#4343 = LINE ( 'NONE', #44746, #22909 ) ;
#4344 = ORIENTED_EDGE ( 'NONE', *, *, #32984, .T. ) ;
#4345 = CARTESIAN_POINT ( 'NONE',  ( -12.73481051501216044, -9.020086340885832499, 70.95651207417664352 ) ) ;
#4346 = CARTESIAN_POINT ( 'NONE',  ( -13.21199854220980718, -9.217750189091946211, 67.39559466746432292 ) ) ;
#4347 = VERTEX_POINT ( 'NONE', #36674 ) ;
#4348 = CARTESIAN_POINT ( 'NONE',  ( -9.939267784769082681, -14.33236412611010913, 53.49999999999994316 ) ) ;
#4349 = EDGE_CURVE ( 'NONE', #36615, #14276, #199, .T. ) ;
#4350 = EDGE_LOOP ( 'NONE', ( #31517, #13786 ) ) ;
#4351 = ORIENTED_EDGE ( 'NONE', *, *, #26350, .F. ) ;
#4352 = ORIENTED_EDGE ( 'NONE', *, *, #1107, .T. ) ;
#4353 = CARTESIAN_POINT ( 'NONE',  ( -22.28902083190231309, -19.84295425696266335, 69.19034576393465841 ) ) ;
#4354 = CARTESIAN_POINT ( 'NONE',  ( -19.38292004262868673, -21.99720527105973744, 58.64694598308297202 ) ) ;
#4355 = CARTESIAN_POINT ( 'NONE',  ( -16.42409385759798823, -9.359200813967568422, 50.49621490985803263 ) ) ;
#4356 = CARTESIAN_POINT ( 'NONE',  ( -12.65491851050466288, -19.93331706820960747, 68.63657436096360698 ) ) ;
#4357 = CYLINDRICAL_SURFACE ( 'NONE', #14961, 0.1500000000000038802 ) ;
#4358 = VERTEX_POINT ( 'NONE', #17500 ) ;
#4359 = ORIENTED_EDGE ( 'NONE', *, *, #43943, .F. ) ;
#4360 = CARTESIAN_POINT ( 'NONE',  ( -46.47622156840087371, -14.20920654474410760, 70.87000000000000455 ) ) ;
#4361 = CARTESIAN_POINT ( 'NONE',  ( -10.38752013045322009, -14.36951432065623635, 64.67331771650336236 ) ) ;
#4362 = CYLINDRICAL_SURFACE ( 'NONE', #14996, 0.3999999999999975797 ) ;
#4363 = ORIENTED_EDGE ( 'NONE', *, *, #26234, .T. ) ;
#4364 = CARTESIAN_POINT ( 'NONE',  ( -16.50534385650551883, -8.801233750844183135, 48.81488406609782515 ) ) ;
#4365 = EDGE_CURVE ( 'NONE', #34898, #40354, #8997, .T. ) ;
#4366 = ORIENTED_EDGE ( 'NONE', *, *, #8954, .F. ) ;
#4367 = ADVANCED_FACE ( 'NONE', ( #31811 ), #40399, .T. ) ;
#4368 = EDGE_CURVE ( 'NONE', #28537, #34367, #35325, .T. ) ;
#4369 = CARTESIAN_POINT ( 'NONE',  ( -12.41310947992116098, -19.76871611099698001, 61.68206578716802113 ) ) ;
#4370 = B_SPLINE_CURVE_WITH_KNOTS ( 'NONE', 1,
 ( #27746, #42776 ),
 .UNSPECIFIED., .F., .F.,
 ( 2, 2 ),
 ( 0.000000000000000000, 1.000000000000000000 ),
 .UNSPECIFIED. ) ;
#4371 = CARTESIAN_POINT ( 'NONE',  ( -15.22349782163815490, -21.45476955923737705, 68.85976349797824980 ) ) ;
#4372 = ORIENTED_EDGE ( 'NONE', *, *, #6608, .T. ) ;
#4373 = CARTESIAN_POINT ( 'NONE',  ( -10.00117625416208433, -15.44487358686203571, 57.68297391752145842 ) ) ;
#4374 = AXIS2_PLACEMENT_3D ( 'NONE', #7215, #65, #29860 ) ;
#4375 = CARTESIAN_POINT ( 'NONE',  ( -10.42581515057458930, -14.65397996935263336, 67.96686193206075188 ) ) ;
#4376 = CARTESIAN_POINT ( 'NONE',  ( -16.15640231613377154, -10.29741749701175202, 52.02966884056656482 ) ) ;
#4377 = ORIENTED_EDGE ( 'NONE', *, *, #21519, .T. ) ;
#4378 = CARTESIAN_POINT ( 'NONE',  ( -10.56492483649129710, -13.18000429128331596, 71.50828586225091499 ) ) ;
#4379 = FACE_OUTER_BOUND ( 'NONE', #37075, .T. ) ;
#4380 = CARTESIAN_POINT ( 'NONE',  ( -20.18232088801011415, -7.888550879367295821, 73.82822426864265708 ) ) ;
#4381 = EDGE_LOOP ( 'NONE', ( #1761, #28551, #42276, #23994 ) ) ;
#4382 = CARTESIAN_POINT ( 'NONE',  ( -10.49862800246030936, -15.82799116930659622, 64.50771590054291948 ) ) ;
#4383 = ORIENTED_EDGE ( 'NONE', *, *, #30565, .T. ) ;
#4384 = CARTESIAN_POINT ( 'NONE',  ( -10.61247293337548214, -12.97981955831074075, 71.62317441356958625 ) ) ;
#4385 = CARTESIAN_POINT ( 'NONE',  ( -11.03124136535102373, -17.66077402989073875, 71.56718193465405875 ) ) ;
#4386 = ORIENTED_EDGE ( 'NONE', *, *, #31017, .T. ) ;
#4387 = CARTESIAN_POINT ( 'NONE',  ( -23.96075626263749214, -17.45014286185010732, 66.24357239682277054 ) ) ;
#4389 = EDGE_CURVE ( 'NONE', #32914, #15992, #39732, .T. ) ;
#4388 = CARTESIAN_POINT ( 'NONE',  ( -17.94572468556024702, -21.83992273462958877, 62.17535918563021369 ) ) ;
#4390 = CARTESIAN_POINT ( 'NONE',  ( -14.28913879486226435, -8.050816564744696535, 67.37479651646088996 ) ) ;
#4391 = ORIENTED_EDGE ( 'NONE', *, *, #33343, .F. ) ;
#4392 = CARTESIAN_POINT ( 'NONE',  ( -21.31800817620502286, -20.62620158190326336, 72.82446429882371319 ) ) ;
#4393 = DIRECTION ( 'NONE',  ( 0.000000000000000000, 1.000000000000000000, -0.000000000000000000 ) ) ;
#4394 = CARTESIAN_POINT ( 'NONE',  ( -11.48063109083140354, -11.11096805901812878, 57.50903159540615661 ) ) ;
#4395 = ORIENTED_EDGE ( 'NONE', *, *, #7324, .T. ) ;
#4396 = CARTESIAN_POINT ( 'NONE',  ( -12.36756753426621813, -9.896138138887707214, 57.37463480816234096 ) ) ;
#4397 = CARTESIAN_POINT ( 'NONE',  ( -23.34288396506439867, -19.33377296368179543, 59.06906041190286771 ) ) ;
#4398 = ORIENTED_EDGE ( 'NONE', *, *, #1526, .T. ) ;
#4399 = VERTEX_POINT ( 'NONE', #5950 ) ;
#4400 = CARTESIAN_POINT ( 'NONE',  ( -22.84587727614884756, -10.37951393556890523, 66.77012138597072521 ) ) ;
#4401 = CARTESIAN_POINT ( 'NONE',  ( -10.61247293337548214, -12.97981955831074075, 71.62317441356958625 ) ) ;
#4402 = DIRECTION ( 'NONE',  ( 1.000000000000000000, -4.164305804376849172E-17, 1.614929280266638808E-16 ) ) ;
#4403 = CARTESIAN_POINT ( 'NONE',  ( -20.83659385650551599, -6.915538690918074494, 49.31353937987644542 ) ) ;
#4404 = CARTESIAN_POINT ( 'NONE',  ( -24.46950595589296285, -14.38832865607273703, 73.26704460715303924 ) ) ;
#4405 =( BOUNDED_CURVE ( )  B_SPLINE_CURVE ( 3, ( #46823, #20490, #46350, #16527 ),
 .UNSPECIFIED., .F., .F. ) 
 B_SPLINE_CURVE_WITH_KNOTS ( ( 4, 4 ),
 ( 0.9074455897393649551, 1.000000000000000000 ),
 .UNSPECIFIED. ) 
 CURVE ( )  GEOMETRIC_REPRESENTATION_ITEM ( )  RATIONAL_B_SPLINE_CURVE ( ( 0.6983129098260905110, 0.7760317562606959818, 0.8765941196519991818, 1.000000000000000000 ) ) 
 REPRESENTATION_ITEM ( '' )  );
#4406 = CARTESIAN_POINT ( 'NONE',  ( -12.40538917401127961, -20.31523793222865493, 68.52152763170285255 ) ) ;
#4407 = CARTESIAN_POINT ( 'NONE',  ( -14.51159385759799214, -8.990409506049202193, 49.61344411288074951 ) ) ;
#4408 = CARTESIAN_POINT ( 'NONE',  ( -11.07238894598444112, -11.74315414212633080, 67.50375847841529264 ) ) ;
#4409 = AXIS2_PLACEMENT_3D ( 'NONE', #10539, #6602, #14670 ) ;
#4410 = ORIENTED_EDGE ( 'NONE', *, *, #33600, .T. ) ;
#4411 = DIRECTION ( 'NONE',  ( -0.1648596854219665231, -0.9863170302304251624, 7.074492695208254125E-08 ) ) ;
#4412 =( NAMED_UNIT ( * ) SI_UNIT ( $, .STERADIAN. ) SOLID_ANGLE_UNIT ( ) );
#4413 = CARTESIAN_POINT ( 'NONE',  ( -24.53360078033622216, -12.58211837844622849, 69.93276349028228367 ) ) ;
#4414 = CARTESIAN_POINT ( 'NONE',  ( -23.89370412103122021, -17.61049410758369760, 62.77360985931112225 ) ) ;
#4415 =( BOUNDED_CURVE ( )  B_SPLINE_CURVE ( 3, ( #5809, #43234, #9508, #12700 ),
 .UNSPECIFIED., .F., .F. ) 
 B_SPLINE_CURVE_WITH_KNOTS ( ( 4, 4 ),
 ( 0.5000000000000000000, 0.9074455897393668424 ),
 .UNSPECIFIED. ) 
 CURVE ( )  GEOMETRIC_REPRESENTATION_ITEM ( )  RATIONAL_B_SPLINE_CURVE ( ( 1.000000000000026423, 0.4567392136813426817, 0.3561768502900156674, 0.6983129098260740797 ) ) 
 REPRESENTATION_ITEM ( '' )  );
#4416 = ORIENTED_EDGE ( 'NONE', *, *, #25102, .F. ) ;
#4417 = ORIENTED_EDGE ( 'NONE', *, *, #26961, .T. ) ;
#4418 = EDGE_CURVE ( 'NONE', #5705, #18740, #37350, .T. ) ;
#4419 = CARTESIAN_POINT ( 'NONE',  ( -19.92732520184441825, -21.34631850905071815, 69.05907916208967379 ) ) ;
#4420 = CARTESIAN_POINT ( 'NONE',  ( -23.85974590284097374, -11.05473623917629844, 73.54848671873985211 ) ) ;
#4421 = CARTESIAN_POINT ( 'NONE',  ( -15.40747091633432575, -21.98125088338273514, 72.18428936984274458 ) ) ;
#4422 = CARTESIAN_POINT ( 'NONE',  ( -15.93879930885702656, -7.917138641544857691, 67.15479422225767792 ) ) ;
#4423 = ORIENTED_EDGE ( 'NONE', *, *, #28900, .T. ) ;
#4424 = CARTESIAN_POINT ( 'NONE',  ( -20.19231683483797113, -8.325423577284544407, 70.55100341277886855 ) ) ;
#4425 =( BOUNDED_SURFACE ( )  B_SPLINE_SURFACE ( 3, 1, ( 
 ( #3750, #15967 ),
 ( #14316, #29609 ),
 ( #29367, #44638 ),
 ( #44399, #31010 ),
 ( #8359, #18765 ),
 ( #14792, #38372 ),
 ( #4666, #46031 ) ),
 .UNSPECIFIED., .T., .F., .F. ) 
 B_SPLINE_SURFACE_WITH_KNOTS ( ( 4, 3, 4 ),
 ( 2, 2 ),
 ( 0.000000000000000000, 0.5000000000000000000, 1.000000000000000000 ),
 ( 0.000000000000000000, 1.000000000000000000 ),
 .UNSPECIFIED. ) 
 GEOMETRIC_REPRESENTATION_ITEM ( )  RATIONAL_B_SPLINE_SURFACE ( (
 ( 1.000000000000000000, 1.000000000000000000),
 ( 0.3333333333333335369, 0.3333333333333330373),
 ( 0.3333333333333335369, 0.3333333333333330373),
 ( 1.000000000000000000, 1.000000000000000000),
 ( 0.3333333333333333703, 0.3333333333333333703),
 ( 0.3333333333333333703, 0.3333333333333333703),
 ( 1.000000000000000000, 1.000000000000000000) ) ) 
 REPRESENTATION_ITEM ( '' )  SURFACE ( )  );
#4426 = ADVANCED_FACE ( 'NONE', ( #29077 ), #11759, .T. ) ;
#4427 = EDGE_CURVE ( 'NONE', #21415, #46626, #33226, .T. ) ;
#4428 = CARTESIAN_POINT ( 'NONE',  ( -24.47217469005601131, -14.64471752244405067, 62.71296487297676947 ) ) ;
#4429 = ORIENTED_EDGE ( 'NONE', *, *, #14551, .F. ) ;
#4430 = EDGE_CURVE ( 'NONE', #28690, #25694, #17986, .T. ) ;
#4431 = CARTESIAN_POINT ( 'NONE',  ( -24.46146587544552276, -14.38248120490118609, 66.46820668217904426 ) ) ;
#4432 = EDGE_CURVE ( 'NONE', #27722, #16942, #46702, .T. ) ;
#4433 = CARTESIAN_POINT ( 'NONE',  ( -50.42609385541305755, -14.80920654474423159, 69.07058823529411029 ) ) ;
#4434 = VERTEX_POINT ( 'NONE', #14501 ) ;
#4435 = CARTESIAN_POINT ( 'NONE',  ( -12.46122051107220408, -19.81685944811288991, 64.88146935704573082 ) ) ;
#4436 = AXIS2_PLACEMENT_3D ( 'NONE', #16822, #21682, #36665 ) ;
#4437 = AXIS2_PLACEMENT_3D ( 'NONE', #41356, #22656, #28036 ) ;
#4438 = ORIENTED_EDGE ( 'NONE', *, *, #25544, .F. ) ;
#4439 = CARTESIAN_POINT ( 'NONE',  ( -10.81170448216924740, -12.36318809540519048, 57.34329390664808557 ) ) ;
#4440 = CARTESIAN_POINT ( 'NONE',  ( -11.42587710518540334, -11.10406226247761019, 57.49431069621225276 ) ) ;
#4441 = EDGE_LOOP ( 'NONE', ( #14485, #43355, #48668, #359, #4634 ) ) ;
#4442 = DIRECTION ( 'NONE',  ( 2.866981220435666553E-17, -1.000000000000000000, -1.190614954331866791E-16 ) ) ;
#4443 = PLANE ( 'NONE',  #30508 ) ;
#4444 = EDGE_CURVE ( 'NONE', #29219, #3179, #22183, .T. ) ;
#4445 = CARTESIAN_POINT ( 'NONE',  ( -18.95534385650551457, -7.417179338643134834, 52.18511593390279302 ) ) ;
#4446 = CARTESIAN_POINT ( 'NONE',  ( -17.57433509196185994, -21.80920136703782575, 58.51626380509593162 ) ) ;
#4447 = CARTESIAN_POINT ( 'NONE',  ( -10.54860170345752302, -17.67816087046063700, 68.28996115284763846 ) ) ;
#4448 = CYLINDRICAL_SURFACE ( 'NONE', #12479, 2.000000000000001776 ) ;
#4449 = EDGE_LOOP ( 'NONE', ( #31051, #29171, #21182, #15665 ) ) ;
#4450 = CARTESIAN_POINT ( 'NONE',  ( -19.22579631480732587, -21.57336711704104104, 58.82507384991394872 ) ) ;
#4451 = CARTESIAN_POINT ( 'NONE',  ( -16.61784385541296416, -6.860780111192013919, 51.02154966934431002 ) ) ;
#4452 = CARTESIAN_POINT ( 'NONE',  ( -23.56856754720352853, -18.27334893135431315, 72.76367955138505295 ) ) ;
#4453 = CARTESIAN_POINT ( 'NONE',  ( -20.49775566701509177, -11.27142682889164327, 52.02966884056656482 ) ) ;
#4454 = CYLINDRICAL_SURFACE ( 'NONE', #12114, 5.249999999999998224 ) ;
#4455 = ORIENTED_EDGE ( 'NONE', *, *, #14484, .T. ) ;
#4456 = ORIENTED_EDGE ( 'NONE', *, *, #45821, .F. ) ;
#4457 = CARTESIAN_POINT ( 'NONE',  ( -18.69922557824643761, -7.468382084482742655, 74.02719791125277027 ) ) ;
#4458 = DIRECTION ( 'NONE',  ( 2.866981220435666553E-17, -1.000000000000000000, -1.190614954331866791E-16 ) ) ;
#4459 = ORIENTED_EDGE ( 'NONE', *, *, #44297, .F. ) ;
#4460 = CARTESIAN_POINT ( 'NONE',  ( -24.00225419842380603, -17.20718624873268254, 73.07263044545001662 ) ) ;
#4461 = DIRECTION ( 'NONE',  ( -1.352396026799963059E-06, -5.694414568552746141E-07, -0.9999999999989234167 ) ) ;
#4462 = CARTESIAN_POINT ( 'NONE',  ( -21.09284385759799463, -8.630756214087126565, 51.74842643355248129 ) ) ;
#4463 = CARTESIAN_POINT ( 'NONE',  ( -20.63647318826268773, -18.96169002115701119, 49.52966884056656482 ) ) ;
#4464 = CARTESIAN_POINT ( 'NONE',  ( -14.24059955017480306, -8.515543114936868108, 67.14486463900426827 ) ) ;
#4465 = CARTESIAN_POINT ( 'NONE',  ( -19.55458118857802319, -21.94809134954223140, 62.09480011547082512 ) ) ;
#4466 = FACE_OUTER_BOUND ( 'NONE', #27960, .T. ) ;
#4467 = ORIENTED_EDGE ( 'NONE', *, *, #16075, .T. ) ;
#4468 = CARTESIAN_POINT ( 'NONE',  ( -24.38957690932039313, -15.50410419900979342, 73.01806150963400910 ) ) ;
#4469 = DIRECTION ( 'NONE',  ( 1.000000000000000000, -4.164305804376849788E-17, 1.614929280266638808E-16 ) ) ;
#4470 = CARTESIAN_POINT ( 'NONE',  ( -15.50784526261009511, -8.076599967007890513, 74.37985659287807039 ) ) ;
#4471 = CARTESIAN_POINT ( 'NONE',  ( -14.84764829735760827, -8.246537290690364230, 60.33468334944129197 ) ) ;
#4472 = CARTESIAN_POINT ( 'NONE',  ( -14.07539642552819359, -8.605278304397881328, 74.19954655214911554 ) ) ;
#4473 = EDGE_CURVE ( 'NONE', #8895, #36030, #40082, .T. ) ;
#4474 = B_SPLINE_CURVE_WITH_KNOTS ( 'NONE', 3,
 ( #1023, #4239, #3997, #38431, #33763, #783, #15044, #15780, #30104, #16019 ),
 .UNSPECIFIED., .F., .F.,
 ( 4, 2, 2, 2, 4 ),
 ( 0.000000000000000000, 0.2500000000000000000, 0.5000000000000000000, 0.7500000000000000000, 1.000000000000000000 ),
 .UNSPECIFIED. ) ;
#4475 = DIRECTION ( 'NONE',  ( -0.9687793358424821033, 0.2479245821708677133, 0.000000000000000000 ) ) ;
#4476 = VERTEX_POINT ( 'NONE', #15252 ) ;
#4477 = CIRCLE ( 'NONE', #31997, 1.249999999999999556 ) ;
#4478 = ORIENTED_EDGE ( 'NONE', *, *, #29302, .F. ) ;
#4479 = AXIS2_PLACEMENT_3D ( 'NONE', #47855, #24964, #6256 ) ;
#4480 = CARTESIAN_POINT ( 'NONE',  ( -22.63659385650551670, -6.915538690918074494, 49.31353937987644542 ) ) ;
#4481 = EDGE_LOOP ( 'NONE', ( #41779, #2990, #21238, #11186, #8309, #41469, #17486, #17323, #14298, #13479, #11383, #24725, #26743 ) ) ;
#4482 = EDGE_CURVE ( 'NONE', #7468, #45657, #3263, .T. ) ;
#4483 = CARTESIAN_POINT ( 'NONE',  ( -11.25622321624083355, -18.98904307544693282, 64.86051675911045322 ) ) ;
#4484 = CARTESIAN_POINT ( 'NONE',  ( -33.52409385541305653, -8.109206544744111511, 49.44999999999998863 ) ) ;
#4485 = AXIS2_PLACEMENT_3D ( 'NONE', #27264, #8557, #32417 ) ;
#4486 = CARTESIAN_POINT ( 'NONE',  ( -21.84256997353123353, -8.809979007422205299, 66.77494628644626573 ) ) ;
#4487 = CARTESIAN_POINT ( 'NONE',  ( -13.27409385759798965, -6.859212275519751323, 50.50378509014259265 ) ) ;
#4488 = CARTESIAN_POINT ( 'NONE',  ( -17.72612443559818018, -7.765381109175947927, 60.36588690973874094 ) ) ;
#4489 = ORIENTED_EDGE ( 'NONE', *, *, #18256, .T. ) ;
#4490 = ADVANCED_FACE ( 'NONE', ( #29558 ), #31606, .T. ) ;
#4491 = DIRECTION ( 'NONE',  ( 0.9687793358424821033, -0.2479245821708679909, 0.000000000000000000 ) ) ;
#4492 = CARTESIAN_POINT ( 'NONE',  ( -18.53202070066404517, -7.846807721809618386, 73.84064401782792686 ) ) ;
#4493 = EDGE_CURVE ( 'NONE', #14, #21561, #37165, .T. ) ;
#4494 = EDGE_LOOP ( 'NONE', ( #28604, #33133 ) ) ;
#4495 = CARTESIAN_POINT ( 'NONE',  ( -11.32266926000110985, -11.37785695497957228, 64.44882076993899034 ) ) ;
#4496 = CARTESIAN_POINT ( 'NONE',  ( -12.23758870452319236, -20.15736674837955889, 64.96651269001253581 ) ) ;
#4497 = ORIENTED_EDGE ( 'NONE', *, *, #6866, .F. ) ;
#4498 = EDGE_CURVE ( 'NONE', #15877, #30899, #41625, .T. ) ;
#4499 = CARTESIAN_POINT ( 'NONE',  ( -24.87417961795293664, -14.80849281899037884, 59.42795564617806292 ) ) ;
#4500 = CARTESIAN_POINT ( 'NONE',  ( -26.92409385541305511, -6.859206544744110623, 63.99999999999998579 ) ) ;
#4501 = CARTESIAN_POINT ( 'NONE',  ( -20.43749099114212342, -18.39845715627588874, 49.52966884056656482 ) ) ;
#4502 = ORIENTED_EDGE ( 'NONE', *, *, #7749, .T. ) ;
#4503 = CARTESIAN_POINT ( 'NONE',  ( -14.54176566789882585, -21.67913831930545854, 58.28122448549703449 ) ) ;
#4504 = EDGE_CURVE ( 'NONE', #42067, #44829, #21517, .T. ) ;
#4505 = CARTESIAN_POINT ( 'NONE',  ( -16.11718879935913407, -7.932176570520619308, 63.97011080779262215 ) ) ;
#4506 = DIRECTION ( 'NONE',  ( -3.071710424422018668E-17, 6.404604876783312462E-16, 1.000000000000000000 ) ) ;
#4507 = LINE ( 'NONE', #47570, #14025 ) ;
#4508 = CARTESIAN_POINT ( 'NONE',  ( -20.00946503018472811, -8.250368534377352958, 73.72096600125087207 ) ) ;
#4509 = TOROIDAL_SURFACE ( 'NONE', #21031, 2.260000000000000675, 0.2399999999999998246 ) ;
#4510 = CIRCLE ( 'NONE', #43861, 2.000000000000001776 ) ;
#4511 = CARTESIAN_POINT ( 'NONE',  ( -23.36251582567715701, -10.31057965045351388, 59.75203426425787256 ) ) ;
#4512 = FACE_OUTER_BOUND ( 'NONE', #4381, .T. ) ;
#4513 = CARTESIAN_POINT ( 'NONE',  ( -22.63560595208270954, -20.13310736574185000, 69.28922662766110818 ) ) ;
#4514 = CARTESIAN_POINT ( 'NONE',  ( -21.17409385650551812, -9.792211528768504536, 50.49490371617623197 ) ) ;
#4515 = ORIENTED_EDGE ( 'NONE', *, *, #19938, .F. ) ;
#4516 = CYLINDRICAL_SURFACE ( 'NONE', #10192, 5.249999999999998224 ) ;
#4517 = CYLINDRICAL_SURFACE ( 'NONE', #39958, 0.1499999999999955536 ) ;
#4518 = ORIENTED_EDGE ( 'NONE', *, *, #16829, .T. ) ;
#4519 = CARTESIAN_POINT ( 'NONE',  ( -10.37394849890712401, -14.76283852923608464, 71.61310637325181006 ) ) ;
#4520 = AXIS2_PLACEMENT_3D ( 'NONE', #48634, #11453, #37794 ) ;
#4521 = FACE_OUTER_BOUND ( 'NONE', #9662, .T. ) ;
#4522 = CARTESIAN_POINT ( 'NONE',  ( -20.75354924259569245, -21.52967727414722532, 54.27966884056655061 ) ) ;
#4523 = VERTEX_POINT ( 'NONE', #19944 ) ;
#4524 = CARTESIAN_POINT ( 'NONE',  ( -10.04821616988549593, -15.85811384580076933, 64.62276300976363075 ) ) ;
#4525 = CARTESIAN_POINT ( 'NONE',  ( -19.05924993160927983, -8.002740344303022724, 63.73089191517998842 ) ) ;
#4526 = EDGE_LOOP ( 'NONE', ( #10187, #32784, #38881, #37367, #48200 ) ) ;
#4527 = CARTESIAN_POINT ( 'NONE',  ( -12.81603496567665879, -20.14954717766431003, 68.54477457630689230 ) ) ;
#4528 = CARTESIAN_POINT ( 'NONE',  ( -12.85370899154983526, -8.925770522350823910, 67.48604460341357481 ) ) ;
#4529 = EDGE_CURVE ( 'NONE', #1590, #24111, #11576, .T. ) ;
#4530 = DIRECTION ( 'NONE',  ( 0.9345716196833626643, -0.3557750520798446114, -2.412542649833449708E-09 ) ) ;
#4531 = CARTESIAN_POINT ( 'NONE',  ( -23.16108440525936274, -18.82016358243141241, 62.42694848944771024 ) ) ;
#4532 = ORIENTED_EDGE ( 'NONE', *, *, #31788, .F. ) ;
#4533 = ORIENTED_EDGE ( 'NONE', *, *, #30160, .F. ) ;
#4534 = CARTESIAN_POINT ( 'NONE',  ( -21.96159385541304232, -7.228003583438117552, 51.38655588711986155 ) ) ;
#4535 = DIRECTION ( 'NONE',  ( -3.071710424422018668E-17, 6.404604876783312462E-16, 1.000000000000000000 ) ) ;
#4536 = APPLICATION_CONTEXT ( 'automotive_design' ) ;
#4537 = CIRCLE ( 'NONE', #31289, 2.000000000000002220 ) ;
#4538 = CARTESIAN_POINT ( 'NONE',  ( -24.15236833420705764, -12.70328255177875754, 70.06683202284229139 ) ) ;
#4539 =( BOUNDED_CURVE ( )  B_SPLINE_CURVE ( 3, ( #8903, #24404, #13532, #17232 ),
 .UNSPECIFIED., .F., .F. ) 
 B_SPLINE_CURVE_WITH_KNOTS ( ( 4, 4 ),
 ( 0.5000000000000000000, 0.9074455897393604031 ),
 .UNSPECIFIED. ) 
 CURVE ( )  GEOMETRIC_REPRESENTATION_ITEM ( )  RATIONAL_B_SPLINE_CURVE ( ( 0.9999999999999921174, 0.4567392136813352987, 0.3561768502900369282, 0.6983129098260885126 ) ) 
 REPRESENTATION_ITEM ( '' )  );
#4540 = VECTOR ( 'NONE', #1439, 1000.000000000000114 ) ;
#4541 = VECTOR ( 'NONE', #21937, 1000.000000000000000 ) ;
#4542 = CARTESIAN_POINT ( 'NONE',  ( -17.77761167241057549, -22.25089262147902147, 58.44907471483963946 ) ) ;
#4543 = CARTESIAN_POINT ( 'NONE',  ( -20.38775243360237965, -8.467418945486670623, 67.08104087472003130 ) ) ;
#4544 = ADVANCED_FACE ( 'NONE', ( #15984 ), #27086, .T. ) ;
#4545 = CARTESIAN_POINT ( 'NONE',  ( -10.37795889460693033, -14.56696403379599403, 68.14328054657653411 ) ) ;
#4546 = CIRCLE ( 'NONE', #32084, 2.000000000000001332 ) ;
#4547 = CARTESIAN_POINT ( 'NONE',  ( -24.36611147337434957, -16.04009697885371111, 66.07797069094537790 ) ) ;
#4548 = EDGE_CURVE ( 'NONE', #37558, #24279, #45137, .T. ) ;
#4549 = ORIENTED_EDGE ( 'NONE', *, *, #24624, .F. ) ;
#4550 =( BOUNDED_SURFACE ( )  B_SPLINE_SURFACE ( 3, 1, ( 
 ( #1798, #28395 ),
 ( #16797, #13818 ),
 ( #46858, #43419 ),
 ( #13099, #9685 ),
 ( #28859, #24701 ),
 ( #39706, #2277 ),
 ( #13581, #43903 ) ),
 .UNSPECIFIED., .T., .F., .F. ) 
 B_SPLINE_SURFACE_WITH_KNOTS ( ( 4, 3, 4 ),
 ( 2, 2 ),
 ( 0.000000000000000000, 0.5000000000000000000, 1.000000000000000000 ),
 ( 0.000000000000000000, 1.000000000000000000 ),
 .UNSPECIFIED. ) 
 GEOMETRIC_REPRESENTATION_ITEM ( )  RATIONAL_B_SPLINE_SURFACE ( (
 ( 1.000000000000000000, 1.000000000000000000),
 ( 0.3333333333333335369, 0.3333333333333330373),
 ( 0.3333333333333335369, 0.3333333333333330373),
 ( 1.000000000000000000, 1.000000000000000000),
 ( 0.3333333333333333703, 0.3333333333333333703),
 ( 0.3333333333333333703, 0.3333333333333333703),
 ( 1.000000000000000000, 1.000000000000000000) ) ) 
 REPRESENTATION_ITEM ( '' )  SURFACE ( )  );
#4551 = CARTESIAN_POINT ( 'NONE',  ( -21.28537167527045071, -20.64804852447636918, 72.52446480616642077 ) ) ;
#4552 = CIRCLE ( 'NONE', #26567, 1.250000000000007994 ) ;
#4553 = CARTESIAN_POINT ( 'NONE',  ( -24.30112618867181240, -13.25578303422174997, 59.64795780745660636 ) ) ;
#4554 = VERTEX_POINT ( 'NONE', #34716 ) ;
#4555 = ADVANCED_FACE ( 'NONE', ( #30555 ), #12788, .T. ) ;
#4556 = CARTESIAN_POINT ( 'NONE',  ( -13.02884944951828494, -13.18282747993466941, 49.52966884056655772 ) ) ;
#4557 = FACE_OUTER_BOUND ( 'NONE', #43608, .T. ) ;
#4558 = CARTESIAN_POINT ( 'NONE',  ( -10.93232766038821424, -17.55941949638709687, 68.38249893951126523 ) ) ;
#4559 = FACE_OUTER_BOUND ( 'NONE', #10018, .T. ) ;
#4560 = ORIENTED_EDGE ( 'NONE', *, *, #374, .T. ) ;
#4561 = CARTESIAN_POINT ( 'NONE',  ( -10.37462440636232053, -14.89569459299594456, 75.09778901493891112 ) ) ;
#4562 = EDGE_CURVE ( 'NONE', #45761, #10902, #15648, .T. ) ;
#4563 = CARTESIAN_POINT ( 'NONE',  ( -21.57657733182563931, -11.59682721189464871, 50.77966884056655772 ) ) ;
#4564 = CARTESIAN_POINT ( 'NONE',  ( -20.87530219893326588, -8.206670134541473871, 59.96312479527349382 ) ) ;
#4565 = ORIENTED_EDGE ( 'NONE', *, *, #34020, .T. ) ;
#4566 = CARTESIAN_POINT ( 'NONE',  ( -10.33762933896429637, -17.10842426733604782, 57.86477433150147931 ) ) ;
#4567 = CYLINDRICAL_SURFACE ( 'NONE', #28957, 4.686499999999997002 ) ;
#4569 =( BOUNDED_SURFACE ( )  B_SPLINE_SURFACE ( 3, 1, ( 
 ( #42352, #9351 ),
 ( #12068, #12785 ),
 ( #5411, #42107 ),
 ( #16709, #4676 ),
 ( #1213, #38390 ),
 ( #35186, #31750 ),
 ( #8370, #15980 ) ),
 .UNSPECIFIED., .T., .F., .F. ) 
 B_SPLINE_SURFACE_WITH_KNOTS ( ( 4, 3, 4 ),
 ( 2, 2 ),
 ( 0.000000000000000000, 0.5000000000000000000, 1.000000000000000000 ),
 ( 0.000000000000000000, 1.000000000000000000 ),
 .UNSPECIFIED. ) 
 GEOMETRIC_REPRESENTATION_ITEM ( )  RATIONAL_B_SPLINE_SURFACE ( (
 ( 1.000000000000000000, 1.000000000000000000),
 ( 0.3333333333333335369, 0.3333333333333330373),
 ( 0.3333333333333335369, 0.3333333333333330373),
 ( 1.000000000000000000, 1.000000000000000000),
 ( 0.3333333333333333703, 0.3333333333333333703),
 ( 0.3333333333333333703, 0.3333333333333333703),
 ( 1.000000000000000000, 1.000000000000000000) ) ) 
 REPRESENTATION_ITEM ( '' )  SURFACE ( )  );
#4568 = CARTESIAN_POINT ( 'NONE',  ( -23.55661029900229053, -18.29303667177271464, 72.64879359478229048 ) ) ;
#4570 = CARTESIAN_POINT ( 'NONE',  ( -21.18000274887674905, -20.77541536365158592, 69.05450184741354747 ) ) ;
#4571 = APPLICATION_PROTOCOL_DEFINITION ( 'draft international standard', 'automotive_design', 1998, #43887 ) ;
#4572 = DIRECTION ( 'NONE',  ( -0.8651630202045380580, 0.5014907262059380422, 5.433021001366389699E-08 ) ) ;
#4573 = CYLINDRICAL_SURFACE ( 'NONE', #41282, 0.1500000000000043243 ) ;
#4574 = CARTESIAN_POINT ( 'NONE',  ( -14.66790711817407278, -21.29843871104708342, 58.18089935161520287 ) ) ;
#4575 = VERTEX_POINT ( 'NONE', #38893 ) ;
#4576 = CARTESIAN_POINT ( 'NONE',  ( -19.77436091090941517, -21.87886160397694368, 65.64981624214608757 ) ) ;
#4577 = ORIENTED_EDGE ( 'NONE', *, *, #29192, .F. ) ;
#4578 = VECTOR ( 'NONE', #39651, 1000.000000000000114 ) ;
#4579 = CARTESIAN_POINT ( 'NONE',  ( -21.47456293661849713, -9.038556783377254433, 70.41660404402310292 ) ) ;
#4580 = CARTESIAN_POINT ( 'NONE',  ( -16.79100947509958175, -22.23238548518695268, 68.87277532904636246 ) ) ;
#4581 = EDGE_CURVE ( 'NONE', #47078, #1710, #15082, .T. ) ;
#4582 = EDGE_LOOP ( 'NONE', ( #39174, #33852, #6507, #13289, #22448 ) ) ;
#4583 = DIRECTION ( 'NONE',  ( -1.000000000000000000, 0.000000000000000000, 0.000000000000000000 ) ) ;
#4584 = AXIS2_PLACEMENT_3D ( 'NONE', #24922, #46848, #2741 ) ;
#4585 = AXIS2_PLACEMENT_3D ( 'NONE', #22619, #7861, #11534 ) ;
#4586 = ADVANCED_FACE ( 'NONE', ( #5171 ), #26561, .T. ) ;
#4587 = FACE_BOUND ( 'NONE', #6456, .T. ) ;
#4588 = ORIENTED_EDGE ( 'NONE', *, *, #22141, .F. ) ;
#4589 = ORIENTED_EDGE ( 'NONE', *, *, #47198, .F. ) ;
#4590 = VERTEX_POINT ( 'NONE', #30798 ) ;
#4591 = FACE_OUTER_BOUND ( 'NONE', #26406, .T. ) ;
#4592 = B_SPLINE_CURVE_WITH_KNOTS ( 'NONE', 3,
 ( #38436, #22463, #4727, #19749, #15052, #45132, #11377, #26399, #41411, #4470 ),
 .UNSPECIFIED., .F., .F.,
 ( 4, 2, 2, 2, 4 ),
 ( 0.000000000000000000, 0.2499999999999981126, 0.4999999999999962252, 0.7499999999999943379, 1.000000000000000000 ),
 .UNSPECIFIED. ) ;
#4593 = CIRCLE ( 'NONE', #10879, 0.5000000000000004441 ) ;
#4594 = FACE_OUTER_BOUND ( 'NONE', #3915, .T. ) ;
#4595 = DIRECTION ( 'NONE',  ( -0.1240347345892086200, 1.145860353393066553E-16, -0.9922778767136676281 ) ) ;
#4596 = CARTESIAN_POINT ( 'NONE',  ( -10.37352921641884684, -17.21638894027030986, 61.31889622878785673 ) ) ;
#4597 = CARTESIAN_POINT ( 'NONE',  ( -20.17268378225416825, -8.371407738384645469, 70.25100341248858626 ) ) ;
#4598 = CARTESIAN_POINT ( 'NONE',  ( -19.32724692393761146, -8.072771991737997865, 59.96093028617590903 ) ) ;
#4599 = ORIENTED_EDGE ( 'NONE', *, *, #3440, .T. ) ;
#4600 = ORIENTED_EDGE ( 'NONE', *, *, #33947, .T. ) ;
#4601 = B_SPLINE_CURVE_WITH_KNOTS ( 'NONE', 1,
 ( #5586, #38817 ),
 .UNSPECIFIED., .F., .F.,
 ( 2, 2 ),
 ( 0.000000000000000000, 1.000000000000000000 ),
 .UNSPECIFIED. ) ;
#4602 = CARTESIAN_POINT ( 'NONE',  ( -22.78034385650551741, -6.424090610841176385, 49.80797279389977916 ) ) ;
#4603 = CARTESIAN_POINT ( 'NONE',  ( -22.54688186880658307, -20.21864567242280941, 65.84275238437966493 ) ) ;
#4604 = LINE ( 'NONE', #19624, #27610 ) ;
#4605 = CARTESIAN_POINT ( 'NONE',  ( -20.75486715718922781, -8.591426074064321128, 63.61121613145932940 ) ) ;
#4606 = ORIENTED_EDGE ( 'NONE', *, *, #16234, .T. ) ;
#4607 = CARTESIAN_POINT ( 'NONE',  ( -15.94284385650552238, -8.811426318492348031, 52.18089403414752070 ) ) ;
#4608 = ORIENTED_EDGE ( 'NONE', *, *, #13516, .T. ) ;
#4609 = CARTESIAN_POINT ( 'NONE',  ( -23.04367355717579713, -10.55211556811382856, 59.90203429191419815 ) ) ;
#4610 = CARTESIAN_POINT ( 'NONE',  ( -12.51133688094842888, -19.86980477907010822, 61.28190024782882972 ) ) ;
#4611 = VECTOR ( 'NONE', #6391, 1000.000000000000000 ) ;
#4612 = CARTESIAN_POINT ( 'NONE',  ( -24.46281123712706673, -17.25067832759902942, 73.06148774291726511 ) ) ;
#4613 = CIRCLE ( 'NONE', #43966, 0.5560000000000009379 ) ;
#4614 = ORIENTED_EDGE ( 'NONE', *, *, #22545, .F. ) ;
#4615 = CARTESIAN_POINT ( 'NONE',  ( -10.43972881942000086, -15.77115500203794873, 64.52243715390834211 ) ) ;
#4616 = AXIS2_PLACEMENT_3D ( 'NONE', #19764, #35001, #31317 ) ;
#4617 = ADVANCED_FACE ( 'NONE', ( #45816 ), #16220, .T. ) ;
#4618 = CARTESIAN_POINT ( 'NONE',  ( -11.33385179977767265, -19.10019906511433518, 68.26043675633501095 ) ) ;
#4619 = DIRECTION ( 'NONE',  ( -3.071710424422018668E-17, 6.404604876783312462E-16, 1.000000000000000000 ) ) ;
#4620 = EDGE_CURVE ( 'NONE', #46199, #23813, #46804, .T. ) ;
#4621 = ORIENTED_EDGE ( 'NONE', *, *, #48585, .T. ) ;
#4622 = AXIS2_PLACEMENT_3D ( 'NONE', #37545, #18855, #21815 ) ;
#4623 = CARTESIAN_POINT ( 'NONE',  ( -24.64621740481133116, -16.83181165628401033, 47.99999999999994316 ) ) ;
#4624 = CARTESIAN_POINT ( 'NONE',  ( -22.87317391125343846, -19.20579927338366133, 58.99483778520830413 ) ) ;
#4625 = CARTESIAN_POINT ( 'NONE',  ( -17.42409385541299471, -14.80920654474435771, 49.52966884056655772 ) ) ;
#4626 = ORIENTED_EDGE ( 'NONE', *, *, #43652, .T. ) ;
#4627 = CARTESIAN_POINT ( 'NONE',  ( -22.04378365035703879, -20.13510231884741231, 62.24911246861644543 ) ) ;
#4628 = ORIENTED_EDGE ( 'NONE', *, *, #24534, .T. ) ;
#4629 = CARTESIAN_POINT ( 'NONE',  ( -18.50196246566170899, -7.838335838159340874, 70.37067732408392828 ) ) ;
#4630 = CARTESIAN_POINT ( 'NONE',  ( -22.00995465109835436, -9.454493699438653920, 59.72171220707129891 ) ) ;
#4631 = ORIENTED_EDGE ( 'NONE', *, *, #34946, .F. ) ;
#4632 = CARTESIAN_POINT ( 'NONE',  ( -22.22619444978876757, -20.50513558618911958, 58.94938304221643222 ) ) ;
#4633 = CARTESIAN_POINT ( 'NONE',  ( -24.47324232082262085, -14.69046401860230766, 62.71856245267908747 ) ) ;
#4634 = ORIENTED_EDGE ( 'NONE', *, *, #29266, .F. ) ;
#4635 = CARTESIAN_POINT ( 'NONE',  ( -10.66331429883175019, -17.94058386735023802, 71.68062945273115361 ) ) ;
#4636 = CARTESIAN_POINT ( 'NONE',  ( -27.42409385541305511, -6.359206544744109735, 63.99999999999998579 ) ) ;
#4638 = EDGE_CURVE ( 'NONE', #43983, #28258, #1687, .T. ) ;
#4637 = CARTESIAN_POINT ( 'NONE',  ( -11.95118918738345748, -9.754277919233853567, 60.69771603915999947 ) ) ;
#4639 = VERTEX_POINT ( 'NONE', #24374 ) ;
#4640 = CARTESIAN_POINT ( 'NONE',  ( -12.15286730501820678, -9.544433317881530598, 57.34581436681493471 ) ) ;
#4641 = EDGE_CURVE ( 'NONE', #29512, #45877, #46190, .T. ) ;
#4642 = B_SPLINE_CURVE_WITH_KNOTS ( 'NONE', 3,
 ( #48215, #220, #14445, #33663, #26300, #44788, #11040, #7852, #29504, #37115 ),
 .UNSPECIFIED., .F., .F.,
 ( 4, 2, 2, 2, 4 ),
 ( 0.6272669072877827823, 0.7522669073072977275, 0.8772669073268126727, 1.002266907346327507, 1.127266907365842563 ),
 .UNSPECIFIED. ) ;
#4643 = CARTESIAN_POINT ( 'NONE',  ( -21.73099075187129614, -8.730192115828774746, 70.31627817507801126 ) ) ;
#4644 = EDGE_CURVE ( 'NONE', #43113, #26442, #6848, .T. ) ;
#4645 = EDGE_CURVE ( 'NONE', #46252, #9124, #35615, .T. ) ;
#4646 = EDGE_CURVE ( 'NONE', #6597, #31450, #22740, .T. ) ;
#4647 = EDGE_LOOP ( 'NONE', ( #16547, #20714, #20087, #44 ) ) ;
#4648 = ORIENTED_EDGE ( 'NONE', *, *, #39017, .T. ) ;
#4649 = LINE ( 'NONE', #476, #24386 ) ;
#4650 = CARTESIAN_POINT ( 'NONE',  ( -19.23659385759798823, -8.995762431863214559, 51.38120296130585274 ) ) ;
#4651 = B_SPLINE_CURVE_WITH_KNOTS ( 'NONE', 3,
 ( #2847, #25505, #22060, #37058, #17854, #47919, #18345, #48390, #14626, #15372 ),
 .UNSPECIFIED., .F., .F.,
 ( 4, 2, 2, 2, 4 ),
 ( 0.6272669072877907759, 0.7522669073073098289, 0.8772669073268288820, 1.002266907346347935, 1.127266907365866988 ),
 .UNSPECIFIED. ) ;
#4653 = CARTESIAN_POINT ( 'NONE',  ( -11.49287318421094817, -18.63485491799402993, 57.96281551145487043 ) ) ;
#4652 = CIRCLE ( 'NONE', #32171, 1.249999999999999556 ) ;
#4654 =( BOUNDED_CURVE ( )  B_SPLINE_CURVE ( 3, ( #36923, #18705, #33712, #6905 ),
 .UNSPECIFIED., .F., .F. ) 
 B_SPLINE_CURVE_WITH_KNOTS ( ( 4, 4 ),
 ( 0.9074455897393653991, 1.000000000000000000 ),
 .UNSPECIFIED. ) 
 CURVE ( )  GEOMETRIC_REPRESENTATION_ITEM ( )  RATIONAL_B_SPLINE_CURVE ( ( 0.6983129098261023904, 0.7760317562607063069, 0.8765941196520055101, 1.000000000000000000 ) ) 
 REPRESENTATION_ITEM ( '' )  );
#4655 = CARTESIAN_POINT ( 'NONE',  ( -22.63659385650551670, -6.915538690918074494, 49.31353937987644542 ) ) ;
#4656 =( GEOMETRIC_REPRESENTATION_CONTEXT ( 3 ) GLOBAL_UNCERTAINTY_ASSIGNED_CONTEXT ( ( #23354 ) ) GLOBAL_UNIT_ASSIGNED_CONTEXT ( ( #21908, #18442, #17714 ) ) REPRESENTATION_CONTEXT ( 'NONE', 'WORKASPACE' ) );
#4657 = CARTESIAN_POINT ( 'NONE',  ( -12.09966231065201825, -10.17612992894743229, 71.11326093460978370 ) ) ;
#4658 = DIRECTION ( 'NONE',  ( -3.071710424422018668E-17, 6.404604876783312462E-16, 1.000000000000000000 ) ) ;
#4659 = AXIS2_PLACEMENT_3D ( 'NONE', #24925, #6214, #21235 ) ;
#4660 = AXIS2_PLACEMENT_3D ( 'NONE', #26259, #24868, #37562 ) ;
#4661 = DIRECTION ( 'NONE',  ( 0.9687793358424819923, -0.2479245821708678243, 0.000000000000000000 ) ) ;
#4662 = EDGE_LOOP ( 'NONE', ( #47175, #30766 ) ) ;
#4663 = ORIENTED_EDGE ( 'NONE', *, *, #17376, .T. ) ;
#4664 = DIRECTION ( 'NONE',  ( 2.081668171172170091E-15, -0.000000000000000000, -1.000000000000000000 ) ) ;
#4665 = B_SPLINE_CURVE_WITH_KNOTS ( 'NONE', 1,
 ( #17271, #32317 ),
 .UNSPECIFIED., .F., .F.,
 ( 2, 2 ),
 ( 0.000000000000000000, 1.000000000000000000 ),
 .UNSPECIFIED. ) ;
#4666 = CARTESIAN_POINT ( 'NONE',  ( -14.78766009005058812, -21.34800739930362568, 58.45145834864037937 ) ) ;
#4667 = CARTESIAN_POINT ( 'NONE',  ( -10.03904597514415009, -13.82694077737217242, 57.56329639008353638 ) ) ;
#4668 = ORIENTED_EDGE ( 'NONE', *, *, #26947, .F. ) ;
#4669 = VERTEX_POINT ( 'NONE', #47264 ) ;
#4670 = EDGE_CURVE ( 'NONE', #29749, #38378, #42094, .T. ) ;
#4671 = FACE_OUTER_BOUND ( 'NONE', #364, .T. ) ;
#4672 = LINE ( 'NONE', #42602, #38628 ) ;
#4673 = CARTESIAN_POINT ( 'NONE',  ( -15.52404113052931223, -21.54652912111637164, 72.04575433027748943 ) ) ;
#4674 = VERTEX_POINT ( 'NONE', #40519 ) ;
#4675 = CARTESIAN_POINT ( 'NONE',  ( -24.43574572327428740, -14.04659777256190623, 69.53786587444344036 ) ) ;
#4676 = CARTESIAN_POINT ( 'NONE',  ( -24.79781851656146330, -15.87314393256401424, 69.64812203948034153 ) ) ;
#4677 = ORIENTED_EDGE ( 'NONE', *, *, #40052, .T. ) ;
#4678 = ADVANCED_FACE ( 'NONE', ( #6796 ), #18336, .T. ) ;
#4679 = VECTOR ( 'NONE', #20307, 999.9999999999998863 ) ;
#4680 = B_SPLINE_CURVE_WITH_KNOTS ( 'NONE', 3,
 ( #44821, #18683, #25107, #3937, #11073, #33691, #26096, #22904, #483, #26579 ),
 .UNSPECIFIED., .F., .F.,
 ( 4, 2, 2, 2, 4 ),
 ( 0.6272669072878297447, 0.7522669073073277035, 0.8772669073268255513, 1.002266907346323510, 1.127266907365821469 ),
 .UNSPECIFIED. ) ;
#4681 = CARTESIAN_POINT ( 'NONE',  ( -11.10386160987148862, -10.86480171160796893, 57.25257256893876701 ) ) ;
#4682 = CARTESIAN_POINT ( 'NONE',  ( -14.13242279744181751, -8.574497162196566435, 74.21426705364891063 ) ) ;
#4683 = EDGE_LOOP ( 'NONE', ( #6582, #30249 ) ) ;
#4684 = CARTESIAN_POINT ( 'NONE',  ( -20.38226146016681994, -7.971588334861294811, 70.36604906519886526 ) ) ;
#4685 = AXIS2_PLACEMENT_3D ( 'NONE', #33503, #36706, #36480 ) ;
#4686 = VECTOR ( 'NONE', #45794, 1000.000000000000000 ) ;
#4687 = VERTEX_POINT ( 'NONE', #26004 ) ;
#4688 = CARTESIAN_POINT ( 'NONE',  ( -17.42409385541299471, -14.80920654474435771, 49.52966884056655772 ) ) ;
#4689 = CARTESIAN_POINT ( 'NONE',  ( -20.39277704316526751, -8.469891104483282973, 63.42007541787698699 ) ) ;
#4690 = ORIENTED_EDGE ( 'NONE', *, *, #34712, .F. ) ;
#4691 = CARTESIAN_POINT ( 'NONE',  ( -13.33151401730585306, -20.55006798877650454, 58.06122216312902395 ) ) ;
#4692 = CARTESIAN_POINT ( 'NONE',  ( -24.36611147337434957, -16.04009697885371111, 66.07797069094537790 ) ) ;
#4693 = CARTESIAN_POINT ( 'NONE',  ( -16.87409385650551386, -9.792211528768504536, 50.49490371617623197 ) ) ;
#4694 = PLANE ( 'NONE',  #3194 ) ;
#4695 = CIRCLE ( 'NONE', #3900, 2.000000000000000000 ) ;
#4696 =( BOUNDED_SURFACE ( )  B_SPLINE_SURFACE ( 3, 1, ( 
 ( #9335, #36376 ),
 ( #43557, #34757 ),
 ( #1698, #24604 ),
 ( #9818, #42156 ),
 ( #16698, #28032 ),
 ( #2170, #31737 ),
 ( #5649, #20657 ) ),
 .UNSPECIFIED., .T., .F., .F. ) 
 B_SPLINE_SURFACE_WITH_KNOTS ( ( 4, 3, 4 ),
 ( 2, 2 ),
 ( 0.000000000000000000, 0.5000000000000000000, 1.000000000000000000 ),
 ( 0.000000000000000000, 1.000000000000000000 ),
 .UNSPECIFIED. ) 
 GEOMETRIC_REPRESENTATION_ITEM ( )  RATIONAL_B_SPLINE_SURFACE ( (
 ( 1.000000000000000000, 1.000000000000000000),
 ( 0.3333333333333335369, 0.3333333333333330373),
 ( 0.3333333333333335369, 0.3333333333333330373),
 ( 1.000000000000000000, 1.000000000000000000),
 ( 0.3333333333333333703, 0.3333333333333333703),
 ( 0.3333333333333333703, 0.3333333333333333703),
 ( 1.000000000000000000, 1.000000000000000000) ) ) 
 REPRESENTATION_ITEM ( '' )  SURFACE ( )  );
#4697 = DIRECTION ( 'NONE',  ( -3.071710424422018668E-17, 6.404604876783312462E-16, 1.000000000000000000 ) ) ;
#4698 = CARTESIAN_POINT ( 'NONE',  ( -17.04413539470110095, -21.84925844046378174, 72.45071136019464575 ) ) ;
#4699 = VERTEX_POINT ( 'NONE', #4561 ) ;
#4700 = CARTESIAN_POINT ( 'NONE',  ( -19.08084801036773825, -21.61197561877568063, 58.63580559908311329 ) ) ;
#4701 = CARTESIAN_POINT ( 'NONE',  ( -13.43773910423563400, -20.62433115109003268, 58.33177939114180788 ) ) ;
#4702 = CYLINDRICAL_SURFACE ( 'NONE', #27367, 0.1500000000000020206 ) ;
#4703 = CARTESIAN_POINT ( 'NONE',  ( -18.34838239305179641, -21.74803989268259130, 69.11514668064288003 ) ) ;
#4704 = CARTESIAN_POINT ( 'NONE',  ( -20.74847848266319161, -20.96993682883388743, 62.39854858292977724 ) ) ;
#4705 = ADVANCED_FACE ( 'NONE', ( #19096 ), #15625, .F. ) ;
#4706 = ADVANCED_FACE ( 'NONE', ( #41501 ), #6718, .T. ) ;
#4708 = ORIENTED_EDGE ( 'NONE', *, *, #6512, .F. ) ;
#4707 = VECTOR ( 'NONE', #28793, 1000.000000000000000 ) ;
#4709 = ORIENTED_EDGE ( 'NONE', *, *, #29594, .T. ) ;
#4710 = CARTESIAN_POINT ( 'NONE',  ( -18.56115164150112662, -7.446410555819776178, 73.88418448558978469 ) ) ;
#4711 = LINE ( 'NONE', #527, #12425 ) ;
#4712 = ORIENTED_EDGE ( 'NONE', *, *, #38371, .T. ) ;
#4713 = CARTESIAN_POINT ( 'NONE',  ( -9.994877497295997060, -15.37525289974553289, 57.75448116320448833 ) ) ;
#4714 = DIRECTION ( 'NONE',  ( 0.3824554607245534421, -0.9239739285077093189, 8.917814433895553251E-09 ) ) ;
#4715 = FACE_OUTER_BOUND ( 'NONE', #37569, .T. ) ;
#4716 = DIRECTION ( 'NONE',  ( -0.1648596854219664953, -0.9863170302304249404, 7.074492695208252801E-08 ) ) ;
#4717 = CARTESIAN_POINT ( 'NONE',  ( -11.16720114480626336, -11.56054632707691709, 67.61864607954859707 ) ) ;
#4718 = CARTESIAN_POINT ( 'NONE',  ( -12.31380156693488992, -10.02538874655004442, 60.85918086676540639 ) ) ;
#4719 =( BOUNDED_CURVE ( )  B_SPLINE_CURVE ( 3, ( #47351, #25173, #40190, #6463 ),
 .UNSPECIFIED., .F., .F. ) 
 B_SPLINE_CURVE_WITH_KNOTS ( ( 4, 4 ),
 ( 0.9074455897393634007, 1.000000000000000000 ),
 .UNSPECIFIED. ) 
 CURVE ( )  GEOMETRIC_REPRESENTATION_ITEM ( )  RATIONAL_B_SPLINE_CURVE ( ( 0.6983129098260865142, 0.7760317562606925401, 0.8765941196519970724, 1.000000000000000000 ) ) 
 REPRESENTATION_ITEM ( '' )  );
#4720 = CARTESIAN_POINT ( 'NONE',  ( -24.14679772577363437, -12.68507108172156705, 70.05770892828130059 ) ) ;
#4721 = VERTEX_POINT ( 'NONE', #7301 ) ;
#4722 = EDGE_CURVE ( 'NONE', #25942, #43778, #33427, .T. ) ;
#4723 = ADVANCED_FACE ( 'NONE', ( #26484 ), #48561, .T. ) ;
#4724 = FACE_OUTER_BOUND ( 'NONE', #48658, .T. ) ;
#4725 = FACE_OUTER_BOUND ( 'NONE', #23559, .T. ) ;
#4726 = AXIS2_PLACEMENT_3D ( 'NONE', #45386, #41688, #7724 ) ;
#4727 = CARTESIAN_POINT ( 'NONE',  ( -15.58315477633296631, -8.055165212349223225, 74.09602325307160697 ) ) ;
#4728 = CARTESIAN_POINT ( 'NONE',  ( -13.84034573514469457, -20.82276458638829553, 68.74008628059695525 ) ) ;
#4729 = CARTESIAN_POINT ( 'NONE',  ( -21.38764993922222146, -9.039365983805389249, 70.20420499562830230 ) ) ;
#4730 = CARTESIAN_POINT ( 'NONE',  ( -15.92487197799934506, -7.971525956357276677, 67.14007330039670762 ) ) ;
#4731 = ORIENTED_EDGE ( 'NONE', *, *, #5334, .F. ) ;
#4732 = EDGE_LOOP ( 'NONE', ( #42030, #33199, #2012, #12171 ) ) ;
#4733 = CARTESIAN_POINT ( 'NONE',  ( -21.96159385650551599, -9.295667164867525756, 49.30633214617472504 ) ) ;
#4734 = ORIENTED_EDGE ( 'NONE', *, *, #3692, .F. ) ;
#4735 = EDGE_CURVE ( 'NONE', #70, #34400, #3843, .T. ) ;
#4736 = CARTESIAN_POINT ( 'NONE',  ( -12.01493067177793606, -9.686186367714711309, 60.68201168315654570 ) ) ;
#4737 = LINE ( 'NONE', #46343, #21365 ) ;
#4738 = AXIS2_PLACEMENT_3D ( 'NONE', #7386, #22386, #18676 ) ;
#4739 = VERTEX_POINT ( 'NONE', #34590 ) ;
#4740 = DIRECTION ( 'NONE',  ( 0.000000000000000000, 0.000000000000000000, 1.000000000000000000 ) ) ;
#4741 = CARTESIAN_POINT ( 'NONE',  ( -13.44284385759799605, -7.587656875400192291, 49.25157356644813689 ) ) ;
#4742 = CARTESIAN_POINT ( 'NONE',  ( -17.58536440216138885, -7.758048768718602162, 59.96572088198239214 ) ) ;
#4743 = VERTEX_POINT ( 'NONE', #26973 ) ;
#4744 = CARTESIAN_POINT ( 'NONE',  ( -16.00570185478497010, -7.495462356776134705, 63.77036791188361775 ) ) ;
#4745 = CARTESIAN_POINT ( 'NONE',  ( -10.48085305489969521, -13.91959585118948617, 57.74825035244229809 ) ) ;
#4746 = ORIENTED_EDGE ( 'NONE', *, *, #24002, .F. ) ;
#4747 = CARTESIAN_POINT ( 'NONE',  ( 9.825906144586951996, -0.1092432217106413528, 50.52422457691088908 ) ) ;
#4748 = CARTESIAN_POINT ( 'NONE',  ( -12.25981284559622075, -20.17899088736047730, 65.04391808465086910 ) ) ;
#4749 = ORIENTED_EDGE ( 'NONE', *, *, #17341, .T. ) ;
#4750 = DIRECTION ( 'NONE',  ( 1.000000000000000000, -0.000000000000000000, 2.081668171172170091E-15 ) ) ;
#4751 = CARTESIAN_POINT ( 'NONE',  ( -22.53098214739562621, -20.23350217257768691, 65.89695895308028639 ) ) ;
#4752 = CARTESIAN_POINT ( 'NONE',  ( -24.03350017844798003, -12.50343444556183847, 73.25728008851183404 ) ) ;
#4753 = ORIENTED_EDGE ( 'NONE', *, *, #8939, .F. ) ;
#4754 = CARTESIAN_POINT ( 'NONE',  ( -10.93447185890128992, -11.14999657484283446, 64.28848697573772597 ) ) ;
#4755 = CARTESIAN_POINT ( 'NONE',  ( -17.80091866675434886, -21.79911790395781424, 58.69088063202684680 ) ) ;
#4756 = AXIS2_PLACEMENT_3D ( 'NONE', #22611, #44790, #25812 ) ;
#4757 = AXIS2_PLACEMENT_3D ( 'NONE', #3712, #41631, #36679 ) ;
#4758 = DIRECTION ( 'NONE',  ( 8.136802275736123818E-17, -2.353473986169886338E-17, 1.000000000000000000 ) ) ;
#4759 = CARTESIAN_POINT ( 'NONE',  ( -21.30572535954460633, -21.16897061578360351, 65.69798576082847319 ) ) ;
#4760 = LINE ( 'NONE', #8705, #37634 ) ;
#4761 = VECTOR ( 'NONE', #16697, 1000.000000000000000 ) ;
#4762 = CARTESIAN_POINT ( 'NONE',  ( -14.78766009005058635, -21.34800739930362568, 58.45145834864037937 ) ) ;
#4763 = PLANE ( 'NONE',  #16337 ) ;
#4764 = CARTESIAN_POINT ( 'NONE',  ( -23.92719435707370224, -11.17417392741853988, 70.00715344888816105 ) ) ;
#4765 = CARTESIAN_POINT ( 'NONE',  ( -10.47679690896004701, -15.67958946752583138, 64.61844751979357682 ) ) ;
#4766 = CARTESIAN_POINT ( 'NONE',  ( -16.39284385650552167, -7.406986770994972602, 48.81910596585309747 ) ) ;
#4767 = ADVANCED_FACE ( 'NONE', ( #876 ), #18852, .F. ) ;
#4768 = ORIENTED_EDGE ( 'NONE', *, *, #10574, .F. ) ;
#4769 = CARTESIAN_POINT ( 'NONE',  ( -14.05371270701021302, -21.00138147690670820, 71.92607703580544865 ) ) ;
#4770 = CARTESIAN_POINT ( 'NONE',  ( -10.45662601068241848, -17.44683468735947685, 64.72765127533203611 ) ) ;
#4771 = VERTEX_POINT ( 'NONE', #39511 ) ;
#4772 = CARTESIAN_POINT ( 'NONE',  ( -15.62222905942471840, -7.993050613273783966, 70.89517703929612935 ) ) ;
#4773 = AXIS2_PLACEMENT_3D ( 'NONE', #1135, #38812, #24774 ) ;
#4774 = CARTESIAN_POINT ( 'NONE',  ( -21.59671027634132656, -20.98115415594247324, 72.56800473755950520 ) ) ;
#4775 = CARTESIAN_POINT ( 'NONE',  ( -22.78195790197552384, -10.22153446486525219, 63.28005797477638339 ) ) ;
#4776 = CARTESIAN_POINT ( 'NONE',  ( -22.72031779163844334, -16.29245029320677673, 53.49899999999994549 ) ) ;
#4777 = ORIENTED_EDGE ( 'NONE', *, *, #15308, .F. ) ;
#4778 = FACE_OUTER_BOUND ( 'NONE', #47645, .T. ) ;
#4779 = EDGE_CURVE ( 'NONE', #27411, #23020, #20373, .T. ) ;
#4780 = CARTESIAN_POINT ( 'NONE',  ( -24.02655296236175175, -11.35792967378293916, 66.53719098615387395 ) ) ;
#4781 = ORIENTED_EDGE ( 'NONE', *, *, #38218, .F. ) ;
#4782 = DIRECTION ( 'NONE',  ( 0.05202058437830281434, -0.9986460127597465153, 1.657953767687799911E-08 ) ) ;
#4783 = EDGE_CURVE ( 'NONE', #29219, #1317, #16762, .T. ) ;
#4784 = EDGE_CURVE ( 'NONE', #29774, #45804, #17765, .T. ) ;
#4785 = LINE ( 'NONE', #366, #21668 ) ;
#4786 = CARTESIAN_POINT ( 'NONE',  ( -10.02134419679888211, -13.96483583313674615, 61.10476640098193002 ) ) ;
#4787 = CARTESIAN_POINT ( 'NONE',  ( -21.71931446036287028, -8.721835193296540112, 70.29165865351603770 ) ) ;
#4788 = DIRECTION ( 'NONE',  ( -0.000000000000000000, -1.000000000000000000, -0.000000000000000000 ) ) ;
#4789 = ORIENTED_EDGE ( 'NONE', *, *, #40163, .T. ) ;
#4790 = ORIENTED_EDGE ( 'NONE', *, *, #47039, .F. ) ;
#4791 = CARTESIAN_POINT ( 'NONE',  ( -21.17409385541304445, -6.859212275519751323, 50.50378509014259265 ) ) ;
#4792 = CIRCLE ( 'NONE', #3219, 1.999999999999999112 ) ;
#4793 = CARTESIAN_POINT ( 'NONE',  ( -13.43921731646364925, -8.993429882417945720, 60.43950277494440115 ) ) ;
#4794 = AXIS2_PLACEMENT_3D ( 'NONE', #23904, #35203, #1472 ) ;
#4795 = CARTESIAN_POINT ( 'NONE',  ( -23.39838849549200717, -11.16098491156533257, 73.66193259096606027 ) ) ;
#4796 = VECTOR ( 'NONE', #30248, 1000.000000000000227 ) ;
#4797 = PRODUCT_DEFINITION_SHAPE ( 'NONE', 'NONE',  #35187 ) ;
#4798 = CARTESIAN_POINT ( 'NONE',  ( -17.70936732686351789, -22.25382107568847800, 58.66199285276312025 ) ) ;
#4799 = CARTESIAN_POINT ( 'NONE',  ( -20.66848101912799862, -8.549761622307151754, 60.12653141481577990 ) ) ;
#4800 = CARTESIAN_POINT ( 'NONE',  ( -14.37051197998799523, -8.445983692038035784, 74.34387349308116200 ) ) ;
#4801 = VECTOR ( 'NONE', #38315, 1000.000000000000114 ) ;
#4802 = CARTESIAN_POINT ( 'NONE',  ( -18.18338144371267617, -21.81849904615365432, 65.63060065626805795 ) ) ;
#4803 = B_SPLINE_CURVE_WITH_KNOTS ( 'NONE', 1,
 ( #23074, #41781 ),
 .UNSPECIFIED., .F., .F.,
 ( 2, 2 ),
 ( 0.000000000000000000, 1.000000000000000000 ),
 .UNSPECIFIED. ) ;
#4804 = VERTEX_POINT ( 'NONE', #9487 ) ;
#4805 = CARTESIAN_POINT ( 'NONE',  ( -21.41781370759021641, -8.989828079956971862, 66.81716936885602820 ) ) ;
#4806 = DIRECTION ( 'NONE',  ( 0.9687793358424821033, -0.2479245821708680464, 0.000000000000000000 ) ) ;
#4807 = ORIENTED_EDGE ( 'NONE', *, *, #22365, .T. ) ;
#4808 = LINE ( 'NONE', #1333, #4834 ) ;
#4809 = CARTESIAN_POINT ( 'NONE',  ( -15.09544287645192462, -21.46351977604527761, 65.10596681500476279 ) ) ;
#4810 = EDGE_LOOP ( 'NONE', ( #17739, #8246, #7110, #6499, #19607 ) ) ;
#4811 = DIRECTION ( 'NONE',  ( 0.04287186434519785205, 0.9990805789562556827, -2.806673972535358096E-09 ) ) ;
#4812 = AXIS2_PLACEMENT_3D ( 'NONE', #41441, #48590, #40715 ) ;
#4813 = CARTESIAN_POINT ( 'NONE',  ( -19.79909385759798823, -8.105421454601382081, 49.25000573077640098 ) ) ;
#4814 = EDGE_CURVE ( 'NONE', #3385, #38648, #7737, .T. ) ;
#4815 = B_SPLINE_CURVE_WITH_KNOTS ( 'NONE', 1,
 ( #472, #41839 ),
 .UNSPECIFIED., .F., .F.,
 ( 2, 2 ),
 ( 0.000000000000000000, 1.000000000000000000 ),
 .UNSPECIFIED. ) ;
#4816 = CARTESIAN_POINT ( 'NONE',  ( -21.35994700726987006, -8.956524206332462157, 70.01643677269403554 ) ) ;
#4817 = CARTESIAN_POINT ( 'NONE',  ( -24.49273639735834607, -17.16277907914581036, 73.04369411581572535 ) ) ;
#4818 = ORIENTED_EDGE ( 'NONE', *, *, #21563, .T. ) ;
#4819 = CARTESIAN_POINT ( 'NONE',  ( -13.99679447977218061, -20.97040113148658591, 71.94079819673058296 ) ) ;
#4820 = CARTESIAN_POINT ( 'NONE',  ( -36.42409385541304800, -8.109206544743658540, 50.50000000000030553 ) ) ;
#4821 = CARTESIAN_POINT ( 'NONE',  ( -17.03658212107600534, -14.90837637761273449, 2.029618040566568027 ) ) ;
#4822 = FACE_BOUND ( 'NONE', #34508, .T. ) ;
#4823 = CONTEXT_DEPENDENT_SHAPE_REPRESENTATION ( #16162, #42148 ) ;
#4824 = AXIS2_PLACEMENT_3D ( 'NONE', #44459, #18326, #17836 ) ;
#4825 = CARTESIAN_POINT ( 'NONE',  ( -22.82696774913247495, -10.28001814127269320, 66.54742050011650178 ) ) ;
#4826 = CARTESIAN_POINT ( 'NONE',  ( -21.67055903134415473, -17.89628178023893668, 49.52966884056656482 ) ) ;
#4827 = AXIS2_PLACEMENT_3D ( 'NONE', #47691, #47938, #10278 ) ;
#4828 = CARTESIAN_POINT ( 'NONE',  ( -11.07857809310684516, -11.73724795245126096, 71.38860870961248395 ) ) ;
#4829 = VERTEX_POINT ( 'NONE', #27216 ) ;
#4830 = DIRECTION ( 'NONE',  ( -5.731567514496413899E-31, -1.020425574103664789E-16, -1.000000000000000000 ) ) ;
#4831 = ORIENTED_EDGE ( 'NONE', *, *, #46898, .F. ) ;
#4832 = CARTESIAN_POINT ( 'NONE',  ( -20.10030204730919223, -21.76202525863913451, 72.51983304728076973 ) ) ;
#4833 = ORIENTED_EDGE ( 'NONE', *, *, #11798, .T. ) ;
#4834 = VECTOR ( 'NONE', #19832, 1000.000000000000000 ) ;
#4835 = DIRECTION ( 'NONE',  ( -3.071710424422018668E-17, 6.404604876783312462E-16, 1.000000000000000000 ) ) ;
#4836 = CARTESIAN_POINT ( 'NONE',  ( -20.16798188746241394, -8.311166627122801742, 66.98924058670168336 ) ) ;
#4837 = B_SPLINE_CURVE_WITH_KNOTS ( 'NONE', 3,
 ( #26926, #30384, #38721, #1058, #46366, #19283, #23000, #19782, #16055, #31096 ),
 .UNSPECIFIED., .F., .F.,
 ( 4, 2, 2, 2, 4 ),
 ( 0.6272669072877714580, 0.7522669073072920654, 0.8772669073268126727, 1.002266907346333280, 1.127266907365853887 ),
 .UNSPECIFIED. ) ;
#4838 = ORIENTED_EDGE ( 'NONE', *, *, #42891, .F. ) ;
#4839 = VERTEX_POINT ( 'NONE', #46899 ) ;
#4840 = ORIENTED_EDGE ( 'NONE', *, *, #15217, .F. ) ;
#4841 = ADVANCED_FACE ( 'NONE', ( #31879 ), #42730, .T. ) ;
#4842 = LINE ( 'NONE', #35352, #6051 ) ;
#4843 = B_SPLINE_CURVE_WITH_KNOTS ( 'NONE', 3,
 ( #10362, #36192, #32514, #25372, #43858, #40383, #10112, #26102, #11081, #32971 ),
 .UNSPECIFIED., .F., .F.,
 ( 4, 2, 2, 2, 4 ),
 ( 0.6272669072782827149, 0.7522669073001686524, 0.8772669073220544789, 1.002266907343940527, 1.127266907365826354 ),
 .UNSPECIFIED. ) ;
#4844 = AXIS2_PLACEMENT_3D ( 'NONE', #30854, #45865, #23452 ) ;
#4845 = EDGE_CURVE ( 'NONE', #28161, #14388, #14672, .T. ) ;
#4846 = CARTESIAN_POINT ( 'NONE',  ( -24.43617598160173543, -14.07860879870782966, 73.12271522640413934 ) ) ;
#4847 =( BOUNDED_CURVE ( )  B_SPLINE_CURVE ( 3, ( #20285, #42457, #23499, #35047 ),
 .UNSPECIFIED., .F., .F. ) 
 B_SPLINE_CURVE_WITH_KNOTS ( ( 4, 4 ),
 ( 0.5000000000000000000, 0.9074455897393657322 ),
 .UNSPECIFIED. ) 
 CURVE ( )  GEOMETRIC_REPRESENTATION_ITEM ( )  RATIONAL_B_SPLINE_CURVE ( ( 1.000000000000004663, 0.4567392136813346326, 0.3561768502900279909, 0.6983129098260896228 ) ) 
 REPRESENTATION_ITEM ( '' )  );
#4848 = CARTESIAN_POINT ( 'NONE',  ( -14.56922799437018057, -8.416425268799397230, 67.33145281372107149 ) ) ;
#4849 = CARTESIAN_POINT ( 'NONE',  ( -10.68551981713787136, -12.73596763222149519, 64.28308208171728211 ) ) ;
#4850 = CARTESIAN_POINT ( 'NONE',  ( -10.50429924535250414, -16.15944446069506668, 71.46222527016213633 ) ) ;
#4851 = ORIENTED_EDGE ( 'NONE', *, *, #29922, .F. ) ;
#4852 = ORIENTED_EDGE ( 'NONE', *, *, #23913, .F. ) ;
#4853 = EDGE_CURVE ( 'NONE', #9098, #6412, #12695, .T. ) ;
#4854 = CARTESIAN_POINT ( 'NONE',  ( -21.65534385650552096, -7.417179338643134834, 52.18511593390279302 ) ) ;
#4855 = AXIS2_PLACEMENT_3D ( 'NONE', #12623, #574, #8704 ) ;
#4856 = CARTESIAN_POINT ( 'NONE',  ( -21.62450594022013206, -20.48119921038467695, 72.68013252948732372 ) ) ;
#4857 = CARTESIAN_POINT ( 'NONE',  ( -10.52311447087272178, -15.98309989773700046, 67.97767878683296772 ) ) ;
#4858 = FACE_BOUND ( 'NONE', #7355, .T. ) ;
#4859 = ORIENTED_EDGE ( 'NONE', *, *, #1268, .F. ) ;
#4860 = EDGE_CURVE ( 'NONE', #38039, #48382, #9998, .T. ) ;
#4861 =( BOUNDED_CURVE ( )  B_SPLINE_CURVE ( 3, ( #45353, #34741, #4962, #15277 ),
 .UNSPECIFIED., .F., .F. ) 
 B_SPLINE_CURVE_WITH_KNOTS ( ( 4, 4 ),
 ( 0.5000000000000000000, 0.9074455897393634007 ),
 .UNSPECIFIED. ) 
 CURVE ( )  GEOMETRIC_REPRESENTATION_ITEM ( )  RATIONAL_B_SPLINE_CURVE ( ( 1.000000000000004663, 0.4567392136813371861, 0.3561768502900288791, 0.6983129098260848489 ) ) 
 REPRESENTATION_ITEM ( '' )  );
#4862 = CARTESIAN_POINT ( 'NONE',  ( -13.13034385650551883, -9.794322478646142471, 51.19202720610083901 ) ) ;
#4863 =( BOUNDED_CURVE ( )  B_SPLINE_CURVE ( 3, ( #22118, #32696, #48203, #37106 ),
 .UNSPECIFIED., .F., .F. ) 
 B_SPLINE_CURVE_WITH_KNOTS ( ( 4, 4 ),
 ( 0.5000000000000000000, 0.9074455897393647330 ),
 .UNSPECIFIED. ) 
 CURVE ( )  GEOMETRIC_REPRESENTATION_ITEM ( )  RATIONAL_B_SPLINE_CURVE ( ( 0.9999999999999874545, 0.4567392136813364645, 0.3561768502900406475, 0.6983129098260862921 ) ) 
 REPRESENTATION_ITEM ( '' )  );
#4864 = ORIENTED_EDGE ( 'NONE', *, *, #8322, .T. ) ;
#4865 = AXIS2_PLACEMENT_3D ( 'NONE', #43262, #9529, #5829 ) ;
#4866 = DIRECTION ( 'NONE',  ( -2.671295504230222649E-06, -1.272698190446629743E-05, -0.9999999999154440822 ) ) ;
#4867 = CARTESIAN_POINT ( 'NONE',  ( 10.57590614458695377, 3.116243883476756515, 50.28399048308536123 ) ) ;
#4868 = VECTOR ( 'NONE', #4186, 1000.000000000000114 ) ;
#4869 = CARTESIAN_POINT ( 'NONE',  ( -12.51438871980625045, -19.79882953766492193, 65.16674880260835323 ) ) ;
#4870 = VERTEX_POINT ( 'NONE', #24020 ) ;
#4871 = CARTESIAN_POINT ( 'NONE',  ( -12.27729936708703384, -9.991218733798060470, 60.70918086709614414 ) ) ;
#4872 =( BOUNDED_SURFACE ( )  B_SPLINE_SURFACE ( 3, 1, ( 
 ( #11249, #26260 ),
 ( #45475, #11484 ),
 ( #18873, #33885 ),
 ( #31351, #16561 ),
 ( #44750, #7815 ),
 ( #20030, #38737 ),
 ( #23744, #5021 ) ),
 .UNSPECIFIED., .T., .F., .F. ) 
 B_SPLINE_SURFACE_WITH_KNOTS ( ( 4, 3, 4 ),
 ( 2, 2 ),
 ( 0.000000000000000000, 0.5000000000000000000, 1.000000000000000000 ),
 ( 0.000000000000000000, 1.000000000000000000 ),
 .UNSPECIFIED. ) 
 GEOMETRIC_REPRESENTATION_ITEM ( )  RATIONAL_B_SPLINE_SURFACE ( (
 ( 1.000000000000000000, 1.000000000000000000),
 ( 0.3333333333333335369, 0.3333333333333330373),
 ( 0.3333333333333335369, 0.3333333333333330373),
 ( 1.000000000000000000, 1.000000000000000000),
 ( 0.3333333333333333703, 0.3333333333333333703),
 ( 0.3333333333333333703, 0.3333333333333333703),
 ( 1.000000000000000000, 1.000000000000000000) ) ) 
 REPRESENTATION_ITEM ( '' )  SURFACE ( )  );
#4873 = CARTESIAN_POINT ( 'NONE',  ( -10.42394424466950476, -17.36098423042032124, 64.81394647623933736 ) ) ;
#4874 = CARTESIAN_POINT ( 'NONE',  ( -12.10369346210734243, -9.594120923840563364, 57.27430859790474926 ) ) ;
#4875 = ORIENTED_EDGE ( 'NONE', *, *, #18257, .T. ) ;
#4876 = AXIS2_PLACEMENT_3D ( 'NONE', #11695, #30668, #26960 ) ;
#4877 = CARTESIAN_POINT ( 'NONE',  ( -10.44050839523226060, -15.30664602827292775, 57.79622666356080174 ) ) ;
#4878 = ADVANCED_FACE ( 'NONE', ( #8998 ), #19838, .T. ) ;
#4879 = CARTESIAN_POINT ( 'NONE',  ( -24.82398108165943285, -15.67291706594333611, 73.18116521566574306 ) ) ;
#4880 = DIRECTION ( 'NONE',  ( 0.4332512900281776380, -0.1108752438054585870, -0.8944271909999159664 ) ) ;
#4881 = ORIENTED_EDGE ( 'NONE', *, *, #5603, .F. ) ;
#4882 = CARTESIAN_POINT ( 'NONE',  ( -15.95707209241614422, -7.504986913482371236, 63.85506412386598640 ) ) ;
#4883 = ORIENTED_EDGE ( 'NONE', *, *, #32459, .F. ) ;
#4884 = CARTESIAN_POINT ( 'NONE',  ( -9.974335981654279593, -14.73511362144080294, 71.50499609704121440 ) ) ;
#4885 = CARTESIAN_POINT ( 'NONE',  ( -24.32886716615087153, -16.23426984194678724, 62.60800820172418923 ) ) ;
#4886 = VERTEX_POINT ( 'NONE', #5296 ) ;
#4887 = CARTESIAN_POINT ( 'NONE',  ( -20.54979551517892489, -8.489990701729437816, 63.31121512946744190 ) ) ;
#4888 = CARTESIAN_POINT ( 'NONE',  ( -13.36114594230879504, -9.147054927169216754, 49.62380229257679076 ) ) ;
#4889 = CARTESIAN_POINT ( 'NONE',  ( -23.80338573481879294, -11.80731802715296297, 59.76763678108634537 ) ) ;
#4890 = CARTESIAN_POINT ( 'NONE',  ( -17.42409385541300182, -14.80920654474440745, 53.27966884056655061 ) ) ;
#4891 = ORIENTED_EDGE ( 'NONE', *, *, #1487, .F. ) ;
#4892 = CARTESIAN_POINT ( 'NONE',  ( -10.63483670088760924, -17.87674068094334245, 71.75213521449022380 ) ) ;
#4893 = CARTESIAN_POINT ( 'NONE',  ( -15.19549097431359463, -21.91815212410659086, 68.76088336006283441 ) ) ;
#4894 = DIRECTION ( 'NONE',  ( -0.7621627669932626858, 0.6473854467078884456, -3.680865981908973010E-08 ) ) ;
#4895 = DIRECTION ( 'NONE',  ( 2.866981220435666553E-17, -1.000000000000000000, -1.190614954331866791E-16 ) ) ;
#4896 = ORIENTED_EDGE ( 'NONE', *, *, #11648, .T. ) ;
#4897 = ADVANCED_FACE ( 'NONE', ( #31390 ), #1595, .T. ) ;
#4898 = CARTESIAN_POINT ( 'NONE',  ( 23.62590614458706639, 3.790747609047893540, 50.53028072113869484 ) ) ;
#4899 = CARTESIAN_POINT ( 'NONE',  ( -11.10470733248389230, -18.75498039752055490, 61.46206112672981448 ) ) ;
#4900 = EDGE_LOOP ( 'NONE', ( #46167, #32168 ) ) ;
#4901 = ORIENTED_EDGE ( 'NONE', *, *, #28234, .T. ) ;
#4902 = AXIS2_PLACEMENT_3D ( 'NONE', #599, #26216, #37270 ) ;
#4903 = FACE_OUTER_BOUND ( 'NONE', #23086, .T. ) ;
#4904 = CARTESIAN_POINT ( 'NONE',  ( -10.20016939456313843, -12.98476690782802834, 71.39483965270750332 ) ) ;
#4905 = FACE_OUTER_BOUND ( 'NONE', #41395, .T. ) ;
#4906 = CARTESIAN_POINT ( 'NONE',  ( -12.77466918460613599, -9.357823218138582533, 50.04127544294632912 ) ) ;
#4907 = CARTESIAN_POINT ( 'NONE',  ( -50.42409385541305511, -15.80920654474410725, 56.99999999999998579 ) ) ;
#4908 = B_SPLINE_CURVE_WITH_KNOTS ( 'NONE', 3,
 ( #45602, #41644, #42, #15027 ),
 .UNSPECIFIED., .F., .F.,
 ( 4, 4 ),
 ( 0.001041996463600835783, 0.002493317452643607161 ),
 .UNSPECIFIED. ) ;
#4909 = CARTESIAN_POINT ( 'NONE',  ( -12.36152504943391506, -19.64358911433177823, 58.15355758026139199 ) ) ;
#4910 = CARTESIAN_POINT ( 'NONE',  ( -10.71953686386422788, -16.98946087901043001, 57.98200754419831782 ) ) ;
#4911 = CARTESIAN_POINT ( 'NONE',  ( -9.975178868143471433, -14.94333879318065428, 74.91966125157830447 ) ) ;
#4912 = ORIENTED_EDGE ( 'NONE', *, *, #41674, .T. ) ;
#4913 = ORIENTED_EDGE ( 'NONE', *, *, #43854, .F. ) ;
#4914 = ADVANCED_FACE ( 'NONE', ( #42962 ), #9238, .T. ) ;
#4915 = CARTESIAN_POINT ( 'NONE',  ( -21.55883939963115026, -8.611815437115641458, 73.78624134823098757 ) ) ;
#4916 = SHAPE_REPRESENTATION_RELATIONSHIP ( 'NONE' , 'NONE' ,  #34550, #44394 ) ;
#4917 = ADVANCED_FACE ( 'NONE', ( #47629 ), #37912, .T. ) ;
#4918 = CARTESIAN_POINT ( 'NONE',  ( -11.90143264907557707, -10.50540407141871668, 74.54958359901495157 ) ) ;
#4919 = CARTESIAN_POINT ( 'NONE',  ( -13.65684165595416921, -8.849801312179289781, 56.98439896120441261 ) ) ;
#4920 = EDGE_CURVE ( 'NONE', #18177, #16383, #2735, .T. ) ;
#4921 = CARTESIAN_POINT ( 'NONE',  ( -21.92783717115298359, -9.450287623791650660, 59.72171200097150745 ) ) ;
#4922 = B_SPLINE_CURVE_WITH_KNOTS ( 'NONE', 3,
 ( #36168, #17696, #13754, #32723, #18423, #14235, #47750, #44319, #3418, #10338 ),
 .UNSPECIFIED., .F., .F.,
 ( 4, 2, 2, 2, 4 ),
 ( 0.1272669073658479755, 0.2522669073439446352, 0.3772669073220412672, 0.5022669073001380102, 0.6272669072782346422 ),
 .UNSPECIFIED. ) ;
#4923 = EDGE_LOOP ( 'NONE', ( #30848, #1354, #7789, #30467, #1364 ) ) ;
#4924 = B_SPLINE_CURVE_WITH_KNOTS ( 'NONE', 3,
 ( #2844, #33348, #17853, #29204, #25503, #29686, #32875, #41015, #10976, #26236 ),
 .UNSPECIFIED., .F., .F.,
 ( 4, 2, 2, 2, 4 ),
 ( 0.000000000000000000, 0.2500000000000000000, 0.5000000000000000000, 0.7500000000000000000, 1.000000000000000000 ),
 .UNSPECIFIED. ) ;
#4925 = DIRECTION ( 'NONE',  ( 1.000000000000000000, -4.164305804376849172E-17, 1.614929280266638808E-16 ) ) ;
#4926 = CARTESIAN_POINT ( 'NONE',  ( -24.47535868512742496, -14.65268306083313199, 66.59781357586173556 ) ) ;
#4927 = CARTESIAN_POINT ( 'NONE',  ( -36.42409385541304800, -8.109206544743658540, 50.50000000000030553 ) ) ;
#4928 = CARTESIAN_POINT ( 'NONE',  ( -11.05969852021412869, -18.68212028911960232, 61.43857375368525453 ) ) ;
#4929 = EDGE_CURVE ( 'NONE', #29888, #11159, #37004, .T. ) ;
#4930 = ORIENTED_EDGE ( 'NONE', *, *, #43440, .T. ) ;
#4931 = EDGE_CURVE ( 'NONE', #7384, #17465, #43953, .T. ) ;
#4932 = CARTESIAN_POINT ( 'NONE',  ( -12.99758330771203951, -9.386476247090117297, 70.84925353123610137 ) ) ;
#4933 = CYLINDRICAL_SURFACE ( 'NONE', #45620, 1.999999999999999556 ) ;
#4934 = EDGE_CURVE ( 'NONE', #29084, #10945, #28437, .T. ) ;
#4935 = EDGE_CURVE ( 'NONE', #41932, #891, #6297, .T. ) ;
#4936 = ORIENTED_EDGE ( 'NONE', *, *, #23398, .F. ) ;
#4937 = DIRECTION ( 'NONE',  ( -2.866981220435666553E-17, 1.000000000000000000, 1.190614954331866791E-16 ) ) ;
#4938 = CARTESIAN_POINT ( 'NONE',  ( -22.10541328151775886, -20.01527608457440266, 65.93251542687603717 ) ) ;
#4939 = ORIENTED_EDGE ( 'NONE', *, *, #1843, .F. ) ;
#4940 = CARTESIAN_POINT ( 'NONE',  ( -11.75774308769439003, -19.00384223356172697, 71.98685884781657762 ) ) ;
#4941 = VERTEX_POINT ( 'NONE', #43463 ) ;
#4942 = CARTESIAN_POINT ( 'NONE',  ( -18.53201889041905659, -7.846807422456379300, 73.99064401781672018 ) ) ;
#4943 = CARTESIAN_POINT ( 'NONE',  ( -21.61680475328812889, -8.650891705389904374, 73.85774703147257014 ) ) ;
#4944 = ORIENTED_EDGE ( 'NONE', *, *, #32394, .T. ) ;
#4945 = CARTESIAN_POINT ( 'NONE',  ( -24.84806299871600643, -14.18603056061780343, 69.69629353939886585 ) ) ;
#4946 = CARTESIAN_POINT ( 'NONE',  ( -45.98959949296318683, -14.20920654474410760, 69.94787228701220272 ) ) ;
#4947 = CARTESIAN_POINT ( 'NONE',  ( -16.76159385650551314, -9.295667164867525756, 49.30633214617472504 ) ) ;
#4948 = DIRECTION ( 'NONE',  ( -3.071710424422018668E-17, 6.404604876783312462E-16, 1.000000000000000000 ) ) ;
#4949 =( BOUNDED_CURVE ( )  B_SPLINE_CURVE ( 3, ( #5563, #20579, #35574, #1852 ),
 .UNSPECIFIED., .F., .F. ) 
 B_SPLINE_CURVE_WITH_KNOTS ( ( 4, 4 ),
 ( 1.570796326794896558, 1.780235837034217505 ),
 .UNSPECIFIED. ) 
 CURVE ( )  GEOMETRIC_REPRESENTATION_ITEM ( )  RATIONAL_B_SPLINE_CURVE ( ( 1.000000000000000000, 0.9963479302455154896, 0.9963479302455154896, 1.000000000000000000 ) ) 
 REPRESENTATION_ITEM ( '' )  );
#4950 = CARTESIAN_POINT ( 'NONE',  ( -10.53392471227544114, -17.64261015482012596, 68.29733140449641837 ) ) ;
#4951 = CARTESIAN_POINT ( 'NONE',  ( -16.97945985512182787, -21.84517132341290591, 72.16543221430227106 ) ) ;
#4952 = ORIENTED_EDGE ( 'NONE', *, *, #45619, .F. ) ;
#4953 = LINE ( 'NONE', #35931, #31027 ) ;
#4954 = DIRECTION ( 'NONE',  ( -3.071710424422018668E-17, 6.404604876783312462E-16, 1.000000000000000000 ) ) ;
#4955 = DIRECTION ( 'NONE',  ( -6.516572651863732626E-06, 8.834921937557814562E-06, 0.9999999999397393147 ) ) ;
#4956 = CYLINDRICAL_SURFACE ( 'NONE', #31368, 2.000000000000001776 ) ;
#4957 = FACE_OUTER_BOUND ( 'NONE', #45369, .T. ) ;
#4958 = ADVANCED_FACE ( 'NONE', ( #47867 ), #26274, .T. ) ;
#4959 = EDGE_LOOP ( 'NONE', ( #1996, #27566 ) ) ;
#4960 = ORIENTED_EDGE ( 'NONE', *, *, #3403, .T. ) ;
#4961 = CARTESIAN_POINT ( 'NONE',  ( -14.92409385541305333, -14.80920654474411080, 47.99999999999997868 ) ) ;
#4962 = CARTESIAN_POINT ( 'NONE',  ( -12.03360233570622739, -10.25976192134970866, 71.26893272426330839 ) ) ;
#4963 = ORIENTED_EDGE ( 'NONE', *, *, #16541, .T. ) ;
#4964 = CARTESIAN_POINT ( 'NONE',  ( -22.43322805121811214, -20.32484237088842249, 65.89077003248591780 ) ) ;
#4965 = CARTESIAN_POINT ( 'NONE',  ( -21.03659385759798894, -8.995762431863214559, 51.38120296130585274 ) ) ;
#4966 = CARTESIAN_POINT ( 'NONE',  ( -10.46764514157213455, -15.58883556682774874, 57.67678839390069356 ) ) ;
#4967 = CARTESIAN_POINT ( 'NONE',  ( -10.63483670088760924, -17.87674068094334245, 71.75213521449022380 ) ) ;
#4968 = DIRECTION ( 'NONE',  ( -3.071710424422018668E-17, 6.404604876783312462E-16, 1.000000000000000000 ) ) ;
#4969 = CARTESIAN_POINT ( 'NONE',  ( -19.39825701701550287, -7.625522893467396202, 60.16081771123726440 ) ) ;
#4970 = ORIENTED_EDGE ( 'NONE', *, *, #40500, .F. ) ;
#4971 = EDGE_CURVE ( 'NONE', #2683, #42051, #29396, .T. ) ;
#4972 = CARTESIAN_POINT ( 'NONE',  ( -22.63560595208270954, -20.13310736574185000, 69.28922662766110818 ) ) ;
#4973 = CARTESIAN_POINT ( 'NONE',  ( -19.17604249790256077, -21.63836284480991878, 58.53979515915469278 ) ) ;
#4974 = CARTESIAN_POINT ( 'NONE',  ( -22.62394951084894146, -10.04809318868971424, 70.29706442286226320 ) ) ;
#4975 = CARTESIAN_POINT ( 'NONE',  ( -24.72409385541305582, -14.90920654474421170, 67.05882352941175384 ) ) ;
#4976 = CARTESIAN_POINT ( 'NONE',  ( -12.72909403660860228, -20.00294204248303132, 72.03483503000991561 ) ) ;
#4977 = B_SPLINE_CURVE_WITH_KNOTS ( 'NONE', 3,
 ( #45594, #11845, #26872, #42853, #16723, #1961, #5906, #46558, #12799, #19957 ),
 .UNSPECIFIED., .F., .F.,
 ( 4, 2, 2, 2, 4 ),
 ( 0.000000000000000000, 0.2500000000000000000, 0.5000000000000000000, 0.7500000000000000000, 1.000000000000000000 ),
 .UNSPECIFIED. ) ;
#4978 = EDGE_LOOP ( 'NONE', ( #25522, #46717, #10806, #4901, #36560 ) ) ;
#4979 = ORIENTED_EDGE ( 'NONE', *, *, #48622, .F. ) ;
#4980 = CARTESIAN_POINT ( 'NONE',  ( -21.73659385650551812, -6.915538690918074494, 49.31353937987644542 ) ) ;
#4981 = VERTEX_POINT ( 'NONE', #14101 ) ;
#4982 = FACE_OUTER_BOUND ( 'NONE', #27478, .T. ) ;
#4983 = DIRECTION ( 'NONE',  ( -9.632611953450936153E-07, 3.816342149705755051E-07, 0.9999999999994632072 ) ) ;
#4984 = VERTEX_POINT ( 'NONE', #6015 ) ;
#4985 = EDGE_CURVE ( 'NONE', #29698, #14925, #25223, .T. ) ;
#4986 = CARTESIAN_POINT ( 'NONE',  ( -16.34301583228449317, -10.23680828416977739, 49.52966884056655772 ) ) ;
#4987 = CARTESIAN_POINT ( 'NONE',  ( -11.22844613476422460, -11.44458948612160043, 64.43409918096024569 ) ) ;
#4988 = EDGE_CURVE ( 'NONE', #40480, #18094, #817, .T. ) ;
#4989 = ADVANCED_FACE ( 'NONE', ( #14338 ), #7735, .T. ) ;
#4990 = VECTOR ( 'NONE', #20067, 1000.000000000000000 ) ;
#4991 = ORIENTED_EDGE ( 'NONE', *, *, #7776, .T. ) ;
#4992 = CARTESIAN_POINT ( 'NONE',  ( -18.09515488393238414, -21.82723660550677636, 65.34532171799240530 ) ) ;
#4993 = DIRECTION ( 'NONE',  ( -0.2393306345705715765, -0.3777841279832278021, 0.8944271909999157444 ) ) ;
#4994 = ORIENTED_EDGE ( 'NONE', *, *, #43497, .F. ) ;
#4995 =( BOUNDED_CURVE ( )  B_SPLINE_CURVE ( 3, ( #9081, #31956, #13707, #17415 ),
 .UNSPECIFIED., .F., .F. ) 
 B_SPLINE_CURVE_WITH_KNOTS ( ( 4, 4 ),
 ( 6.147240100468659207, 6.419130513890513257 ),
 .UNSPECIFIED. ) 
 CURVE ( )  GEOMETRIC_REPRESENTATION_ITEM ( )  RATIONAL_B_SPLINE_CURVE ( ( 1.000000000000000000, 0.9938491152766115722, 0.9938491152766115722, 1.000000000000000000 ) ) 
 REPRESENTATION_ITEM ( '' )  );
#4996 = DIRECTION ( 'NONE',  ( 3.549360974554993999E-17, -6.371834667797928663E-18, -1.000000000000000000 ) ) ;
#4997 = ORIENTED_EDGE ( 'NONE', *, *, #39785, .F. ) ;
#4998 = EDGE_CURVE ( 'NONE', #2922, #41672, #42951, .T. ) ;
#4999 = EDGE_CURVE ( 'NONE', #33324, #46845, #34286, .T. ) ;
#5000 = CARTESIAN_POINT ( 'NONE',  ( -23.00190342510993347, -19.12578814502481350, 62.76895730438863552 ) ) ;
#5001 = CARTESIAN_POINT ( 'NONE',  ( -22.23721589179859492, -20.49593378876094718, 58.92476249817150347 ) ) ;
#5002 = CARTESIAN_POINT ( 'NONE',  ( 9.825906144586950219, -6.109215713985405749, 50.50605614422795497 ) ) ;
#5003 = VERTEX_POINT ( 'NONE', #45652 ) ;
#5004 = CARTESIAN_POINT ( 'NONE',  ( -45.92409385541306222, -14.20920654474410760, 70.50000000000000000 ) ) ;
#5005 = CARTESIAN_POINT ( 'NONE',  ( -21.68495691188242702, -20.43592993620880804, 58.90875877921045145 ) ) ;
#5006 = CARTESIAN_POINT ( 'NONE',  ( -14.81535805098777736, -7.777528402031248511, 47.99999999999994316 ) ) ;
#5007 = CARTESIAN_POINT ( 'NONE',  ( -20.72253465480533308, -21.04901898548487793, 65.72887014617839441 ) ) ;
#5008 = B_SPLINE_CURVE_WITH_KNOTS ( 'NONE', 3,
 ( #24232, #13597, #39969, #17300, #1811, #9209, #16574, #6239, #5764, #2051 ),
 .UNSPECIFIED., .F., .F.,
 ( 4, 2, 2, 2, 4 ),
 ( 0.1272669073658179995, 0.2522669073463016942, 0.3772669073267853612, 0.5022669073072690837, 0.6272669072877528063 ),
 .UNSPECIFIED. ) ;
#5009 = CARTESIAN_POINT ( 'NONE',  ( -10.96921284960095377, -11.97350354382807680, 74.84368195529052059 ) ) ;
#5011 =( BOUNDED_CURVE ( )  B_SPLINE_CURVE ( 3, ( #22749, #8441, #37488, #19523 ),
 .UNSPECIFIED., .F., .F. ) 
 B_SPLINE_CURVE_WITH_KNOTS ( ( 4, 4 ),
 ( 0.4074455897393670090, 0.5000000000000000000 ),
 .UNSPECIFIED. ) 
 CURVE ( )  GEOMETRIC_REPRESENTATION_ITEM ( )  RATIONAL_B_SPLINE_CURVE ( ( 0.6983129098260917322, 0.7760317562606943165, 0.8765941196519962952, 0.9999999999999956701 ) ) 
 REPRESENTATION_ITEM ( '' )  );
#5010 = DIRECTION ( 'NONE',  ( -0.9687793358424821033, 0.2479245821708679909, 0.000000000000000000 ) ) ;
#5012 = CARTESIAN_POINT ( 'NONE',  ( -10.39634573379212767, -15.41385649924959544, 61.33789215671617967 ) ) ;
#5013 = CARTESIAN_POINT ( 'NONE',  ( -20.16691314815865255, -21.73601827195274794, 72.58974169946205279 ) ) ;
#5014 = CARTESIAN_POINT ( 'NONE',  ( -17.79909385650551812, -8.114302828567740988, 52.18300498402516041 ) ) ;
#5015 = EDGE_CURVE ( 'NONE', #20388, #19733, #28907, .T. ) ;
#5016 = EDGE_LOOP ( 'NONE', ( #16870, #20143, #8141, #34815, #36800 ) ) ;
#5017 = CARTESIAN_POINT ( 'NONE',  ( -21.84079957929829874, -9.314189696129256291, 63.19153755727188582 ) ) ;
#5018 = CARTESIAN_POINT ( 'NONE',  ( -12.50776634899986384, -20.40684016789016297, 71.92158251742569064 ) ) ;
#5019 = EDGE_LOOP ( 'NONE', ( #15002, #37109, #24074, #47920, #12714 ) ) ;
#5020 = FACE_OUTER_BOUND ( 'NONE', #48369, .T. ) ;
#5021 = CARTESIAN_POINT ( 'NONE',  ( -14.41428275390769365, -7.994163218335415877, 63.97474169571218283 ) ) ;
#5022 = CARTESIAN_POINT ( 'NONE',  ( -44.72480688026392670, -12.91120565595568870, 70.87000000000000455 ) ) ;
#5023 = CARTESIAN_POINT ( 'NONE',  ( -12.27729925481933471, -9.991218852276041673, 60.55918086709623083 ) ) ;
#5024 = CYLINDRICAL_SURFACE ( 'NONE', #48616, 0.1499999999999971634 ) ;
#5025 = ORIENTED_EDGE ( 'NONE', *, *, #44136, .F. ) ;
#5026 = DIRECTION ( 'NONE',  ( 0.000000000000000000, 0.000000000000000000, 1.000000000000000000 ) ) ;
#5027 = CARTESIAN_POINT ( 'NONE',  ( -24.42421134999058552, -14.80068637069104653, 59.54300242294779366 ) ) ;
#5028 = CARTESIAN_POINT ( 'NONE',  ( -10.09536215149225491, -16.14886288462728459, 68.11621278793219858 ) ) ;
#5029 = VERTEX_POINT ( 'NONE', #37986 ) ;
#5030 = CARTESIAN_POINT ( 'NONE',  ( -18.08884787034790875, -9.601462109806339740, 50.77966884056655772 ) ) ;
#5031 = DIRECTION ( 'NONE',  ( 0.000000000000000000, 1.000000000000000000, -0.000000000000000000 ) ) ;
#5032 = CARTESIAN_POINT ( 'NONE',  ( -12.76547314785493192, -9.517330534081262172, 74.60450883341005124 ) ) ;
#5033 = DIRECTION ( 'NONE',  ( 1.616182858256118536E-16, 0.003028072113822188795, -0.9999954153791273948 ) ) ;
#5034 = CYLINDRICAL_SURFACE ( 'NONE', #44890, 2.000000000000001776 ) ;
#5035 = EDGE_LOOP ( 'NONE', ( #37757, #22593, #27606, #40868 ) ) ;
#5036 = ORIENTED_EDGE ( 'NONE', *, *, #47835, .T. ) ;
#5037 = CARTESIAN_POINT ( 'NONE',  ( -20.21784385541304374, -6.860780111191487229, 51.02154966934377001 ) ) ;
#5038 = CARTESIAN_POINT ( 'NONE',  ( -10.74573065459234478, -12.54952415110468422, 60.81325645027152405 ) ) ;
#5039 = CARTESIAN_POINT ( 'NONE',  ( -14.11538500997439627, -8.134069317748153338, 70.86924253296322718 ) ) ;
#5040 = CARTESIAN_POINT ( 'NONE',  ( -17.04413539470110095, -21.84925844046378174, 72.45071136019464575 ) ) ;
#5041 = ADVANCED_FACE ( 'NONE', ( #45165 ), #41203, .T. ) ;
#5042 = CARTESIAN_POINT ( 'NONE',  ( -15.53265176333180619, -21.60105060138385369, 72.33103357390284316 ) ) ;
#5043 = ORIENTED_EDGE ( 'NONE', *, *, #10709, .F. ) ;
#5044 = CARTESIAN_POINT ( 'NONE',  ( -14.01837044221388595, -8.636059239884618322, 74.48482605064899076 ) ) ;
#5045 = FACE_OUTER_BOUND ( 'NONE', #44134, .T. ) ;
#5046 = ORIENTED_EDGE ( 'NONE', *, *, #24633, .T. ) ;
#5047 = CARTESIAN_POINT ( 'NONE',  ( -22.43986228125061544, -19.69212616369310354, 69.24706122172230494 ) ) ;
#5048 = PLANE ( 'NONE',  #11789 ) ;
#5049 = AXIS2_PLACEMENT_3D ( 'NONE', #15588, #11927, #29910 ) ;
#5051 = ORIENTED_EDGE ( 'NONE', *, *, #2452, .F. ) ;
#5050 =( BOUNDED_CURVE ( )  B_SPLINE_CURVE ( 3, ( #37382, #14061, #15224, #32562 ),
 .UNSPECIFIED., .F., .F. ) 
 B_SPLINE_CURVE_WITH_KNOTS ( ( 4, 4 ),
 ( 1.570796326794896558, 1.780235837034217505 ),
 .UNSPECIFIED. ) 
 CURVE ( )  GEOMETRIC_REPRESENTATION_ITEM ( )  RATIONAL_B_SPLINE_CURVE ( ( 1.000000000000000000, 0.9963479302455154896, 0.9963479302455154896, 1.000000000000000000 ) ) 
 REPRESENTATION_ITEM ( '' )  );
#5052 = EDGE_CURVE ( 'NONE', #33382, #17990, #3526, .T. ) ;
#5053 = ADVANCED_FACE ( 'NONE', ( #10927 ), #11405, .F. ) ;
#5054 = CARTESIAN_POINT ( 'NONE',  ( -10.80730693270912468, -17.26544268483686650, 57.84327589213576459 ) ) ;
#5055 = CARTESIAN_POINT ( 'NONE',  ( -20.31443949084103906, -8.433657969208125493, 67.08104076698165841 ) ) ;
#5056 = VERTEX_POINT ( 'NONE', #19281 ) ;
#5057 = CARTESIAN_POINT ( 'NONE',  ( -14.03870967672415304, -8.172720116890397790, 70.91453050697840865 ) ) ;
#5058 = AXIS2_PLACEMENT_3D ( 'NONE', #37749, #38224, #34053 ) ;
#5059 = EDGE_CURVE ( 'NONE', #37287, #30155, #23233, .T. ) ;
#5060 = CARTESIAN_POINT ( 'NONE',  ( -10.00761947527410634, -15.51609109068450465, 57.75288224187332276 ) ) ;
#5061 = ADVANCED_FACE ( 'NONE', ( #30629 ), #18290, .T. ) ;
#5062 = CARTESIAN_POINT ( 'NONE',  ( -21.78913871579879569, -8.771809629715434653, 70.24637254705723421 ) ) ;
#5063 = CARTESIAN_POINT ( 'NONE',  ( -24.46683668533210110, -14.41599144169055258, 62.71296521563537141 ) ) ;
#5064 = EDGE_LOOP ( 'NONE', ( #19498, #22237, #1721, #47699 ) ) ;
#5065 = DIRECTION ( 'NONE',  ( -3.071710424422018668E-17, 6.404604876783312462E-16, 1.000000000000000000 ) ) ;
#5066 = CARTESIAN_POINT ( 'NONE',  ( -22.96375064570672819, -10.44813988596692589, 63.08658113699938497 ) ) ;
#5067 = CARTESIAN_POINT ( 'NONE',  ( -10.90414816633800399, -11.20463157964466205, 64.24858404949443980 ) ) ;
#5068 = CARTESIAN_POINT ( 'NONE',  ( -22.60969001043771698, -13.98939405582217255, 50.77966884056655772 ) ) ;
#5069 = SHAPE_DEFINITION_REPRESENTATION ( #7948, #5940 ) ;
#5070 = CARTESIAN_POINT ( 'NONE',  ( -42.07024770156689897, -25.10920654474410441, 65.83076923076922071 ) ) ;
#5071 = DIRECTION ( 'NONE',  ( 0.6478992145799702396, -0.7617260713318518839, 1.927832152310587483E-08 ) ) ;
#5072 = EDGE_CURVE ( 'NONE', #10114, #18224, #21251, .T. ) ;
#5073 = CARTESIAN_POINT ( 'NONE',  ( -24.40658499505740053, -15.78250870199476630, 69.83307488408829045 ) ) ;
#5074 = VERTEX_POINT ( 'NONE', #48588 ) ;
#5075 = CARTESIAN_POINT ( 'NONE',  ( -10.71495605983455590, -12.81234157828920850, 64.26836111193937029 ) ) ;
#5076 = EDGE_LOOP ( 'NONE', ( #34521, #6510 ) ) ;
#5077 = CARTESIAN_POINT ( 'NONE',  ( -19.85891393954322837, -21.37210614461000446, 47.99999999999994316 ) ) ;
#5078 = CARTESIAN_POINT ( 'NONE',  ( -14.65765131015531253, -21.78034674156931061, 47.99999999999994316 ) ) ;
#5079 = ORIENTED_EDGE ( 'NONE', *, *, #21021, .T. ) ;
#5080 = DIRECTION ( 'NONE',  ( 0.9862050927915948506, 0.1655279884246635136, 7.765682856207885122E-08 ) ) ;
#5081 = FACE_BOUND ( 'NONE', #1218, .T. ) ;
#5082 = ORIENTED_EDGE ( 'NONE', *, *, #14082, .T. ) ;
#5083 = VERTEX_POINT ( 'NONE', #14821 ) ;
#5084 = ORIENTED_EDGE ( 'NONE', *, *, #27009, .F. ) ;
#5085 = CARTESIAN_POINT ( 'NONE',  ( -10.02191638112385697, -15.65273889608829982, 61.15293747381159761 ) ) ;
#5086 = B_SPLINE_CURVE_WITH_KNOTS ( 'NONE', 3,
 ( #20985, #2269, #13808, #24456, #31827, #43157, #39459, #5742, #2026, #17021 ),
 .UNSPECIFIED., .F., .F.,
 ( 4, 2, 2, 2, 4 ),
 ( 0.1272669073657571592, 0.2522669073462757705, 0.3772669073267943540, 0.5022669073073130486, 0.6272669072878316321 ),
 .UNSPECIFIED. ) ;
#5087 = CARTESIAN_POINT ( 'NONE',  ( -22.09321184435721719, -14.28490438881294367, 49.52966884056655772 ) ) ;
#5088 = DIRECTION ( 'NONE',  ( 0.000000000000000000, 0.000000000000000000, 1.000000000000000000 ) ) ;
#5089 = CARTESIAN_POINT ( 'NONE',  ( -24.83263378688676326, -15.59489965655864374, 73.18799144572807336 ) ) ;
#5090 = ORIENTED_EDGE ( 'NONE', *, *, #35204, .F. ) ;
#5091 = ORIENTED_EDGE ( 'NONE', *, *, #48551, .T. ) ;
#5092 = VECTOR ( 'NONE', #20650, 1000.000000000000114 ) ;
#5093 = CARTESIAN_POINT ( 'NONE',  ( -22.94909385650551314, -8.104110260919577868, 48.81699501597546487 ) ) ;
#5094 = AXIS2_PLACEMENT_3D ( 'NONE', #2281, #13586, #17288 ) ;
#5095 = CARTESIAN_POINT ( 'NONE',  ( -22.68646401470678953, -20.08284273627726435, 69.35913316877790180 ) ) ;
#5096 = CYLINDRICAL_SURFACE ( 'NONE', #7952, 0.1500000000000072387 ) ;
#5097 = CARTESIAN_POINT ( 'NONE',  ( -28.05565061734489873, -15.48652051201079516, 54.60745305979834541 ) ) ;
#5098 = ORIENTED_EDGE ( 'NONE', *, *, #4295, .T. ) ;
#5099 = EDGE_CURVE ( 'NONE', #28201, #20914, #7492, .T. ) ;
#5100 = CARTESIAN_POINT ( 'NONE',  ( -21.20534385650551812, -8.801233750844183135, 48.81488406609782515 ) ) ;
#5101 = ORIENTED_EDGE ( 'NONE', *, *, #16858, .F. ) ;
#5102 = CARTESIAN_POINT ( 'NONE',  ( -23.08463473158306556, -10.68898933584892674, 59.67373781969178737 ) ) ;
#5103 = ADVANCED_FACE ( 'NONE', ( #34046 ), #37489, .T. ) ;
#5104 = LINE ( 'NONE', #45506, #26905 ) ;
#5105 = CARTESIAN_POINT ( 'NONE',  ( -24.48028110873323726, -17.19936403064268760, 73.08324815060153412 ) ) ;
#5106 = EDGE_LOOP ( 'NONE', ( #6737, #10786, #43845, #44023 ) ) ;
#5107 = CARTESIAN_POINT ( 'NONE',  ( -10.87811525140410929, -17.44835992831754368, 61.31310265544169624 ) ) ;
#5108 = DIRECTION ( 'NONE',  ( 5.224165695523869193E-06, -4.853366963026260877E-07, -0.9999999999862362321 ) ) ;
#5109 = CARTESIAN_POINT ( 'NONE',  ( -22.82502255886352671, -19.94079571721461264, 72.75062258121896264 ) ) ;
#5110 = EDGE_CURVE ( 'NONE', #15426, #6917, #99, .T. ) ;
#5111 = ORIENTED_EDGE ( 'NONE', *, *, #45957, .T. ) ;
#5112 = CARTESIAN_POINT ( 'NONE',  ( -8.424093855413067544, -6.859206544744110623, 50.49999999999999289 ) ) ;
#5113 = EDGE_CURVE ( 'NONE', #10119, #6712, #4035, .T. ) ;
#5114 = CARTESIAN_POINT ( 'NONE',  ( -22.72031779163844334, -16.29245029320677673, 54.07175714974878389 ) ) ;
#5115 = CARTESIAN_POINT ( 'NONE',  ( -20.69509153224808173, -8.115601224564374050, 63.49616927690831858 ) ) ;
#5116 = ORIENTED_EDGE ( 'NONE', *, *, #9768, .F. ) ;
#5117 = DIRECTION ( 'NONE',  ( 6.258914665795302800E-07, -5.777405081385165423E-07, -0.9999999999996371791 ) ) ;
#5118 = EDGE_LOOP ( 'NONE', ( #9798, #41670, #35586, #18025 ) ) ;
#5119 = VECTOR ( 'NONE', #36482, 1000.000000000000114 ) ;
#5120 = CARTESIAN_POINT ( 'NONE',  ( -19.61601346313181082, -21.50980264518277707, 65.46486213821819433 ) ) ;
#5121 = CARTESIAN_POINT ( 'NONE',  ( -23.74619244455238487, -11.68933966055485030, 63.25218278636740621 ) ) ;
#5122 = EDGE_CURVE ( 'NONE', #24550, #14223, #45032, .T. ) ;
#5123 = EDGE_LOOP ( 'NONE', ( #28183, #13041, #41794, #32534, #30987 ) ) ;
#5124 = CARTESIAN_POINT ( 'NONE',  ( -21.76243611580424897, -17.76577320756515022, 50.77966884056655772 ) ) ;
#5125 = CARTESIAN_POINT ( 'NONE',  ( -10.42546172544805039, -12.25520447285018122, 57.44362008841285672 ) ) ;
#5126 = CIRCLE ( 'NONE', #37324, 5.249999999999998224 ) ;
#5127 = DIRECTION ( 'NONE',  ( -3.071710424422018668E-17, 6.404604876783312462E-16, 1.000000000000000000 ) ) ;
#5128 = CARTESIAN_POINT ( 'NONE',  ( -42.18144679658953322, -14.80920654474417830, 64.94117647058821774 ) ) ;
#5129 = ORIENTED_EDGE ( 'NONE', *, *, #14743, .F. ) ;
#5130 = CARTESIAN_POINT ( 'NONE',  ( -10.60570763719787735, -17.81143699334987218, 71.68222866232767387 ) ) ;
#5131 = EDGE_CURVE ( 'NONE', #24042, #19458, #22682, .T. ) ;
#5132 =( BOUNDED_CURVE ( )  B_SPLINE_CURVE ( 3, ( #39965, #28155, #36256, #21728 ),
 .UNSPECIFIED., .F., .F. ) 
 B_SPLINE_CURVE_WITH_KNOTS ( ( 4, 4 ),
 ( 1.570796326794896780, 1.780235837034217727 ),
 .UNSPECIFIED. ) 
 CURVE ( )  GEOMETRIC_REPRESENTATION_ITEM ( )  RATIONAL_B_SPLINE_CURVE ( ( 1.000000000000000000, 0.9963479302455154896, 0.9963479302455154896, 1.000000000000000000 ) ) 
 REPRESENTATION_ITEM ( '' )  );
#5133 = DIRECTION ( 'NONE',  ( 5.297746385098606630E-06, 8.914243324979344743E-06, 0.9999999999462350075 ) ) ;
#5134 = CARTESIAN_POINT ( 'NONE',  ( -22.28911595143133439, -9.166815984689403507, 59.86137841136315529 ) ) ;
#5135 = ORIENTED_EDGE ( 'NONE', *, *, #20935, .T. ) ;
#5136 = CARTESIAN_POINT ( 'NONE',  ( -15.89079584495563502, -7.517933547575396780, 67.32662675182959333 ) ) ;
#5137 = CARTESIAN_POINT ( 'NONE',  ( -11.24997143734453076, -18.22902874506724302, 61.42143955951387113 ) ) ;
#5138 = ORIENTED_EDGE ( 'NONE', *, *, #5336, .F. ) ;
#5139 = ORIENTED_EDGE ( 'NONE', *, *, #16358, .T. ) ;
#5140 = FACE_OUTER_BOUND ( 'NONE', #32706, .T. ) ;
#5141 = CARTESIAN_POINT ( 'NONE',  ( -13.22529448846758804, -9.145569705956512863, 64.19474388871357462 ) ) ;
#5142 = CARTESIAN_POINT ( 'NONE',  ( -11.42787535746950667, -18.52272177604094239, 57.69225786326394001 ) ) ;
#5143 = CARTESIAN_POINT ( 'NONE',  ( -13.33034385759799001, -6.857644439848014528, 49.98602051094140819 ) ) ;
#5144 = CARTESIAN_POINT ( 'NONE',  ( -40.92409385541305511, -14.80920654474410725, 74.99999999999998579 ) ) ;
#5145 = CARTESIAN_POINT ( 'NONE',  ( -23.84653597794508784, -18.58622903642730151, 72.87712840465626130 ) ) ;
#5146 = CARTESIAN_POINT ( 'NONE',  ( -19.71364512540636582, -21.89872317270189939, 65.57212061471852849 ) ) ;
#5147 =( BOUNDED_CURVE ( )  B_SPLINE_CURVE ( 3, ( #15423, #38321, #30491, #34388 ),
 .UNSPECIFIED., .F., .F. ) 
 B_SPLINE_CURVE_WITH_KNOTS ( ( 4, 4 ),
 ( 0.5000000000000000000, 0.9074455897393605142 ),
 .UNSPECIFIED. ) 
 CURVE ( )  GEOMETRIC_REPRESENTATION_ITEM ( )  RATIONAL_B_SPLINE_CURVE ( ( 1.000000000000018430, 0.4567392136813420711, 0.3561768502900211075, 0.6983129098260754120 ) ) 
 REPRESENTATION_ITEM ( '' )  );
#5148 = CARTESIAN_POINT ( 'NONE',  ( -22.96481576609224717, -19.16891988936071556, 58.89882756593014790 ) ) ;
#5149 = EDGE_LOOP ( 'NONE', ( #9774, #44002 ) ) ;
#5150 = VERTEX_POINT ( 'NONE', #30871 ) ;
#5151 = CARTESIAN_POINT ( 'NONE',  ( -10.96921284960095555, -11.97350354382807680, 74.84368195529052059 ) ) ;
#5152 =( LENGTH_UNIT ( ) NAMED_UNIT ( * ) SI_UNIT ( .MILLI., .METRE. ) );
#5153 = CARTESIAN_POINT ( 'NONE',  ( -20.96187357126569850, -17.88286835634646721, 49.52966884056655772 ) ) ;
#5154 = CARTESIAN_POINT ( 'NONE',  ( -23.21283044961208830, -10.11939778159179859, 63.25681392212788268 ) ) ;
#5155 = DIRECTION ( 'NONE',  ( 0.05202058437830281434, -0.9986460127597465153, 1.657953767687799911E-08 ) ) ;
#5156 = EDGE_CURVE ( 'NONE', #31006, #17131, #42045, .T. ) ;
#5157 =( BOUNDED_CURVE ( )  B_SPLINE_CURVE ( 3, ( #19038, #37982, #23726, #46112 ),
 .UNSPECIFIED., .F., .F. ) 
 B_SPLINE_CURVE_WITH_KNOTS ( ( 4, 4 ),
 ( 0.5000000000000000000, 0.9074455897393653991 ),
 .UNSPECIFIED. ) 
 CURVE ( )  GEOMETRIC_REPRESENTATION_ITEM ( )  RATIONAL_B_SPLINE_CURVE ( ( 1.000000000000033973, 0.4567392136813364090, 0.3561768502900080069, 0.6983129098260858481 ) ) 
 REPRESENTATION_ITEM ( '' )  );
#5158 = AXIS2_PLACEMENT_3D ( 'NONE', #3436, #36911, #32513 ) ;
#5159 = ORIENTED_EDGE ( 'NONE', *, *, #20645, .T. ) ;
#5160 = CARTESIAN_POINT ( 'NONE',  ( -15.06868085595426621, -21.40102190336860488, 61.82703723969883924 ) ) ;
#5161 = CARTESIAN_POINT ( 'NONE',  ( -23.28952267755650851, -10.88343168269180339, 73.51760210707182353 ) ) ;
#5162 = CARTESIAN_POINT ( 'NONE',  ( -15.52406250999510817, -21.54653527486415854, 72.34575433013422696 ) ) ;
#5163 = CARTESIAN_POINT ( 'NONE',  ( -15.82941474652824176, -7.531753325696857182, 67.31820067426403398 ) ) ;
#5164 = ORIENTED_EDGE ( 'NONE', *, *, #40278, .T. ) ;
#5165 = CARTESIAN_POINT ( 'NONE',  ( -24.84793648988037518, -14.18443574041886457, 69.83770584630335065 ) ) ;
#5166 = B_SPLINE_CURVE_WITH_KNOTS ( 'NONE', 3,
 ( #15601, #45680, #26954, #4531, #41973, #23262, #19556, #850, #15851, #16577 ),
 .UNSPECIFIED., .F., .F.,
 ( 4, 2, 2, 2, 4 ),
 ( 0.000000000000000000, 0.2500000000000000000, 0.5000000000000000000, 0.7500000000000000000, 1.000000000000000000 ),
 .UNSPECIFIED. ) ;
#5167 = DIRECTION ( 'NONE',  ( -0.000000000000000000, -1.000000000000000000, -0.000000000000000000 ) ) ;
#5168 = ORIENTED_EDGE ( 'NONE', *, *, #40405, .T. ) ;
#5169 = ADVANCED_FACE ( 'NONE', ( #20504 ), #46841, .T. ) ;
#5170 = CARTESIAN_POINT ( 'NONE',  ( -22.63017914794042085, -20.13847084750349836, 69.29701070597593571 ) ) ;
#5171 = FACE_OUTER_BOUND ( 'NONE', #12667, .T. ) ;
#5172 = ORIENTED_EDGE ( 'NONE', *, *, #2601, .F. ) ;
#5173 = DIRECTION ( 'NONE',  ( -2.867370864192053918E-15, -0.4461977533475101065, 0.8949343913984056931 ) ) ;
#5174 = ORIENTED_EDGE ( 'NONE', *, *, #33588, .F. ) ;
#5175 = LINE ( 'NONE', #38656, #11508 ) ;
#5176 = EDGE_CURVE ( 'NONE', #1179, #30092, #29680, .T. ) ;
#5177 = CARTESIAN_POINT ( 'NONE',  ( -10.42411308964128480, -14.77563531838571009, 71.61317379136900740 ) ) ;
#5178 = ORIENTED_EDGE ( 'NONE', *, *, #27558, .T. ) ;
#5179 = DIRECTION ( 'NONE',  ( 0.9687793358424821033, -0.2479245821708678243, 0.000000000000000000 ) ) ;
#5180 = CARTESIAN_POINT ( 'NONE',  ( -18.37786432726835883, -21.79469297182707521, 69.10042588711679912 ) ) ;
#5181 = CARTESIAN_POINT ( 'NONE',  ( -17.04284385650551670, -8.811426318492348031, 52.18089403414751359 ) ) ;
#5182 = ORIENTED_EDGE ( 'NONE', *, *, #48088, .F. ) ;
#5183 = CARTESIAN_POINT ( 'NONE',  ( -24.42668993457695592, -13.99045928592870780, 73.40799407547365263 ) ) ;
#5184 = EDGE_CURVE ( 'NONE', #34569, #545, #27851, .T. ) ;
#5185 = CARTESIAN_POINT ( 'NONE',  ( -14.73368791995220839, -7.861157911666011522, 56.96344736924808672 ) ) ;
#5186 = CARTESIAN_POINT ( 'NONE',  ( -24.86242983737997747, -14.39095285025967286, 66.36788159907001727 ) ) ;
#5187 = ORIENTED_EDGE ( 'NONE', *, *, #31505, .T. ) ;
#5188 = DIRECTION ( 'NONE',  ( 0.9687793358424821033, -0.2479245821708677133, 0.000000000000000000 ) ) ;
#5189 = CARTESIAN_POINT ( 'NONE',  ( -11.38784684563249527, -10.44144024994987774, 74.55229573521346254 ) ) ;
#5190 = CIRCLE ( 'NONE', #26452, 5.249999999999998224 ) ;
#5191 = CARTESIAN_POINT ( 'NONE',  ( -15.32409385541304481, -9.359200813967568422, 50.49621490985804684 ) ) ;
#5192 = CARTESIAN_POINT ( 'NONE',  ( -20.50783493979771421, -8.027295371342848540, 66.96599508560271374 ) ) ;
#5193 = CARTESIAN_POINT ( 'NONE',  ( -12.25434429315920859, -20.17366997322574562, 65.05170215947674706 ) ) ;
#5194 = VERTEX_POINT ( 'NONE', #12374 ) ;
#5195 = ORIENTED_EDGE ( 'NONE', *, *, #40804, .T. ) ;
#5196 = CARTESIAN_POINT ( 'NONE',  ( -24.48824824621826224, -12.44270503963961438, 73.44236770847334128 ) ) ;
#5197 = CARTESIAN_POINT ( 'NONE',  ( -21.65914559189701194, -18.31838547852702348, 53.49999999999995026 ) ) ;
#5198 = VERTEX_POINT ( 'NONE', #16542 ) ;
#5199 = CARTESIAN_POINT ( 'NONE',  ( -24.72409385541305582, -14.80920654474426357, 72.98823529411762934 ) ) ;
#5200 = FACE_OUTER_BOUND ( 'NONE', #2859, .T. ) ;
#5201 = CARTESIAN_POINT ( 'NONE',  ( -21.65534385759799463, -8.623186033802570094, 49.24843789510466507 ) ) ;
#5202 = DIRECTION ( 'NONE',  ( 0.000000000000000000, 0.000000000000000000, 1.000000000000000000 ) ) ;
#5203 = ADVANCED_FACE ( 'NONE', ( #27396 ), #47979, .T. ) ;
#5204 = CARTESIAN_POINT ( 'NONE',  ( -16.80428239998583351, -12.38725820513820253, 54.28066884056654828 ) ) ;
#5205 = CARTESIAN_POINT ( 'NONE',  ( -15.77324217985454347, -8.006205760197399712, 70.89373336146486793 ) ) ;
#5206 = EDGE_CURVE ( 'NONE', #30992, #10658, #33833, .T. ) ;
#5207 = ORIENTED_EDGE ( 'NONE', *, *, #35300, .T. ) ;
#5208 = PRODUCT_DEFINITION_SHAPE ( 'NONE', 'NONE',  #48734 ) ;
#5209 = CARTESIAN_POINT ( 'NONE',  ( -15.59410181515468530, -19.12364873146922051, 49.52966884056656482 ) ) ;
#5210 = ADVANCED_FACE ( 'NONE', ( #5490 ), #16293, .T. ) ;
#5211 = DIRECTION ( 'NONE',  ( 0.9687793358424822143, -0.2479245821708672415, 0.000000000000000000 ) ) ;
#5212 = B_SPLINE_CURVE_WITH_KNOTS ( 'NONE', 3,
 ( #8599, #12993, #38625, #27304, #19921, #35411, #31241, #46517, #5146, #34926 ),
 .UNSPECIFIED., .F., .F.,
 ( 4, 2, 2, 2, 4 ),
 ( 0.6272669072877862240, 0.7522669073072955070, 0.8772669073268049011, 1.002266907346314184, 1.127266907365823467 ),
 .UNSPECIFIED. ) ;
#5213 = CARTESIAN_POINT ( 'NONE',  ( -24.42401643431037073, -14.84212902100172293, 59.54300237020546405 ) ) ;
#5214 = CARTESIAN_POINT ( 'NONE',  ( -19.81321178474628653, -21.38894381613673090, 68.93482470043255717 ) ) ;
#5215 = EDGE_LOOP ( 'NONE', ( #28186, #32722, #30945, #1047, #41429 ) ) ;
#5216 = VERTEX_POINT ( 'NONE', #12855 ) ;
#5217 = ORIENTED_EDGE ( 'NONE', *, *, #48585, .F. ) ;
#5218 = CARTESIAN_POINT ( 'NONE',  ( -11.17855950479832927, -18.87086615690261482, 64.86211796126700335 ) ) ;
#5219 = CARTESIAN_POINT ( 'NONE',  ( -24.07726096719255438, -12.63292432398402454, 69.84531015058388448 ) ) ;
#5220 = ORIENTED_EDGE ( 'NONE', *, *, #31630, .F. ) ;
#5221 = CARTESIAN_POINT ( 'NONE',  ( -10.43414267264621209, -14.42617504702240616, 67.87416736802629202 ) ) ;
#5222 = VECTOR ( 'NONE', #23113, 1000.000000000000000 ) ;
#5223 = CYLINDRICAL_SURFACE ( 'NONE', #30433, 1.249999999999998668 ) ;
#5224 = ORIENTED_EDGE ( 'NONE', *, *, #5938, .T. ) ;
#5225 =( BOUNDED_CURVE ( )  B_SPLINE_CURVE ( 3, ( #36104, #44019, #32194, #39571 ),
 .UNSPECIFIED., .F., .F. ) 
 B_SPLINE_CURVE_WITH_KNOTS ( ( 4, 4 ),
 ( 1.570796326794897002, 1.780235837034217283 ),
 .UNSPECIFIED. ) 
 CURVE ( )  GEOMETRIC_REPRESENTATION_ITEM ( )  RATIONAL_B_SPLINE_CURVE ( ( 1.000000000000000000, 0.9963479302455154896, 0.9963479302455154896, 1.000000000000000000 ) ) 
 REPRESENTATION_ITEM ( '' )  );
#5226 = CARTESIAN_POINT ( 'NONE',  ( -10.47558616449645719, -13.96070292038791294, 57.74824990892705756 ) ) ;
#5227 = ORIENTED_EDGE ( 'NONE', *, *, #10485, .T. ) ;
#5228 = DIRECTION ( 'NONE',  ( 2.168404344971008375E-16, -0.000000000000000000, -1.000000000000000000 ) ) ;
#5229 = ORIENTED_EDGE ( 'NONE', *, *, #47231, .F. ) ;
#5230 = CARTESIAN_POINT ( 'NONE',  ( -14.25068793291388225, -8.513811817964199946, 71.02957628655769895 ) ) ;
#5231 = PLANE ( 'NONE',  #28345 ) ;
#5232 = EDGE_CURVE ( 'NONE', #25942, #12218, #27386, .T. ) ;
#5233 = CARTESIAN_POINT ( 'NONE',  ( -27.42409385541305511, -6.359206544744109735, 63.99999999999998579 ) ) ;
#5234 = ORIENTED_EDGE ( 'NONE', *, *, #44465, .T. ) ;
#5235 = DIRECTION ( 'NONE',  ( 1.000000000000000000, 0.000000000000000000, 0.000000000000000000 ) ) ;
#5236 = CARTESIAN_POINT ( 'NONE',  ( -24.46812100523181144, -14.51191712007779699, 66.19764790277996269 ) ) ;
#5237 = CARTESIAN_POINT ( 'NONE',  ( -15.39389095703113952, -21.97733419268598709, 72.23070866474378704 ) ) ;
#5238 = ADVANCED_FACE ( 'NONE', ( #20740 ), #35980, .T. ) ;
#5239 = DIRECTION ( 'NONE',  ( -0.9687793358424821033, 0.2479245821708679631, 8.466249959240414680E-17 ) ) ;
#5240 = CARTESIAN_POINT ( 'NONE',  ( -20.83411228044830210, -20.98307166581800587, 65.99942768993690834 ) ) ;
#5241 = CARTESIAN_POINT ( 'NONE',  ( -20.60909959404585479, -21.04276736930940572, 58.64475179565906160 ) ) ;
#5242 = ORIENTED_EDGE ( 'NONE', *, *, #17838, .F. ) ;
#5243 = DIRECTION ( 'NONE',  ( -0.8565259173193582320, 0.5161040137028852781, -6.301967848571462020E-08 ) ) ;
#5244 = CARTESIAN_POINT ( 'NONE',  ( -13.49145512112739276, -18.65424914341562967, 53.49999999999995026 ) ) ;
#5245 = CARTESIAN_POINT ( 'NONE',  ( -24.86683893566021908, -14.47670559543334612, 66.32259343128521323 ) ) ;
#5246 = DIRECTION ( 'NONE',  ( 3.549360974554993999E-17, -6.371834667797928663E-18, -1.000000000000000000 ) ) ;
#5247 = CARTESIAN_POINT ( 'NONE',  ( -14.21044241041869682, -21.02792381686613155, 72.11710836390169277 ) ) ;
#5248 = CARTESIAN_POINT ( 'NONE',  ( -17.34909385650551883, -8.104110260919579645, 48.81699501597546487 ) ) ;
#5249 = ORIENTED_EDGE ( 'NONE', *, *, #40239, .F. ) ;
#5250 = CARTESIAN_POINT ( 'NONE',  ( 23.52590614458706852, -0.1092523909521068148, 50.53028072113869484 ) ) ;
#5251 = CARTESIAN_POINT ( 'NONE',  ( -24.26837845117148618, -16.27774503625218827, 59.13834813487091679 ) ) ;
#5252 = ORIENTED_EDGE ( 'NONE', *, *, #31379, .F. ) ;
#5253 = CYLINDRICAL_SURFACE ( 'NONE', #35491, 0.1499999999999994116 ) ;
#5254 = CARTESIAN_POINT ( 'NONE',  ( -14.97500087744905706, -21.84515684796887314, 65.20573060225068218 ) ) ;
#5255 = CARTESIAN_POINT ( 'NONE',  ( -17.90754188454616980, -22.24362682123764401, 62.05348668397390099 ) ) ;
#5256 = CARTESIAN_POINT ( 'NONE',  ( -22.89412281574421471, -9.750308782327882895, 70.12523226502652562 ) ) ;
#5257 = LINE ( 'NONE', #21250, #40848 ) ;
#5258 = ORIENTED_EDGE ( 'NONE', *, *, #12418, .T. ) ;
#5259 = CARTESIAN_POINT ( 'NONE',  ( -24.41485939984550058, -14.44976655980182834, 66.48292729254383460 ) ) ;
#5260 = EDGE_CURVE ( 'NONE', #16415, #40297, #13940, .T. ) ;
#5261 = AXIS2_PLACEMENT_3D ( 'NONE', #26827, #7388, #37892 ) ;
#5262 = CARTESIAN_POINT ( 'NONE',  ( -16.93941734680483080, -7.775588144984237005, 74.24546186738449194 ) ) ;
#5263 = AXIS2_PLACEMENT_3D ( 'NONE', #19439, #12535, #41859 ) ;
#5264 = CARTESIAN_POINT ( 'NONE',  ( -10.09540101917376198, -16.14908387813135349, 68.13801154137269123 ) ) ;
#5265 = EDGE_CURVE ( 'NONE', #46590, #27904, #43800, .T. ) ;
#5266 = EDGE_CURVE ( 'NONE', #32811, #12742, #6902, .T. ) ;
#5267 = ADVANCED_FACE ( 'NONE', ( #36684 ), #28612, .T. ) ;
#5268 = ORIENTED_EDGE ( 'NONE', *, *, #7866, .F. ) ;
#5269 = CARTESIAN_POINT ( 'NONE',  ( -14.97188219925329378, -8.199429090594037461, 56.84999999999994458 ) ) ;
#5270 = VECTOR ( 'NONE', #17881, 1000.000000000000000 ) ;
#5271 = CARTESIAN_POINT ( 'NONE',  ( -23.41977742916776251, -11.19648202114625235, 73.66193302070908544 ) ) ;
#5272 = DIRECTION ( 'NONE',  ( 1.000000000000000000, -4.164305804376849172E-17, 1.614929280266638808E-16 ) ) ;
#5273 = CARTESIAN_POINT ( 'NONE',  ( -10.59656512619885227, -13.05092609425065397, 68.02360230423870746 ) ) ;
#5274 = LINE ( 'NONE', #23506, #30724 ) ;
#5275 = ORIENTED_EDGE ( 'NONE', *, *, #25593, .T. ) ;
#5276 = ORIENTED_EDGE ( 'NONE', *, *, #36050, .F. ) ;
#5277 = CARTESIAN_POINT ( 'NONE',  ( -22.01784385541304090, -6.860780111191487229, 51.02154966934377001 ) ) ;
#5278 = CARTESIAN_POINT ( 'NONE',  ( -24.05059673655033947, -17.06518960458298650, 73.18336032079744768 ) ) ;
#5279 = CARTESIAN_POINT ( 'NONE',  ( -20.11563925035808253, -8.345964739383660458, 73.79266765117813520 ) ) ;
#5280 =( BOUNDED_SURFACE ( )  B_SPLINE_SURFACE ( 3, 1, ( 
 ( #43962, #17091 ),
 ( #36526, #10462 ),
 ( #6760, #43476 ),
 ( #24757, #39759 ),
 ( #113, #15098 ),
 ( #18301, #14837 ),
 ( #48351, #33311 ) ),
 .UNSPECIFIED., .T., .F., .F. ) 
 B_SPLINE_SURFACE_WITH_KNOTS ( ( 4, 3, 4 ),
 ( 2, 2 ),
 ( 0.000000000000000000, 0.5000000000000000000, 1.000000000000000000 ),
 ( 0.000000000000000000, 1.000000000000000000 ),
 .UNSPECIFIED. ) 
 GEOMETRIC_REPRESENTATION_ITEM ( )  RATIONAL_B_SPLINE_SURFACE ( (
 ( 1.000000000000000000, 1.000000000000000000),
 ( 0.3333333333333335369, 0.3333333333333330373),
 ( 0.3333333333333335369, 0.3333333333333330373),
 ( 1.000000000000000000, 1.000000000000000000),
 ( 0.3333333333333333703, 0.3333333333333333703),
 ( 0.3333333333333333703, 0.3333333333333333703),
 ( 1.000000000000000000, 1.000000000000000000) ) ) 
 REPRESENTATION_ITEM ( '' )  SURFACE ( )  );
#5281 = CARTESIAN_POINT ( 'NONE',  ( -17.36015840614627592, -7.359395087992972151, 67.20535029649403214 ) ) ;
#5282 = ADVANCED_FACE ( 'NONE', ( #9902 ), #17511, .T. ) ;
#5283 = CARTESIAN_POINT ( 'NONE',  ( -24.33592553122863578, -17.58935301986056032, 66.14346027011359297 ) ) ;
#5284 = CARTESIAN_POINT ( 'NONE',  ( -20.12289122552838094, -7.865124802246414859, 73.90591932823114973 ) ) ;
#5285 = LINE ( 'NONE', #17066, #13109 ) ;
#5286 = EDGE_LOOP ( 'NONE', ( #11314, #27625, #24910, #40535, #19946 ) ) ;
#5287 = CARTESIAN_POINT ( 'NONE',  ( -21.89826351590202336, -8.852228842849337198, 66.84645279485334868 ) ) ;
#5288 =( BOUNDED_CURVE ( )  B_SPLINE_CURVE ( 3, ( #35122, #8315, #12725, #447 ),
 .UNSPECIFIED., .F., .F. ) 
 B_SPLINE_CURVE_WITH_KNOTS ( ( 4, 4 ),
 ( 0.5000000000000000000, 0.9074455897393635118 ),
 .UNSPECIFIED. ) 
 CURVE ( )  GEOMETRIC_REPRESENTATION_ITEM ( )  RATIONAL_B_SPLINE_CURVE ( ( 0.9999999999999961142, 0.4567392136813367420, 0.3561768502900346522, 0.6983129098260856260 ) ) 
 REPRESENTATION_ITEM ( '' )  );
#5289 = CARTESIAN_POINT ( 'NONE',  ( -17.14068154504527186, -7.813665858854684565, 74.03188528864532714 ) ) ;
#5290 = CIRCLE ( 'NONE', #11571, 1.999999999999999556 ) ;
#5291 = AXIS2_PLACEMENT_3D ( 'NONE', #16464, #16215, #8866 ) ;
#5292 = ORIENTED_EDGE ( 'NONE', *, *, #8679, .T. ) ;
#5293 = CARTESIAN_POINT ( 'NONE',  ( -10.76802635004704989, -17.14192985119425572, 57.57271792098855201 ) ) ;
#5294 = ORIENTED_EDGE ( 'NONE', *, *, #23814, .T. ) ;
#5295 = CARTESIAN_POINT ( 'NONE',  ( -10.51728758832436661, -13.39531270954807063, 74.97817630058322891 ) ) ;
#5296 = CARTESIAN_POINT ( 'NONE',  ( -10.49189908542464522, -16.09426454567519116, 68.26295692486267797 ) ) ;
#5297 = EDGE_CURVE ( 'NONE', #12385, #24381, #22064, .T. ) ;
#5298 = CIRCLE ( 'NONE', #29651, 0.6570903894995150374 ) ;
#5299 = CARTESIAN_POINT ( 'NONE',  ( -13.60236376389480384, -20.73382277062339085, 61.80174179654961364 ) ) ;
#5300 = CARTESIAN_POINT ( 'NONE',  ( -19.32571124525177098, -8.020471753322730990, 59.96093016115477070 ) ) ;
#5301 = VERTEX_POINT ( 'NONE', #2971 ) ;
#5302 = CARTESIAN_POINT ( 'NONE',  ( -24.10489316104180801, -11.51232611631470348, 63.10218278254900781 ) ) ;
#5303 = CARTESIAN_POINT ( 'NONE',  ( -10.96693745925601959, -17.63935232738105796, 71.57277952047664371 ) ) ;
#5304 = CARTESIAN_POINT ( 'NONE',  ( -24.57916482434842820, -12.73107666121563142, 69.95898344571149607 ) ) ;
#5305 = CARTESIAN_POINT ( 'NONE',  ( -19.86569447268030686, -19.73755174630646536, 54.07175714974878389 ) ) ;
#5306 = CONTEXT_DEPENDENT_SHAPE_REPRESENTATION ( #36577, #19744 ) ;
#5307 = B_SPLINE_CURVE_WITH_KNOTS ( 'NONE', 1,
 ( #22097, #13712 ),
 .UNSPECIFIED., .F., .F.,
 ( 2, 2 ),
 ( 0.000000000000000000, 1.000000000000000000 ),
 .UNSPECIFIED. ) ;
#5308 = CARTESIAN_POINT ( 'NONE',  ( -11.43673139740920597, -18.43582035383210993, 57.88002590065035946 ) ) ;
#5309 = DIRECTION ( 'NONE',  ( -3.071710424422018668E-17, 6.404604876783312462E-16, 1.000000000000000000 ) ) ;
#5310 = CARTESIAN_POINT ( 'NONE',  ( -22.84886471163500588, -9.702775354051940582, 73.59665661135821324 ) ) ;
#5311 = VERTEX_POINT ( 'NONE', #28844 ) ;
#5312 = CARTESIAN_POINT ( 'NONE',  ( -23.64630840998975359, -11.48693468987944577, 63.16038249791161263 ) ) ;
#5313 = ORIENTED_EDGE ( 'NONE', *, *, #32512, .F. ) ;
#5314 = CARTESIAN_POINT ( 'NONE',  ( -21.34121592312026650, -8.943118034117361503, 70.13132274644620168 ) ) ;
#5315 = DIRECTION ( 'NONE',  ( 1.000000000000000000, 0.000000000000000000, 8.260587980841940012E-17 ) ) ;
#5316 = ORIENTED_EDGE ( 'NONE', *, *, #11805, .T. ) ;
#5317 = CARTESIAN_POINT ( 'NONE',  ( -24.37683887807358474, -15.97618392648307584, 66.36324926629207255 ) ) ;
#5318 = FACE_BOUND ( 'NONE', #48512, .T. ) ;
#5319 = ORIENTED_EDGE ( 'NONE', *, *, #3210, .T. ) ;
#5320 = ADVANCED_FACE ( 'NONE', ( #35736 ), #25162, .F. ) ;
#5321 = EDGE_CURVE ( 'NONE', #1571, #25382, #34961, .T. ) ;
#5322 = ORIENTED_EDGE ( 'NONE', *, *, #29235, .T. ) ;
#5323 = ORIENTED_EDGE ( 'NONE', *, *, #37392, .T. ) ;
#5324 = CARTESIAN_POINT ( 'NONE',  ( -17.85728874018075985, -21.84618329174708151, 61.89007996730683203 ) ) ;
#5325 = DIRECTION ( 'NONE',  ( 1.000000000000000000, -0.000000000000000000, -2.406186529621654511E-16 ) ) ;
#5326 = CARTESIAN_POINT ( 'NONE',  ( -11.53247046633659423, -18.68106308600668441, 64.74707076449911369 ) ) ;
#5327 = CARTESIAN_POINT ( 'NONE',  ( -12.57344175313163781, -19.85833261874117284, 68.44730439049486392 ) ) ;
#5328 = CARTESIAN_POINT ( 'NONE',  ( -14.72778380697628187, -21.32322314059345558, 58.16617885012795597 ) ) ;
#5329 =( GEOMETRIC_REPRESENTATION_CONTEXT ( 3 ) GLOBAL_UNCERTAINTY_ASSIGNED_CONTEXT ( ( #9070 ) ) GLOBAL_UNIT_ASSIGNED_CONTEXT ( ( #22723, #41915, #30847 ) ) REPRESENTATION_CONTEXT ( 'NONE', 'WORKASPACE' ) );
#5330 = AXIS2_PLACEMENT_3D ( 'NONE', #2902, #14214, #43332 ) ;
#5331 = ORIENTED_EDGE ( 'NONE', *, *, #10422, .T. ) ;
#5332 = EDGE_LOOP ( 'NONE', ( #8379, #14604, #44261, #14559 ) ) ;
#5333 = EDGE_CURVE ( 'NONE', #46610, #32982, #44139, .T. ) ;
#5334 = EDGE_CURVE ( 'NONE', #15747, #39502, #42666, .T. ) ;
#5335 = CARTESIAN_POINT ( 'NONE',  ( -20.53034385650551386, -9.794322478646142471, 51.19202720610083901 ) ) ;
#5336 = EDGE_CURVE ( 'NONE', #10683, #26257, #4546, .T. ) ;
#5337 = FACE_OUTER_BOUND ( 'NONE', #20791, .T. ) ;
#5338 = DIRECTION ( 'NONE',  ( -0.9180681052388980357, 0.3964226963016364014, 0.000000000000000000 ) ) ;
#5339 = AXIS2_PLACEMENT_3D ( 'NONE', #33672, #29514, #3411 ) ;
#5340 = CARTESIAN_POINT ( 'NONE',  ( -22.89284385650552522, -7.406986770994973490, 48.81910596585309747 ) ) ;
#5341 = CIRCLE ( 'NONE', #621, 1.999999999999999556 ) ;
#5342 = VERTEX_POINT ( 'NONE', #24916 ) ;
#5343 = B_SPLINE_CURVE_WITH_KNOTS ( 'NONE', 1,
 ( #10336, #40362 ),
 .UNSPECIFIED., .F., .F.,
 ( 2, 2 ),
 ( 0.000000000000000000, 1.000000000000000000 ),
 .UNSPECIFIED. ) ;
#5344 = DIRECTION ( 'NONE',  ( -5.731567514496413899E-31, -1.020425574103664789E-16, -1.000000000000000000 ) ) ;
#5345 = EDGE_CURVE ( 'NONE', #18572, #24808, #48042, .T. ) ;
#5346 = CYLINDRICAL_SURFACE ( 'NONE', #41841, 2.499999999999999112 ) ;
#5347 = CARTESIAN_POINT ( 'NONE',  ( -12.54253442593986456, -19.82621537833410841, 64.86674886820043184 ) ) ;
#5348 = VERTEX_POINT ( 'NONE', #10140 ) ;
#5349 = DIRECTION ( 'NONE',  ( 0.9774082387306983755, -0.2113602016968848529, 7.903122840289807171E-08 ) ) ;
#5350 = CARTESIAN_POINT ( 'NONE',  ( -22.57893663749957369, -9.999394138389963160, 73.49633153340955971 ) ) ;
#5351 = CARTESIAN_POINT ( 'NONE',  ( -22.10214723240122225, -9.011059706093044852, 63.29179509575568119 ) ) ;
#5352 = CARTESIAN_POINT ( 'NONE',  ( -19.12163971562669218, -7.963538243666484107, 67.31560661829935555 ) ) ;
#5353 = VERTEX_POINT ( 'NONE', #32999 ) ;
#5354 = AXIS2_PLACEMENT_3D ( 'NONE', #36680, #10614, #17979 ) ;
#5355 = CARTESIAN_POINT ( 'NONE',  ( -11.77169535943213319, -10.59578862612641714, 74.73885051658086809 ) ) ;
#5356 = DIRECTION ( 'NONE',  ( -0.000000000000000000, -1.000000000000000000, -0.000000000000000000 ) ) ;
#5357 = CARTESIAN_POINT ( 'NONE',  ( -11.38992678570165396, -18.36044987817664875, 61.38784012437933768 ) ) ;
#5358 = EDGE_LOOP ( 'NONE', ( #3347, #22271, #271, #46767 ) ) ;
#5359 = DIRECTION ( 'NONE',  ( 0.000000000000000000, 0.000000000000000000, -1.000000000000000000 ) ) ;
#5360 = VECTOR ( 'NONE', #38478, 1000.000000000000000 ) ;
#5361 = VECTOR ( 'NONE', #37421, 999.9999999999998863 ) ;
#5362 = ORIENTED_EDGE ( 'NONE', *, *, #44509, .T. ) ;
#5363 = CARTESIAN_POINT ( 'NONE',  ( -15.80034074178659331, -19.80179363221599687, 49.52966884056656482 ) ) ;
#5364 = CARTESIAN_POINT ( 'NONE',  ( -14.67111564601650997, -7.886426081561471513, 60.43500846974642116 ) ) ;
#5365 = EDGE_LOOP ( 'NONE', ( #44682, #15278 ) ) ;
#5366 = LINE ( 'NONE', #5124, #18733 ) ;
#5367 = DIRECTION ( 'NONE',  ( 0.9986807914369957295, -0.05134858142905001505, 1.286972170232539807E-09 ) ) ;
#5368 = CARTESIAN_POINT ( 'NONE',  ( -13.71586683582447819, -8.803873544643577631, 60.58383457371648717 ) ) ;
#5369 = CARTESIAN_POINT ( 'NONE',  ( -26.66312147401635713, -19.64855152110175140, 54.58422952202462142 ) ) ;
#5370 = ORIENTED_EDGE ( 'NONE', *, *, #36392, .T. ) ;
#5371 = DIRECTION ( 'NONE',  ( -5.731567514496413899E-31, -1.020425574103664789E-16, -1.000000000000000000 ) ) ;
#5372 = VECTOR ( 'NONE', #24458, 1000.000000000000000 ) ;
#5373 = LINE ( 'NONE', #43287, #41562 ) ;
#5374 = ADVANCED_FACE ( 'NONE', ( #39929 ), #32540, .T. ) ;
#5375 = CARTESIAN_POINT ( 'NONE',  ( -10.49189908542464700, -16.09426454567519116, 68.26295692486267797 ) ) ;
#5376 = ORIENTED_EDGE ( 'NONE', *, *, #45361, .T. ) ;
#5377 = B_SPLINE_CURVE_WITH_KNOTS ( 'NONE', 3,
 ( #30077, #46302, #1225, #42850, #47017, #23409, #15994, #12315, #13261, #23900 ),
 .UNSPECIFIED., .F., .F.,
 ( 4, 2, 2, 2, 4 ),
 ( 0.1272669073657988481, 0.2522669073439235410, 0.3772669073220482616, 0.5022669073001729823, 0.6272669072782977029 ),
 .UNSPECIFIED. ) ;
#5378 = CARTESIAN_POINT ( 'NONE',  ( -15.81235419205221859, -7.945607373518419614, 67.42535135806457447 ) ) ;
#5379 = CARTESIAN_POINT ( 'NONE',  ( -24.72417498505505051, -16.29709994844161969, 62.73295351231081440 ) ) ;
#5380 = EDGE_CURVE ( 'NONE', #32441, #17998, #4271, .T. ) ;
#5381 = ORIENTED_EDGE ( 'NONE', *, *, #40240, .F. ) ;
#5382 = ORIENTED_EDGE ( 'NONE', *, *, #13750, .T. ) ;
#5383 = CARTESIAN_POINT ( 'NONE',  ( -24.45601047785835647, -15.36200925639139037, 73.21123547652044294 ) ) ;
#5384 = LINE ( 'NONE', #24338, #13975 ) ;
#5385 = CARTESIAN_POINT ( 'NONE',  ( -10.42619868690400153, -14.62054347036657909, 71.34399284208600989 ) ) ;
#5386 = CARTESIAN_POINT ( 'NONE',  ( -19.76784385650551812, -6.428312510596451368, 51.20221977374900035 ) ) ;
#5387 = CARTESIAN_POINT ( 'NONE',  ( -11.75188473902813335, -10.61641672623718158, 71.17712947513925315 ) ) ;
#5388 = CARTESIAN_POINT ( 'NONE',  ( -4.424093855413053333, -6.859206544744110623, 63.99999999999998579 ) ) ;
#5389 = CARTESIAN_POINT ( 'NONE',  ( -12.19762647230555075, -20.11848340473563468, 64.98957966092764593 ) ) ;
#5390 = CARTESIAN_POINT ( 'NONE',  ( -13.87335526996593948, -21.35862697870957660, 72.02584070344211398 ) ) ;
#5391 = ORIENTED_EDGE ( 'NONE', *, *, #48107, .F. ) ;
#5392 = ORIENTED_EDGE ( 'NONE', *, *, #18547, .T. ) ;
#5393 = ADVANCED_FACE ( 'NONE', ( #39870 ), #9312, .T. ) ;
#5394 = EDGE_CURVE ( 'NONE', #38583, #40137, #31492, .T. ) ;
#5395 = LINE ( 'NONE', #1697, #4761 ) ;
#5396 = CARTESIAN_POINT ( 'NONE',  ( -24.07704370891654122, -17.14264987453632827, 72.89808101046213551 ) ) ;
#5397 = LINE ( 'NONE', #28289, #12657 ) ;
#5398 = EDGE_CURVE ( 'NONE', #45248, #39530, #12753, .T. ) ;
#5399 = AXIS2_PLACEMENT_3D ( 'NONE', #34988, #23201, #22966 ) ;
#5400 = AXIS2_PLACEMENT_3D ( 'NONE', #40482, #21309, #10226 ) ;
#5401 = CIRCLE ( 'NONE', #10106, 1.250000000000001110 ) ;
#5402 = ORIENTED_EDGE ( 'NONE', *, *, #13893, .F. ) ;
#5403 = DIRECTION ( 'NONE',  ( -3.071710424422018668E-17, 6.404604876783312462E-16, 1.000000000000000000 ) ) ;
#5404 = CARTESIAN_POINT ( 'NONE',  ( -10.20197030601470090, -12.78660143320473175, 54.27966884056655061 ) ) ;
#5405 = CARTESIAN_POINT ( 'NONE',  ( -19.09948850906665285, -8.012659424734943414, 63.73089235424028942 ) ) ;
#5406 = CARTESIAN_POINT ( 'NONE',  ( -10.51729421260818320, -16.22293138110306643, 71.44750383217574097 ) ) ;
#5407 = CIRCLE ( 'NONE', #15609, 2.000000000000001776 ) ;
#5408 = EDGE_CURVE ( 'NONE', #38712, #28574, #11516, .T. ) ;
#5409 = ORIENTED_EDGE ( 'NONE', *, *, #35700, .T. ) ;
#5410 = CARTESIAN_POINT ( 'NONE',  ( -15.87557486115803052, -7.931373420853708112, 67.44007279014866185 ) ) ;
#5411 = CARTESIAN_POINT ( 'NONE',  ( -24.43499015649444317, -15.57872826220114781, 69.41818628325123086 ) ) ;
#5412 =( LENGTH_UNIT ( ) NAMED_UNIT ( * ) SI_UNIT ( .MILLI., .METRE. ) );
#5413 = CARTESIAN_POINT ( 'NONE',  ( -22.84886471163500588, -9.702775354051940582, 73.59665661135821324 ) ) ;
#5414 =( BOUNDED_CURVE ( )  B_SPLINE_CURVE ( 3, ( #11501, #11753, #26777, #41796 ),
 .UNSPECIFIED., .F., .F. ) 
 B_SPLINE_CURVE_WITH_KNOTS ( ( 4, 4 ),
 ( 4.712388980384690562, 4.921828490624004182 ),
 .UNSPECIFIED. ) 
 CURVE ( )  GEOMETRIC_REPRESENTATION_ITEM ( )  RATIONAL_B_SPLINE_CURVE ( ( 1.000000000000000000, 0.9963479302455156006, 0.9963479302455156006, 1.000000000000000000 ) ) 
 REPRESENTATION_ITEM ( '' )  );
#5415 = CARTESIAN_POINT ( 'NONE',  ( -22.61159385759798823, -8.990409506049200417, 49.61344411288074951 ) ) ;
#5416 = ORIENTED_EDGE ( 'NONE', *, *, #34630, .F. ) ;
#5417 = CARTESIAN_POINT ( 'NONE',  ( -21.63336539757928634, -9.153348366551478321, 66.94677872351418557 ) ) ;
#5418 = ORIENTED_EDGE ( 'NONE', *, *, #41499, .T. ) ;
#5419 = CARTESIAN_POINT ( 'NONE',  ( -10.00731240618708462, -14.10555136595099945, 61.10316694600977172 ) ) ;
#5420 = LINE ( 'NONE', #20441, #20327 ) ;
#5421 = VERTEX_POINT ( 'NONE', #14958 ) ;
#5422 = CARTESIAN_POINT ( 'NONE',  ( -24.84240844029834250, -14.11474841844398043, 69.76619977786306492 ) ) ;
#5423 = DIRECTION ( 'NONE',  ( -0.5022914217388750879, 0.8646984027090224290, 6.766381827299039861E-08 ) ) ;
#5424 = CARTESIAN_POINT ( 'NONE',  ( -18.89909385650551599, -8.114302828567740988, 52.18300498402516041 ) ) ;
#5425 = AXIS2_PLACEMENT_3D ( 'NONE', #36, #14513, #44605 ) ;
#5426 = ORIENTED_EDGE ( 'NONE', *, *, #3472, .F. ) ;
#5427 = CARTESIAN_POINT ( 'NONE',  ( -15.26209398273251772, -21.93938324809698770, 68.68937616499954402 ) ) ;
#5428 = AXIS2_PLACEMENT_3D ( 'NONE', #8855, #35170, #46271 ) ;
#5429 = EDGE_CURVE ( 'NONE', #3502, #44359, #30895, .T. ) ;
#5430 = CARTESIAN_POINT ( 'NONE',  ( -10.65158109870909442, -11.70468408355161216, 74.71986640429058468 ) ) ;
#5431 =( BOUNDED_CURVE ( )  B_SPLINE_CURVE ( 3, ( #12434, #5300, #20316, #631 ),
 .UNSPECIFIED., .F., .F. ) 
 B_SPLINE_CURVE_WITH_KNOTS ( ( 4, 4 ),
 ( 0.4074455897393606252, 0.5000000000000000000 ),
 .UNSPECIFIED. ) 
 CURVE ( )  GEOMETRIC_REPRESENTATION_ITEM ( )  RATIONAL_B_SPLINE_CURVE ( ( 0.6983129098260884016, 0.7760317562607006447, 0.8765941196520063983, 1.000000000000010214 ) ) 
 REPRESENTATION_ITEM ( '' )  );
#5432 = CARTESIAN_POINT ( 'NONE',  ( -16.22845603143158755, -22.16339683637704638, 61.94223519165076652 ) ) ;
#5433 = ORIENTED_EDGE ( 'NONE', *, *, #3052, .F. ) ;
#5435 = FACE_OUTER_BOUND ( 'NONE', #8403, .T. ) ;
#5434 =( BOUNDED_CURVE ( )  B_SPLINE_CURVE ( 3, ( #12658, #15607, #34571, #38511 ),
 .UNSPECIFIED., .F., .F. ) 
 B_SPLINE_CURVE_WITH_KNOTS ( ( 4, 4 ),
 ( 0.4074455897393636228, 0.5000000000000000000 ),
 .UNSPECIFIED. ) 
 CURVE ( )  GEOMETRIC_REPRESENTATION_ITEM ( )  RATIONAL_B_SPLINE_CURVE ( ( 0.6983129098260854040, 0.7760317562606773301, 0.8765941196519780876, 0.9999999999999773515 ) ) 
 REPRESENTATION_ITEM ( '' )  );
#5436 = CIRCLE ( 'NONE', #23507, 5.249999999999998224 ) ;
#5437 = PLANE ( 'NONE',  #11763 ) ;
#5438 = FACE_OUTER_BOUND ( 'NONE', #22345, .T. ) ;
#5439 = B_SPLINE_CURVE_WITH_KNOTS ( 'NONE', 3,
 ( #34109, #44732, #3588, #14635, #30204, #29952, #37301, #18596, #37549, #44987 ),
 .UNSPECIFIED., .F., .F.,
 ( 4, 2, 2, 2, 4 ),
 ( 0.6272669072783160216, 0.7522669073002095086, 0.8772669073221031066, 1.002266907343996483, 1.127266907365890081 ),
 .UNSPECIFIED. ) ;
#5440 = CARTESIAN_POINT ( 'NONE',  ( -17.42409385541299471, -14.80920654474435594, 52.02966884056656482 ) ) ;
#5441 = CARTESIAN_POINT ( 'NONE',  ( -17.42409385541299471, -14.80920654474434883, 62.02966884056656482 ) ) ;
#5442 = ORIENTED_EDGE ( 'NONE', *, *, #39587, .T. ) ;
#5443 = VERTEX_POINT ( 'NONE', #18176 ) ;
#5444 = DIRECTION ( 'NONE',  ( -3.071710424422018668E-17, 6.404604876783312462E-16, 1.000000000000000000 ) ) ;
#5445 = ORIENTED_EDGE ( 'NONE', *, *, #29619, .F. ) ;
#5446 = CARTESIAN_POINT ( 'NONE',  ( -15.81235419205221859, -7.945607373518419614, 67.42535135806457447 ) ) ;
#5447 = DIRECTION ( 'NONE',  ( -3.071710424422018668E-17, 6.404604876783312462E-16, 1.000000000000000000 ) ) ;
#5448 = VECTOR ( 'NONE', #24917, 1000.000000000000000 ) ;
#5449 = CARTESIAN_POINT ( 'NONE',  ( -18.61784385759799321, -6.860780111191487229, 51.02154966934377001 ) ) ;
#5450 = CARTESIAN_POINT ( 'NONE',  ( -23.79929752752725847, -10.95441614946243725, 73.56182072376812187 ) ) ;
#5451 = DIRECTION ( 'NONE',  ( -3.071710424422018668E-17, 6.404604876783312462E-16, 1.000000000000000000 ) ) ;
#5452 = CARTESIAN_POINT ( 'NONE',  ( -10.72552546848295485, -12.61109793159036485, 61.09853568372136579 ) ) ;
#5453 =( BOUNDED_CURVE ( )  B_SPLINE_CURVE ( 3, ( #3651, #32939, #33419, #45048 ),
 .UNSPECIFIED., .F., .F. ) 
 B_SPLINE_CURVE_WITH_KNOTS ( ( 4, 4 ),
 ( 0.000000000000000000, 0.4074455897393692849 ),
 .UNSPECIFIED. ) 
 CURVE ( )  GEOMETRIC_REPRESENTATION_ITEM ( )  RATIONAL_B_SPLINE_CURVE ( ( 1.000000000000000000, 0.4567392136813255288, 0.3561768502900278799, 0.6983129098261070533 ) ) 
 REPRESENTATION_ITEM ( '' )  );
#5454 = ORIENTED_EDGE ( 'NONE', *, *, #46523, .F. ) ;
#5455 = CARTESIAN_POINT ( 'NONE',  ( -22.79734409636068904, -10.24514240368273477, 66.54182257473807738 ) ) ;
#5456 = CARTESIAN_POINT ( 'NONE',  ( -14.84927081153347039, -21.37251255130113137, 61.65072491673618771 ) ) ;
#5457 = EDGE_CURVE ( 'NONE', #17138, #7495, #37619, .T. ) ;
#5458 = CARTESIAN_POINT ( 'NONE',  ( -23.25657551529890554, -10.17392617991681192, 63.32831932546986309 ) ) ;
#5459 = FACE_OUTER_BOUND ( 'NONE', #2481, .T. ) ;
#5460 = EDGE_CURVE ( 'NONE', #28748, #27648, #27565, .T. ) ;
#5461 = VERTEX_POINT ( 'NONE', #14456 ) ;
#5462 = ORIENTED_EDGE ( 'NONE', *, *, #19094, .F. ) ;
#5463 = EDGE_CURVE ( 'NONE', #8478, #30371, #20276, .T. ) ;
#5464 = VERTEX_POINT ( 'NONE', #30268 ) ;
#5465 = CYLINDRICAL_SURFACE ( 'NONE', #28026, 4.686499999999997002 ) ;
#5466 = AXIS2_PLACEMENT_3D ( 'NONE', #44499, #24811, #25525 ) ;
#5467 = DIRECTION ( 'NONE',  ( -0.9180681052388980357, 0.3964226963016366789, 0.000000000000000000 ) ) ;
#5468 = EDGE_CURVE ( 'NONE', #1538, #20590, #29134, .T. ) ;
#5469 = ORIENTED_EDGE ( 'NONE', *, *, #40024, .F. ) ;
#5470 = EDGE_CURVE ( 'NONE', #23831, #34081, #41328, .T. ) ;
#5471 = CIRCLE ( 'NONE', #40847, 2.000000000000001776 ) ;
#5472 = CIRCLE ( 'NONE', #32952, 1.250000000000001110 ) ;
#5473 = CARTESIAN_POINT ( 'NONE',  ( -10.83219059380440541, -11.33772365494832535, 67.74147721111465614 ) ) ;
#5474 = CARTESIAN_POINT ( 'NONE',  ( -10.79572390357762046, -11.40795830647630282, 67.80360014157953685 ) ) ;
#5475 = VERTEX_POINT ( 'NONE', #26077 ) ;
#5476 = CARTESIAN_POINT ( 'NONE',  ( -11.15651104234136781, -18.05456883900698983, 57.95147637344698666 ) ) ;
#5477 = LINE ( 'NONE', #43134, #24203 ) ;
#5478 = ORIENTED_EDGE ( 'NONE', *, *, #46226, .T. ) ;
#5479 = CARTESIAN_POINT ( 'NONE',  ( -11.34160916837339883, -11.34373242234389778, 64.43265517655409269 ) ) ;
#5480 = VERTEX_POINT ( 'NONE', #41088 ) ;
#5481 = CARTESIAN_POINT ( 'NONE',  ( -10.12802834128535245, -13.30252786720044078, 74.77794016282906853 ) ) ;
#5482 = ORIENTED_EDGE ( 'NONE', *, *, #9948, .T. ) ;
#5483 = DIRECTION ( 'NONE',  ( 0.9687793358424821033, -0.2479245821708677133, 0.000000000000000000 ) ) ;
#5484 = CARTESIAN_POINT ( 'NONE',  ( -12.98761351705371503, -9.325367763573320090, 74.61923228824977627 ) ) ;
#5485 = CYLINDRICAL_SURFACE ( 'NONE', #20294, 0.1500000000000032696 ) ;
#5486 = ORIENTED_EDGE ( 'NONE', *, *, #8390, .T. ) ;
#5487 = DIRECTION ( 'NONE',  ( 1.224646799147353207E-16, 1.000000000000000000, -1.912410701131276611E-32 ) ) ;
#5488 = CARTESIAN_POINT ( 'NONE',  ( -10.37795889460693033, -14.56696403379599225, 68.14328054657653411 ) ) ;
#5489 = APPLICATION_CONTEXT ( 'automotive_design' ) ;
#5490 = FACE_OUTER_BOUND ( 'NONE', #47453, .T. ) ;
#5491 = EDGE_CURVE ( 'NONE', #42196, #38954, #26559, .T. ) ;
#5492 = CARTESIAN_POINT ( 'NONE',  ( -11.19706266256277694, -11.50303319689152737, 67.63336710488009373 ) ) ;
#5493 = FACE_OUTER_BOUND ( 'NONE', #27867, .T. ) ;
#5494 = CARTESIAN_POINT ( 'NONE',  ( -19.28939461086542906, -8.062307027802660286, 60.26092997386343342 ) ) ;
#5495 = ORIENTED_EDGE ( 'NONE', *, *, #21366, .T. ) ;
#5496 = CARTESIAN_POINT ( 'NONE',  ( -17.44246871614987526, -7.809230653018538248, 63.65943123996323294 ) ) ;
#5497 = CARTESIAN_POINT ( 'NONE',  ( -17.01195873393923463, -21.85086728866913219, 68.69560488337936022 ) ) ;
#5498 = DIRECTION ( 'NONE',  ( -1.061592179903616477E-06, -3.103086884670442514E-06, 0.9999999999946218576 ) ) ;
#5499 = CARTESIAN_POINT ( 'NONE',  ( -15.18731133007365663, -21.91554468673477629, 68.68254614095756949 ) ) ;
#5500 = CARTESIAN_POINT ( 'NONE',  ( -18.19389434033494268, -22.21941471489327569, 65.53027570717884487 ) ) ;
#5501 = CARTESIAN_POINT ( 'NONE',  ( -15.66159385650551705, -9.295667164867525756, 49.30633214617472504 ) ) ;
#5502 = ORIENTED_EDGE ( 'NONE', *, *, #46653, .T. ) ;
#5503 = CARTESIAN_POINT ( 'NONE',  ( -16.89278889608604572, -7.297489456700872346, 53.60585781316035536 ) ) ;
#5504 = EDGE_LOOP ( 'NONE', ( #32077, #46966, #14256, #11104 ) ) ;
#5505 = DIRECTION ( 'NONE',  ( 0.000000000000000000, -0.9999954153791273948, -0.003028072113822395228 ) ) ;
#5506 = DIRECTION ( 'NONE',  ( 0.9687793358424819923, -0.2479245821708680464, 0.000000000000000000 ) ) ;
#5507 = CARTESIAN_POINT ( 'NONE',  ( -23.17061082369141900, -10.06671700699632233, 66.72837583070179335 ) ) ;
#5508 = CARTESIAN_POINT ( 'NONE',  ( -18.69909385541303948, -8.105421454601382081, 49.25000573077639388 ) ) ;
#5509 = CARTESIAN_POINT ( 'NONE',  ( -10.76785811675246940, -12.48515291162924434, 57.61385273545094066 ) ) ;
#5510 = ORIENTED_EDGE ( 'NONE', *, *, #41529, .F. ) ;
#5511 = EDGE_CURVE ( 'NONE', #29328, #43190, #48715, .T. ) ;
#5512 = CARTESIAN_POINT ( 'NONE',  ( -12.09832633641969402, -9.599544124683230706, 57.26652452003035876 ) ) ;
#5513 = AXIS2_PLACEMENT_3D ( 'NONE', #28993, #2411, #43548 ) ;
#5514 = FACE_OUTER_BOUND ( 'NONE', #30377, .T. ) ;
#5515 = ORIENTED_EDGE ( 'NONE', *, *, #2181, .T. ) ;
#5516 = CARTESIAN_POINT ( 'NONE',  ( -12.81830071990639475, -20.15163239091832992, 68.33657451194982002 ) ) ;
#5517 = VECTOR ( 'NONE', #15046, 1000.000000000000000 ) ;
#5518 = CARTESIAN_POINT ( 'NONE',  ( -23.44004635400542114, -11.23012040261692590, 73.36193342793328043 ) ) ;
#5519 = CARTESIAN_POINT ( 'NONE',  ( -24.53780051168580911, -12.59584816521350348, 69.95738404390658616 ) ) ;
#5520 = B_SPLINE_CURVE_WITH_KNOTS ( 'NONE', 3,
 ( #20454, #46317, #34968, #20932, #31281, #24392, #32012, #12571, #38912, #27831 ),
 .UNSPECIFIED., .F., .F.,
 ( 4, 2, 2, 2, 4 ),
 ( 0.6272669072877306018, 0.7522669073072547619, 0.8772669073267790329, 1.002266907346303304, 1.127266907365827464 ),
 .UNSPECIFIED. ) ;
#5521 = LINE ( 'NONE', #27188, #42522 ) ;
#5522 = DIRECTION ( 'NONE',  ( -2.866981220435666553E-17, 1.000000000000000000, 1.190614954331866791E-16 ) ) ;
#5523 = EDGE_LOOP ( 'NONE', ( #45948, #47271, #14932, #671 ) ) ;
#5524 = ORIENTED_EDGE ( 'NONE', *, *, #19039, .F. ) ;
#5525 = CARTESIAN_POINT ( 'NONE',  ( -22.07409385541304303, -6.859212275519751323, 50.50378509014259265 ) ) ;
#5526 = ADVANCED_FACE ( 'NONE', ( #11298 ), #3918, .T. ) ;
#5527 = CARTESIAN_POINT ( 'NONE',  ( -13.19836015843563182, -9.228522675521540819, 64.13619768069759175 ) ) ;
#5528 = VECTOR ( 'NONE', #32490, 1000.000000000000000 ) ;
#5529 = ADVANCED_FACE ( 'NONE', ( #40583 ), #42563, .F. ) ;
#5530 = CARTESIAN_POINT ( 'NONE',  ( -15.41904641700715217, -7.634001813009263060, 74.19490365927923392 ) ) ;
#5531 = EDGE_CURVE ( 'NONE', #17249, #46845, #46760, .T. ) ;
#5532 = CARTESIAN_POINT ( 'NONE',  ( -11.64339224431418529, -10.10844562305556771, 71.15548443915361077 ) ) ;
#5533 = CARTESIAN_POINT ( 'NONE',  ( -22.97879330524300912, -10.54927326435941026, 59.90203382372271790 ) ) ;
#5534 = FACE_OUTER_BOUND ( 'NONE', #11489, .T. ) ;
#5535 = VERTEX_POINT ( 'NONE', #27523 ) ;
#5536 = AXIS2_PLACEMENT_3D ( 'NONE', #39076, #23342, #5359 ) ;
#5537 = FACE_OUTER_BOUND ( 'NONE', #16531, .T. ) ;
#5538 = VECTOR ( 'NONE', #26425, 1000.000000000000000 ) ;
#5539 = CARTESIAN_POINT ( 'NONE',  ( -24.41897112398753933, -17.37347453850100720, 69.59835118672229726 ) ) ;
#5540 = VERTEX_POINT ( 'NONE', #4889 ) ;
#5541 = CARTESIAN_POINT ( 'NONE',  ( -24.18037252889021005, -17.94870914462638822, 59.18873732074431615 ) ) ;
#5542 = EDGE_CURVE ( 'NONE', #13202, #1590, #21039, .T. ) ;
#5543 = CIRCLE ( 'NONE', #25214, 5.000000000000000000 ) ;
#5544 = CARTESIAN_POINT ( 'NONE',  ( -10.52215041504658188, -13.37196039468857833, 74.97817647370040106 ) ) ;
#5545 = EDGE_CURVE ( 'NONE', #13075, #21204, #34410, .T. ) ;
#5546 = ORIENTED_EDGE ( 'NONE', *, *, #8535, .F. ) ;
#5547 = DIRECTION ( 'NONE',  ( 0.09855345062332551698, 0.9951317587989213509, 3.188559572831062401E-08 ) ) ;
#5548 = CARTESIAN_POINT ( 'NONE',  ( -12.21605471856059921, -19.48707561184010117, 57.94298983722725183 ) ) ;
#5549 = EDGE_CURVE ( 'NONE', #26266, #43656, #19405, .T. ) ;
#5551 = EDGE_CURVE ( 'NONE', #45668, #42703, #35581, .T. ) ;
#5550 = ORIENTED_EDGE ( 'NONE', *, *, #48609, .T. ) ;
#5552 = DIRECTION ( 'NONE',  ( 0.9048399035850772654, 0.4257519804770707461, 1.330923649722295902E-08 ) ) ;
#5553 = ADVANCED_FACE ( 'NONE', ( #9065 ), #38845, .T. ) ;
#5554 = CARTESIAN_POINT ( 'NONE',  ( -12.00117731135775578, -10.30420433458623819, 67.79896860124506475 ) ) ;
#5555 = CARTESIAN_POINT ( 'NONE',  ( -10.76763551407085373, -17.13171859787639661, 61.45743118825841833 ) ) ;
#5556 = CARTESIAN_POINT ( 'NONE',  ( -17.03658212107600534, -14.90837637761270429, 49.52966884056655772 ) ) ;
#5557 = ORIENTED_EDGE ( 'NONE', *, *, #12595, .T. ) ;
#5558 = CARTESIAN_POINT ( 'NONE',  ( -10.70532053225239366, -12.67267096592666675, 61.08381491717225487 ) ) ;
#5559 = CARTESIAN_POINT ( 'NONE',  ( -10.39693166811831304, -15.37990016280386740, 57.58264896457095006 ) ) ;
#5560 = CARTESIAN_POINT ( 'NONE',  ( -23.19948571119275726, -18.85291137746750323, 65.83861571032234394 ) ) ;
#5561 = DIRECTION ( 'NONE',  ( 0.4332512900281770274, -0.1108752438054627226, 0.8944271909999157444 ) ) ;
#5562 = CONTEXT_DEPENDENT_SHAPE_REPRESENTATION ( #7066, #34251 ) ;
#5563 = CARTESIAN_POINT ( 'NONE',  ( -17.73224099643095286, -22.30287356026373047, 53.49999999999994316 ) ) ;
#5564 = CARTESIAN_POINT ( 'NONE',  ( -21.39914427356725213, -17.29159580171669219, 49.52966884056655772 ) ) ;
#5565 = CARTESIAN_POINT ( 'NONE',  ( 18.54465614458695200, 3.140741878271521070, 50.53406581128081143 ) ) ;
#5566 = ORIENTED_EDGE ( 'NONE', *, *, #44339, .F. ) ;
#5567 = DIRECTION ( 'NONE',  ( -3.071710424422018668E-17, 6.404604876783312462E-16, 1.000000000000000000 ) ) ;
#5568 = CARTESIAN_POINT ( 'NONE',  ( -10.52422430310768320, -17.61911375464911700, 68.21226508126260057 ) ) ;
#5569 = CARTESIAN_POINT ( 'NONE',  ( -21.08780618903275439, -10.68911097779236385, 53.69233794759168887 ) ) ;
#5570 = ORIENTED_EDGE ( 'NONE', *, *, #30786, .T. ) ;
#5571 = CARTESIAN_POINT ( 'NONE',  ( -19.90433039125390025, -21.83431899736824988, 69.04987161812600505 ) ) ;
#5572 = EDGE_LOOP ( 'NONE', ( #5896, #24563, #3952, #26022 ) ) ;
#5573 = ADVANCED_FACE ( 'NONE', ( #15698 ), #706, .F. ) ;
#5574 = VERTEX_POINT ( 'NONE', #20136 ) ;
#5575 = ORIENTED_EDGE ( 'NONE', *, *, #40257, .T. ) ;
#5577 = CARTESIAN_POINT ( 'NONE',  ( -16.92409385541305511, -14.80920654474410547, 47.99999999999998579 ) ) ;
#5576 = AXIS2_PLACEMENT_3D ( 'NONE', #22680, #12084, #41381 ) ;
#5578 = DIRECTION ( 'NONE',  ( -0.3566357048164924270, 0.9342435303763380050, -8.054691247152028744E-09 ) ) ;
#5579 =( BOUNDED_CURVE ( )  B_SPLINE_CURVE ( 3, ( #23790, #8281, #24032, #5073 ),
 .UNSPECIFIED., .F., .F. ) 
 B_SPLINE_CURVE_WITH_KNOTS ( ( 4, 4 ),
 ( 0.5000000000000000000, 0.9074455897393697290 ),
 .UNSPECIFIED. ) 
 CURVE ( )  GEOMETRIC_REPRESENTATION_ITEM ( )  RATIONAL_B_SPLINE_CURVE ( ( 1.000000000000022649, 0.4567392136813365200, 0.3561768502900160560, 0.6983129098260858481 ) ) 
 REPRESENTATION_ITEM ( '' )  );
#5580 = CYLINDRICAL_SURFACE ( 'NONE', #30675, 5.249999999999998224 ) ;
#5581 = CARTESIAN_POINT ( 'NONE',  ( -24.70797074432933371, -13.24467984323328551, 59.56279132098635642 ) ) ;
#5582 = CARTESIAN_POINT ( 'NONE',  ( -16.29069520099238133, -22.17261162040731648, 61.93380917110247452 ) ) ;
#5583 = ORIENTED_EDGE ( 'NONE', *, *, #29523, .T. ) ;
#5584 = EDGE_LOOP ( 'NONE', ( #4840, #36723, #14127, #35441, #39123 ) ) ;
#5585 = CARTESIAN_POINT ( 'NONE',  ( -22.66784385650551670, -6.428312510596451368, 51.20221977374900035 ) ) ;
#5586 = CARTESIAN_POINT ( 'NONE',  ( -17.66159697976433307, -21.85550285805611637, 58.42025434932890704 ) ) ;
#5587 = DIRECTION ( 'NONE',  ( -3.071710424422018668E-17, 6.404604876783312462E-16, 1.000000000000000000 ) ) ;
#5588 = AXIS2_PLACEMENT_3D ( 'NONE', #29671, #7282, #40276 ) ;
#5589 = CARTESIAN_POINT ( 'NONE',  ( -19.80301227694363675, -21.44571519258606074, 69.08482476707463604 ) ) ;
#5590 = CARTESIAN_POINT ( 'NONE',  ( -23.06159385650551386, -9.295667164867525756, 49.30633214617472504 ) ) ;
#5591 =( BOUNDED_CURVE ( )  B_SPLINE_CURVE ( 2, ( #29366, #34019, #19015, #26402, #29608, #66, #36972, #15054, #41177 ),
 .UNSPECIFIED., .F., .F. ) 
 B_SPLINE_CURVE_WITH_KNOTS ( ( 3, 2, 2, 2, 3 ),
 ( 0.01573617513994363115, 0.01671960456604025536, 0.01770303399213687956, 0.01868646341823350029, 0.01966989284433012450 ),
 .UNSPECIFIED. ) 
 CURVE ( )  GEOMETRIC_REPRESENTATION_ITEM ( )  RATIONAL_B_SPLINE_CURVE ( ( 1.000000000000510925, 0.9238795325107758138, 1.000000000000000000, 0.9238795325112867385, 1.000000000000000000, 0.9238795325112867385, 1.000000000000000000, 0.9238795325112530987, 1.000000000000033751 ) ) 
 REPRESENTATION_ITEM ( '' )  );
#5592 = ORIENTED_EDGE ( 'NONE', *, *, #36859, .F. ) ;
#5593 = DIRECTION ( 'NONE',  ( -0.9999247414263408018, 0.01226831216845469807, 5.367905339378915168E-08 ) ) ;
#5594 = DIRECTION ( 'NONE',  ( 0.8603613874411346618, -0.3191920208248670288, -0.3973597071195111852 ) ) ;
#5595 = AXIS2_PLACEMENT_3D ( 'NONE', #32535, #18652, #30257 ) ;
#5596 = DIRECTION ( 'NONE',  ( -0.7364384864160969935, 0.6765045127160409510, 1.031360481960658298E-08 ) ) ;
#5597 = B_SPLINE_CURVE_WITH_KNOTS ( 'NONE', 1,
 ( #38285, #27891 ),
 .UNSPECIFIED., .F., .F.,
 ( 2, 2 ),
 ( 0.000000000000000000, 1.000000000000000000 ),
 .UNSPECIFIED. ) ;
#5598 = EDGE_LOOP ( 'NONE', ( #4107, #24962, #46171, #1514 ) ) ;
#5599 = CARTESIAN_POINT ( 'NONE',  ( -11.60677440104695890, -18.70493592551879658, 68.28860005670347277 ) ) ;
#5600 = AXIS2_PLACEMENT_3D ( 'NONE', #36912, #29541, #10826 ) ;
#5601 = CARTESIAN_POINT ( 'NONE',  ( -10.38025826595154477, -14.36272272558099772, 71.47215414551031643 ) ) ;
#5602 = CARTESIAN_POINT ( 'NONE',  ( -24.46479344177693349, -14.44719919422189491, 66.18292729247950490 ) ) ;
#5603 = EDGE_CURVE ( 'NONE', #5635, #21906, #14304, .T. ) ;
#5604 = ADVANCED_FACE ( 'NONE', ( #30516 ), #45532, .T. ) ;
#5605 = CARTESIAN_POINT ( 'NONE',  ( -22.58763249286555208, -20.18056880150341215, 65.81766459098905386 ) ) ;
#5606 = AXIS2_PLACEMENT_3D ( 'NONE', #31947, #5371, #43030 ) ;
#5607 = VERTEX_POINT ( 'NONE', #12260 ) ;
#5608 = DIRECTION ( 'NONE',  ( 0.000000000000000000, 0.000000000000000000, 1.000000000000000000 ) ) ;
#5609 = CARTESIAN_POINT ( 'NONE',  ( -24.82569768056232107, -15.65743930089875668, 73.19642064348015253 ) ) ;
#5610 = DIRECTION ( 'NONE',  ( -6.516572651863732626E-06, 8.834921937557814562E-06, 0.9999999999397393147 ) ) ;
#5611 = ORIENTED_EDGE ( 'NONE', *, *, #33591, .T. ) ;
#5612 = DIRECTION ( 'NONE',  ( 0.9968684284758858594, -0.07907803935364897396, 1.831731161803828584E-08 ) ) ;
#5613 = VERTEX_POINT ( 'NONE', #11787 ) ;
#5614 = CARTESIAN_POINT ( 'NONE',  ( -22.63560516303400050, -20.13310814558360917, 69.28922553891734992 ) ) ;
#5615 = EDGE_CURVE ( 'NONE', #30692, #6106, #47379, .T. ) ;
#5616 = EDGE_CURVE ( 'NONE', #38015, #35776, #34905, .T. ) ;
#5617 = CARTESIAN_POINT ( 'NONE',  ( -9.983049145142542713, -14.44146248316089753, 67.98083219581930337 ) ) ;
#5618 = ORIENTED_EDGE ( 'NONE', *, *, #24122, .F. ) ;
#5619 = CARTESIAN_POINT ( 'NONE',  ( -22.17789279454246554, -20.54546261288653852, 58.95781210373504422 ) ) ;
#5620 = DIRECTION ( 'NONE',  ( 0.9687793358424819923, -0.2479245821708678799, -1.824489850066507969E-17 ) ) ;
#5621 = CARTESIAN_POINT ( 'NONE',  ( -24.21458799606873669, -12.91388130977151327, 66.60246716606879147 ) ) ;
#5622 = DIRECTION ( 'NONE',  ( 0.6205284308219133349, 0.7841839494287637935, 1.702810348471058466E-17 ) ) ;
#5623 = VERTEX_POINT ( 'NONE', #23601 ) ;
#5624 = CARTESIAN_POINT ( 'NONE',  ( -11.46043843694620179, -11.04924462883820802, 57.50903212149482613 ) ) ;
#5625 = CIRCLE ( 'NONE', #4079, 4.686499999999999666 ) ;
#5626 = CARTESIAN_POINT ( 'NONE',  ( -20.52762743779272014, -8.534807845156915818, 63.31121513079826713 ) ) ;
#5627 = CARTESIAN_POINT ( 'NONE',  ( -22.22370946352282672, -9.111183370010303761, 59.90666632495347699 ) ) ;
#5628 = ORIENTED_EDGE ( 'NONE', *, *, #14146, .T. ) ;
#5629 = CARTESIAN_POINT ( 'NONE',  ( -17.46222794319647775, -7.759011850482251837, 67.03511641684839617 ) ) ;
#5630 = CARTESIAN_POINT ( 'NONE',  ( -42.43291738482482600, -14.80920654474415699, 62.92941176470587550 ) ) ;
#5631 = B_SPLINE_CURVE_WITH_KNOTS ( 'NONE', 3,
 ( #22542, #6558, #37537, #30192, #3577, #14624, #21580, #36803, #44976, #3838 ),
 .UNSPECIFIED., .F., .F.,
 ( 4, 2, 2, 2, 4 ),
 ( 0.000000000000000000, 0.2500000000000000000, 0.5000000000000000000, 0.7500000000000000000, 1.000000000000000000 ),
 .UNSPECIFIED. ) ;
#5632 = EDGE_CURVE ( 'NONE', #29649, #34219, #2396, .T. ) ;
#5634 = EDGE_LOOP ( 'NONE', ( #15445, #3816 ) ) ;
#5633 = AXIS2_PLACEMENT_3D ( 'NONE', #33864, #41023, #7053 ) ;
#5635 = VERTEX_POINT ( 'NONE', #28972 ) ;
#5636 = CARTESIAN_POINT ( 'NONE',  ( -23.71751471349159601, -11.63122711669449316, 63.23746208799618529 ) ) ;
#5637 = CARTESIAN_POINT ( 'NONE',  ( -50.42609385541305755, -14.80920654474424225, 70.07647058823528141 ) ) ;
#5638 = CARTESIAN_POINT ( 'NONE',  ( -10.96149970135419061, -18.51576062833312974, 58.06360531077050524 ) ) ;
#5639 = CARTESIAN_POINT ( 'NONE',  ( -17.01159385650551670, -6.922745924619793101, 51.69366785382590024 ) ) ;
#5640 = CARTESIAN_POINT ( 'NONE',  ( -20.47136568995129480, -10.23054578351414001, 53.49999999999995026 ) ) ;
#5641 = CARTESIAN_POINT ( 'NONE',  ( -16.15640231613377154, -10.29741749701175380, 49.52966884056655772 ) ) ;
#5642 = CARTESIAN_POINT ( 'NONE',  ( -17.72612443559818018, -7.765381109175947927, 60.36588690973874094 ) ) ;
#5643 = ORIENTED_EDGE ( 'NONE', *, *, #11819, .F. ) ;
#5644 = ORIENTED_EDGE ( 'NONE', *, *, #48391, .T. ) ;
#5646 = CARTESIAN_POINT ( 'NONE',  ( -12.34715986329718085, -20.26164850408625284, 68.45940522080938706 ) ) ;
#5645 = VECTOR ( 'NONE', #14132, 1000.000000000000000 ) ;
#5647 = CARTESIAN_POINT ( 'NONE',  ( -0.9999999999999940048, 0.000000000000000000, -9.000000000000014211 ) ) ;
#5648 = CARTESIAN_POINT ( 'NONE',  ( -17.42409385541299471, -14.80920654474435594, 52.02966884056656482 ) ) ;
#5649 = CARTESIAN_POINT ( 'NONE',  ( -19.67760665824181388, -21.48965406232008490, 65.75014118398131302 ) ) ;
#5650 = CARTESIAN_POINT ( 'NONE',  ( -13.35685073114381716, -8.567315923767541364, 57.01321801328607108 ) ) ;
#5651 = DIRECTION ( 'NONE',  ( 0.9687793358424819923, -0.2479245821708680464, 0.000000000000000000 ) ) ;
#5652 = ORIENTED_EDGE ( 'NONE', *, *, #10613, .T. ) ;
#5653 = CARTESIAN_POINT ( 'NONE',  ( -20.54979551517892489, -8.489990701729437816, 63.31121512946744190 ) ) ;
#5654 = CARTESIAN_POINT ( 'NONE',  ( -23.99312268326606201, -11.29471679256767125, 66.60709928216182618 ) ) ;
#5655 = CARTESIAN_POINT ( 'NONE',  ( -11.06712629860931152, -18.69414434431124761, 61.39215439313597500 ) ) ;
#5656 = AXIS2_PLACEMENT_3D ( 'NONE', #42603, #23881, #35424 ) ;
#5657 = EDGE_LOOP ( 'NONE', ( #7722, #2967, #2725, #12120 ) ) ;
#5658 = CARTESIAN_POINT ( 'NONE',  ( -10.12481675042743667, -13.31795058064993853, 74.87091791722596668 ) ) ;
#5659 = CARTESIAN_POINT ( 'NONE',  ( -24.01565389239745585, -17.31039229478603048, 69.41899553355973751 ) ) ;
#5660 = ADVANCED_FACE ( 'NONE', ( #2629 ), #13693, .T. ) ;
#5661 = SURFACE_STYLE_USAGE ( .BOTH. , #37057 ) ;
#5662 =( BOUNDED_CURVE ( )  B_SPLINE_CURVE ( 3, ( #16686, #1433, #35878, #46748 ),
 .UNSPECIFIED., .F., .F. ) 
 B_SPLINE_CURVE_WITH_KNOTS ( ( 4, 4 ),
 ( 0.4074455897393622350, 0.5000000000000000000 ),
 .UNSPECIFIED. ) 
 CURVE ( )  GEOMETRIC_REPRESENTATION_ITEM ( )  RATIONAL_B_SPLINE_CURVE ( ( 0.6983129098260739687, 0.7760317562606696695, 0.8765941196519746459, 0.9999999999999807931 ) ) 
 REPRESENTATION_ITEM ( '' )  );
#5663 = CARTESIAN_POINT ( 'NONE',  ( -24.03160975973305824, -17.26750547207224784, 69.56339792588553905 ) ) ;
#5664 = CARTESIAN_POINT ( 'NONE',  ( -23.47957010007013778, -11.29750547940444427, 69.90713163543374264 ) ) ;
#5665 = ORIENTED_EDGE ( 'NONE', *, *, #13423, .F. ) ;
#5666 = CARTESIAN_POINT ( 'NONE',  ( -23.65366066840426029, -18.89546231072650784, 69.45518534502666341 ) ) ;
#5667 = ORIENTED_EDGE ( 'NONE', *, *, #8161, .F. ) ;
#5668 = ADVANCED_FACE ( 'NONE', ( #9306 ), #10590, .T. ) ;
#5669 = CARTESIAN_POINT ( 'NONE',  ( -14.96159385759799143, -7.228003583438117552, 51.38655588711986155 ) ) ;
#5671 = CARTESIAN_POINT ( 'NONE',  ( -21.50087588749055811, -8.572740410265922151, 73.71473348964758543 ) ) ;
#5670 = AXIS2_PLACEMENT_3D ( 'NONE', #45030, #33917, #18398 ) ;
#5672 = ORIENTED_EDGE ( 'NONE', *, *, #13871, .F. ) ;
#5673 = CARTESIAN_POINT ( 'NONE',  ( -15.77409385541301035, -6.859212275519753099, 50.50378509014291240 ) ) ;
#5674 = ADVANCED_FACE ( 'NONE', ( #13926 ), #3992, .T. ) ;
#5675 = CARTESIAN_POINT ( 'NONE',  ( -15.52409385650551421, -6.426201560718813433, 50.50509628382439331 ) ) ;
#5676 = VECTOR ( 'NONE', #13776, 1000.000000000000227 ) ;
#5677 = ORIENTED_EDGE ( 'NONE', *, *, #41950, .F. ) ;
#5678 = CARTESIAN_POINT ( 'NONE',  ( -15.34465393633500696, -21.54586957516256263, 68.86120835375241711 ) ) ;
#5679 = ADVANCED_FACE ( 'NONE', ( #28256 ), #15611, .T. ) ;
#5680 = CARTESIAN_POINT ( 'NONE',  ( -19.79661600260421750, -8.166467367689241641, 73.72096660036417859 ) ) ;
#5681 = CARTESIAN_POINT ( 'NONE',  ( -16.36675962830097930, -22.18387328577503581, 61.79922180027413958 ) ) ;
#5682 = EDGE_LOOP ( 'NONE', ( #10343, #23727, #16566, #9906, #18384 ) ) ;
#5683 = CARTESIAN_POINT ( 'NONE',  ( -23.86876348378221024, -17.54180441657964096, 62.75895669395315224 ) ) ;
#5684 = CARTESIAN_POINT ( 'NONE',  ( -10.90856645720024254, -17.50971350489534828, 64.51250748301919202 ) ) ;
#5685 = DIRECTION ( 'NONE',  ( 7.130145686591618268E-06, -1.088473442731139027E-05, -0.9999999999153417196 ) ) ;
#5686 = DIRECTION ( 'NONE',  ( 1.000000000000000000, 0.000000000000000000, 0.000000000000000000 ) ) ;
#5687 = EDGE_CURVE ( 'NONE', #46547, #46160, #30741, .T. ) ;
#5688 = ORIENTED_EDGE ( 'NONE', *, *, #38380, .F. ) ;
#5689 = ORIENTED_EDGE ( 'NONE', *, *, #612, .T. ) ;
#5690 = CARTESIAN_POINT ( 'NONE',  ( -22.51726279860821478, -19.68384809141796765, 72.64400547081167758 ) ) ;
#5691 = CARTESIAN_POINT ( 'NONE',  ( -21.35412623182586955, -20.66579906811421452, 68.93961316870652922 ) ) ;
#5692 = ORIENTED_EDGE ( 'NONE', *, *, #17278, .T. ) ;
#5693 = CARTESIAN_POINT ( 'NONE',  ( -19.92409385541305511, -14.80920654474410725, 81.99999999999998579 ) ) ;
#5694 = CARTESIAN_POINT ( 'NONE',  ( -19.27094009026993859, -21.56284704995934831, 62.10576782500217519 ) ) ;
#5695 = CARTESIAN_POINT ( 'NONE',  ( -18.50534385759798894, -7.595227055684746986, 51.75156210489594599 ) ) ;
#5696 = CARTESIAN_POINT ( 'NONE',  ( -10.42751908256963311, -15.03006480610451234, 74.87066898757765898 ) ) ;
#5697 = DIRECTION ( 'NONE',  ( 0.9687793358424821033, -0.2479245821708677133, 0.000000000000000000 ) ) ;
#5698 = CARTESIAN_POINT ( 'NONE',  ( -12.26133756782281203, -10.08196798276019557, 60.57420568413689210 ) ) ;
#5699 = ORIENTED_EDGE ( 'NONE', *, *, #40554, .T. ) ;
#5700 = FACE_OUTER_BOUND ( 'NONE', #46447, .T. ) ;
#5701 = FACE_OUTER_BOUND ( 'NONE', #44006, .T. ) ;
#5702 = FACE_OUTER_BOUND ( 'NONE', #42984, .T. ) ;
#5703 = CARTESIAN_POINT ( 'NONE',  ( -22.81633530706992019, -9.668548653678303850, 73.68149876278019406 ) ) ;
#5704 = CARTESIAN_POINT ( 'NONE',  ( -13.54291469596969577, -20.63483873347275122, 61.51646374974303200 ) ) ;
#5705 = VERTEX_POINT ( 'NONE', #40063 ) ;
#5706 = ORIENTED_EDGE ( 'NONE', *, *, #12386, .F. ) ;
#5707 = ORIENTED_EDGE ( 'NONE', *, *, #2290, .T. ) ;
#5708 = CARTESIAN_POINT ( 'NONE',  ( -28.42409385541305511, -6.859206544744110623, 54.49999999999997158 ) ) ;
#5709 = DIRECTION ( 'NONE',  ( -1.000000000000000000, 0.000000000000000000, 0.000000000000000000 ) ) ;
#5710 = DIRECTION ( 'NONE',  ( -3.413470714839332458E-33, 1.190614954331866791E-16, -1.000000000000000000 ) ) ;
#5711 =( BOUNDED_SURFACE ( )  B_SPLINE_SURFACE ( 3, 1, ( 
 ( #1622, #657 ),
 ( #16134, #19610 ),
 ( #38557, #38806 ),
 ( #5324, #31178 ),
 ( #23310, #27724 ),
 ( #45960, #12706 ),
 ( #46200, #30948 ) ),
 .UNSPECIFIED., .T., .F., .F. ) 
 B_SPLINE_SURFACE_WITH_KNOTS ( ( 4, 3, 4 ),
 ( 2, 2 ),
 ( 0.000000000000000000, 0.5000000000000000000, 1.000000000000000000 ),
 ( 0.000000000000000000, 1.000000000000000000 ),
 .UNSPECIFIED. ) 
 GEOMETRIC_REPRESENTATION_ITEM ( )  RATIONAL_B_SPLINE_SURFACE ( (
 ( 1.000000000000000000, 1.000000000000000000),
 ( 0.3333333333333335369, 0.3333333333333330373),
 ( 0.3333333333333335369, 0.3333333333333330373),
 ( 1.000000000000000000, 1.000000000000000000),
 ( 0.3333333333333333703, 0.3333333333333333703),
 ( 0.3333333333333333703, 0.3333333333333333703),
 ( 1.000000000000000000, 1.000000000000000000) ) ) 
 REPRESENTATION_ITEM ( '' )  SURFACE ( )  );
#5712 = EDGE_CURVE ( 'NONE', #38928, #19353, #10996, .T. ) ;
#5713 = EDGE_LOOP ( 'NONE', ( #17413, #19574, #44445, #44070, #28697, #28326, #10093, #10707 ) ) ;
#5714 = B_SPLINE_CURVE_WITH_KNOTS ( 'NONE', 1,
 ( #31304, #31549 ),
 .UNSPECIFIED., .F., .F.,
 ( 2, 2 ),
 ( 0.000000000000000000, 1.000000000000000000 ),
 .UNSPECIFIED. ) ;
#5715 = CARTESIAN_POINT ( 'NONE',  ( -16.23805205469483681, -7.454097322849217555, 60.37841262270664089 ) ) ;
#5716 = CARTESIAN_POINT ( 'NONE',  ( -10.01086014178825323, -14.06997349321342483, 61.06821291928545747 ) ) ;
#5717 = EDGE_CURVE ( 'NONE', #12076, #21448, #8555, .T. ) ;
#5718 = ORIENTED_EDGE ( 'NONE', *, *, #26514, .T. ) ;
#5719 = CARTESIAN_POINT ( 'NONE',  ( -13.43773910423563400, -20.62433115109003268, 58.33177939114180788 ) ) ;
#5720 = LINE ( 'NONE', #20728, #16300 ) ;
#5721 = ORIENTED_EDGE ( 'NONE', *, *, #37434, .F. ) ;
#5722 = CARTESIAN_POINT ( 'NONE',  ( -23.34092575347512266, -10.28207967581048088, 59.78698817202694471 ) ) ;
#5723 = ORIENTED_EDGE ( 'NONE', *, *, #42481, .F. ) ;
#5724 =( BOUNDED_CURVE ( )  B_SPLINE_CURVE ( 3, ( #1623, #4846, #35353, #16136 ),
 .UNSPECIFIED., .F., .F. ) 
 B_SPLINE_CURVE_WITH_KNOTS ( ( 4, 4 ),
 ( 0.4074455897393660098, 0.5000000000000000000 ),
 .UNSPECIFIED. ) 
 CURVE ( )  GEOMETRIC_REPRESENTATION_ITEM ( )  RATIONAL_B_SPLINE_CURVE ( ( 0.6983129098260920653, 0.7760317562606868780, 0.8765941196519864143, 0.9999999999999834577 ) ) 
 REPRESENTATION_ITEM ( '' )  );
#5725 = CARTESIAN_POINT ( 'NONE',  ( -10.59609684676525276, -13.26671058769154676, 71.22330973224352135 ) ) ;
#5726 = ORIENTED_EDGE ( 'NONE', *, *, #16020, .T. ) ;
#5727 = CARTESIAN_POINT ( 'NONE',  ( -11.91343869374197695, -19.82283377674160718, 58.04186948019505365 ) ) ;
#5728 = CARTESIAN_POINT ( 'NONE',  ( -12.27729947935473476, -9.991218615320079266, 60.85918086709605745 ) ) ;
#5729 = CARTESIAN_POINT ( 'NONE',  ( -19.44371787714632305, -21.98101111209947334, 58.63852002154196441 ) ) ;
#5730 = ORIENTED_EDGE ( 'NONE', *, *, #1319, .T. ) ;
#5731 = FACE_OUTER_BOUND ( 'NONE', #5504, .T. ) ;
#5732 = CARTESIAN_POINT ( 'NONE',  ( -24.69852204723760281, -16.41745771733451775, 59.30827817708741634 ) ) ;
#5733 = EDGE_CURVE ( 'NONE', #32337, #21832, #24435, .T. ) ;
#5734 = CARTESIAN_POINT ( 'NONE',  ( -50.42609385541305755, -14.80920654474414810, 61.02352941176469869 ) ) ;
#5735 = EDGE_CURVE ( 'NONE', #10202, #34559, #19364, .T. ) ;
#5736 = CARTESIAN_POINT ( 'NONE',  ( -19.86401518824997581, -21.42384811948916479, 69.22010401872219632 ) ) ;
#5737 = FACE_OUTER_BOUND ( 'NONE', #13058, .T. ) ;
#5738 = CARTESIAN_POINT ( 'NONE',  ( -10.38069781390674251, -17.23693455343903480, 61.26468960721474843 ) ) ;
#5739 = ORIENTED_EDGE ( 'NONE', *, *, #20014, .F. ) ;
#5740 = PLANE ( 'NONE',  #46708 ) ;
#5741 =( BOUNDED_SURFACE ( )  B_SPLINE_SURFACE ( 3, 1, ( 
 ( #47666, #14140 ),
 ( #21798, #17119 ),
 ( #28232, #32172 ),
 ( #43263, #29197 ),
 ( #28948, #40042 ),
 ( #47190, #21574 ),
 ( #13434, #6055 ) ),
 .UNSPECIFIED., .T., .F., .F. ) 
 B_SPLINE_SURFACE_WITH_KNOTS ( ( 4, 3, 4 ),
 ( 2, 2 ),
 ( 0.000000000000000000, 0.5000000000000000000, 1.000000000000000000 ),
 ( 0.000000000000000000, 1.000000000000000000 ),
 .UNSPECIFIED. ) 
 GEOMETRIC_REPRESENTATION_ITEM ( )  RATIONAL_B_SPLINE_SURFACE ( (
 ( 1.000000000000000000, 1.000000000000000000),
 ( 0.3333333333333335369, 0.3333333333333330373),
 ( 0.3333333333333335369, 0.3333333333333330373),
 ( 1.000000000000000000, 1.000000000000000000),
 ( 0.3333333333333333703, 0.3333333333333333703),
 ( 0.3333333333333333703, 0.3333333333333333703),
 ( 1.000000000000000000, 1.000000000000000000) ) ) 
 REPRESENTATION_ITEM ( '' )  SURFACE ( )  );
#5742 = CARTESIAN_POINT ( 'NONE',  ( -24.65603385937463088, -13.01988417981330315, 63.03252945310004662 ) ) ;
#5743 = B_SPLINE_CURVE_WITH_KNOTS ( 'NONE', 3,
 ( #8607, #5646, #16930, #35415, #20416, #38874, #23632, #42819, #31244, #38629 ),
 .UNSPECIFIED., .F., .F.,
 ( 4, 2, 2, 2, 4 ),
 ( 0.1272669073658327099, 0.2522669073488013614, 0.3772669073317700406, 0.5022669073147386642, 0.6272669072977072879 ),
 .UNSPECIFIED. ) ;
#5744 = CARTESIAN_POINT ( 'NONE',  ( -21.35673258969864818, -10.96416394607318701, 53.49899999999994549 ) ) ;
#5745 = EDGE_CURVE ( 'NONE', #10314, #1656, #28535, .T. ) ;
#5746 = CARTESIAN_POINT ( 'NONE',  ( -19.98494827787780181, -21.80542074767473437, 69.07335975967473018 ) ) ;
#5747 = CARTESIAN_POINT ( 'NONE',  ( -15.15534385650551741, -7.417179338643134834, 52.18511593390279302 ) ) ;
#5748 = ORIENTED_EDGE ( 'NONE', *, *, #10890, .F. ) ;
#5749 = CARTESIAN_POINT ( 'NONE',  ( -21.68499379980493558, -9.192514338196573931, 66.96149992326067490 ) ) ;
#5750 = LINE ( 'NONE', #36474, #45445 ) ;
#5751 = ORIENTED_EDGE ( 'NONE', *, *, #1575, .T. ) ;
#5752 = FACE_OUTER_BOUND ( 'NONE', #10936, .T. ) ;
#5753 = CARTESIAN_POINT ( 'NONE',  ( -10.53028993777715883, -16.28642212234895226, 71.73278239416407587 ) ) ;
#5754 = CARTESIAN_POINT ( 'NONE',  ( -22.75539019595755263, -10.19575032747719590, 66.82710158566565894 ) ) ;
#5755 = CARTESIAN_POINT ( 'NONE',  ( -19.37484727228654080, -7.619050864103940057, 60.14588289477547534 ) ) ;
#5756 = EDGE_CURVE ( 'NONE', #24418, #47047, #25762, .T. ) ;
#5757 = VERTEX_POINT ( 'NONE', #14642 ) ;
#5758 = CARTESIAN_POINT ( 'NONE',  ( -23.70135487130767515, -11.71146637837649074, 63.25218278684473461 ) ) ;
#5759 = DIRECTION ( 'NONE',  ( 3.549360974551883545E-17, -6.371834667872732552E-18, -1.000000000000000000 ) ) ;
#5760 = EDGE_LOOP ( 'NONE', ( #19411, #44640, #8100, #24991 ) ) ;
#5761 = CARTESIAN_POINT ( 'NONE',  ( -21.22358616875703063, -21.29681159568578153, 53.76227901944321275 ) ) ;
#5762 = CARTESIAN_POINT ( 'NONE',  ( -22.07409385541323488, -6.859212275519745994, 50.50378509014079498 ) ) ;
#5763 = B_SPLINE_CURVE_WITH_KNOTS ( 'NONE', 3,
 ( #15805, #35244, #19268, #562, #23946, #46102, #23716, #45872, #46352, #8432 ),
 .UNSPECIFIED., .F., .F.,
 ( 4, 2, 2, 2, 4 ),
 ( 0.1272669073658498906, 0.2522669073463310041, 0.3772669073268121176, 0.5022669073072931756, 0.6272669072877743446 ),
 .UNSPECIFIED. ) ;
#5764 = CARTESIAN_POINT ( 'NONE',  ( -13.18991935570955576, -8.679356915182284027, 60.63224404241364596 ) ) ;
#5765 = CARTESIAN_POINT ( 'NONE',  ( -21.12013511752277495, -20.75402118300628018, 69.35450231647695318 ) ) ;
#5766 = CARTESIAN_POINT ( 'NONE',  ( -10.76458884141051975, -11.46785096862322995, 71.27516169247240896 ) ) ;
#5767 = CARTESIAN_POINT ( 'NONE',  ( -10.73729177923718758, -12.73729707409820122, 64.28452752943745452 ) ) ;
#5768 = VERTEX_POINT ( 'NONE', #29703 ) ;
#5769 = ORIENTED_EDGE ( 'NONE', *, *, #29800, .F. ) ;
#5770 = CARTESIAN_POINT ( 'NONE',  ( -16.56159385541304019, -7.228003583438117552, 51.38655588711986155 ) ) ;
#5771 = CARTESIAN_POINT ( 'NONE',  ( -10.37491704552005167, -14.91954605113452459, 75.09778880425432135 ) ) ;
#5772 = AXIS2_PLACEMENT_3D ( 'NONE', #34575, #1096, #38517 ) ;
#5773 = CARTESIAN_POINT ( 'NONE',  ( -14.06039897761215762, -8.161786889575166626, 70.92946410255460421 ) ) ;
#5774 = ADVANCED_FACE ( 'NONE', ( #22316 ), #14400, .T. ) ;
#5775 = CYLINDRICAL_SURFACE ( 'NONE', #30051, 2.000000000000003109 ) ;
#5776 = CARTESIAN_POINT ( 'NONE',  ( -24.79781836340079337, -15.87314503134675014, 69.64812095075065201 ) ) ;
#5777 = ORIENTED_EDGE ( 'NONE', *, *, #29503, .F. ) ;
#5778 = CARTESIAN_POINT ( 'NONE',  ( -20.98579777188748707, -20.83533835786949950, 65.58453944793343737 ) ) ;
#5779 = CARTESIAN_POINT ( 'NONE',  ( -24.24654216478982960, -17.80199886438881762, 62.67372181833962230 ) ) ;
#5780 = ORIENTED_EDGE ( 'NONE', *, *, #46869, .T. ) ;
#5781 = CYLINDRICAL_SURFACE ( 'NONE', #6057, 0.1499999999999962474 ) ;
#5782 = EDGE_CURVE ( 'NONE', #26257, #23869, #33632, .T. ) ;
#5783 = DIRECTION ( 'NONE',  ( 0.000000000000000000, 0.000000000000000000, 1.000000000000000000 ) ) ;
#5784 = ORIENTED_EDGE ( 'NONE', *, *, #14022, .F. ) ;
#5785 = B_SPLINE_CURVE_WITH_KNOTS ( 'NONE', 3,
 ( #23992, #24235, #5767, #39241, #2054, #13116, #38993, #1569, #17054, #28159 ),
 .UNSPECIFIED., .F., .F.,
 ( 4, 2, 2, 2, 4 ),
 ( 0.000000000000000000, 0.2500000000000000000, 0.5000000000000000000, 0.7500000000000000000, 1.000000000000000000 ),
 .UNSPECIFIED. ) ;
#5786 = CARTESIAN_POINT ( 'NONE',  ( -24.48810908846319734, -17.17637088580320537, 73.06831457992643664 ) ) ;
#5787 = CARTESIAN_POINT ( 'NONE',  ( -18.64993026675905341, -21.70103686862637105, 72.47614041008449703 ) ) ;
#5788 = VERTEX_POINT ( 'NONE', #18602 ) ;
#5789 = CARTESIAN_POINT ( 'NONE',  ( -23.80321465417087978, -17.81075909821204917, 59.15378417737379380 ) ) ;
#5790 = EDGE_CURVE ( 'NONE', #12016, #40648, #25520, .T. ) ;
#5791 = CARTESIAN_POINT ( 'NONE',  ( -22.94085434386056832, -9.802298134861713308, 70.19673941016031904 ) ) ;
#5792 = DIRECTION ( 'NONE',  ( -3.071710424422018668E-17, 6.404604876783312462E-16, 1.000000000000000000 ) ) ;
#5793 = CARTESIAN_POINT ( 'NONE',  ( -16.93941734680482725, -7.775588144984237005, 74.24546186738449194 ) ) ;
#5794 = ORIENTED_EDGE ( 'NONE', *, *, #47178, .T. ) ;
#5795 = LINE ( 'NONE', #20804, #21278 ) ;
#5796 = CARTESIAN_POINT ( 'NONE',  ( -17.42409385541299471, -14.80920654474435594, 52.02966884056656482 ) ) ;
#5797 = CARTESIAN_POINT ( 'NONE',  ( -11.07857809310684338, -11.73724795245126451, 71.38860870961248395 ) ) ;
#5798 = CARTESIAN_POINT ( 'NONE',  ( -12.18836193727821460, -19.53083876418623532, 57.94154444592973618 ) ) ;
#5799 = EDGE_CURVE ( 'NONE', #30955, #22574, #39954, .T. ) ;
#5800 = CARTESIAN_POINT ( 'NONE',  ( -20.12437885760196110, -7.865711196993452781, 73.76450701231766516 ) ) ;
#5801 = DIRECTION ( 'NONE',  ( 1.000000000000000000, -0.000000000000000000, 0.000000000000000000 ) ) ;
#5802 = AXIS2_PLACEMENT_3D ( 'NONE', #20502, #16782, #35016 ) ;
#5803 = ORIENTED_EDGE ( 'NONE', *, *, #48186, .T. ) ;
#5804 = LINE ( 'NONE', #9741, #18191 ) ;
#5805 = EDGE_CURVE ( 'NONE', #26444, #45257, #32114, .T. ) ;
#5806 = CARTESIAN_POINT ( 'NONE',  ( -14.23131808380166596, -8.077975302584915696, 67.45249250995216528 ) ) ;
#5807 = CARTESIAN_POINT ( 'NONE',  ( -24.32886716615087153, -16.23426984194678724, 62.60800820172418923 ) ) ;
#5808 = ORIENTED_EDGE ( 'NONE', *, *, #17494, .T. ) ;
#5809 = CARTESIAN_POINT ( 'NONE',  ( -15.22116837037893866, -21.50650591823945845, 68.59065000974109694 ) ) ;
#5810 = VERTEX_POINT ( 'NONE', #174 ) ;
#5811 = ORIENTED_EDGE ( 'NONE', *, *, #21811, .F. ) ;
#5812 = ORIENTED_EDGE ( 'NONE', *, *, #31229, .F. ) ;
#5813 = CARTESIAN_POINT ( 'NONE',  ( -24.93953149451673568, -10.04808947811604902, 53.49999999999995026 ) ) ;
#5814 = FACE_OUTER_BOUND ( 'NONE', #31126, .T. ) ;
#5815 = FACE_BOUND ( 'NONE', #47142, .T. ) ;
#5816 = EDGE_CURVE ( 'NONE', #39922, #15615, #2672, .T. ) ;
#5817 = CARTESIAN_POINT ( 'NONE',  ( -16.98831825750070479, -22.24652902502744922, 72.20897298418123000 ) ) ;
#5818 = ADVANCED_FACE ( 'NONE', ( #48656 ), #29756, .F. ) ;
#5819 = ORIENTED_EDGE ( 'NONE', *, *, #6876, .T. ) ;
#5820 = ORIENTED_EDGE ( 'NONE', *, *, #8265, .F. ) ;
#5821 = CARTESIAN_POINT ( 'NONE',  ( -18.16784385650552025, -6.428312510596451368, 51.20221977374900035 ) ) ;
#5822 = EDGE_CURVE ( 'NONE', #43599, #47374, #40781, .T. ) ;
#5823 = CARTESIAN_POINT ( 'NONE',  ( -24.87388367747922757, -14.87141420204137710, 59.43638527419312823 ) ) ;
#5824 = CARTESIAN_POINT ( 'NONE',  ( -24.05059659118241555, -17.06519001246171996, 72.88336032079776317 ) ) ;
#5825 = CARTESIAN_POINT ( 'NONE',  ( -21.09284385650551741, -7.406986770994973490, 48.81910596585309747 ) ) ;
#5826 = VECTOR ( 'NONE', #15511, 1000.000000000000000 ) ;
#5827 = VERTEX_POINT ( 'NONE', #40306 ) ;
#5828 = CARTESIAN_POINT ( 'NONE',  ( -12.43365403769799826, -9.824193568099090612, 60.85918061814654578 ) ) ;
#5829 = DIRECTION ( 'NONE',  ( 1.184681381641773627E-05, 1.827615834487727850E-06, -0.9999999999281563579 ) ) ;
#5830 = AXIS2_PLACEMENT_3D ( 'NONE', #106, #48112, #25696 ) ;
#5831 = FACE_OUTER_BOUND ( 'NONE', #36770, .T. ) ;
#5832 = VERTEX_POINT ( 'NONE', #21595 ) ;
#5833 = CARTESIAN_POINT ( 'NONE',  ( -14.98927377128279304, -8.246306944878790901, 47.99999999999994316 ) ) ;
#5834 = DIRECTION ( 'NONE',  ( -0.4599824152910791941, -0.8879280250239794947, -2.250728351766169940E-08 ) ) ;
#5835 = LINE ( 'NONE', #20846, #38331 ) ;
#5836 = CARTESIAN_POINT ( 'NONE',  ( -14.41428173599358331, -7.994163662063686893, 63.97474278339937115 ) ) ;
#5837 = ORIENTED_EDGE ( 'NONE', *, *, #4262, .F. ) ;
#5838 = CARTESIAN_POINT ( 'NONE',  ( -19.85890256509918572, -21.37233786973231275, 68.95612130754568625 ) ) ;
#5839 = DIRECTION ( 'NONE',  ( -1.000000000000000000, 4.164305804376849172E-17, -1.614929280266638808E-16 ) ) ;
#5840 = CARTESIAN_POINT ( 'NONE',  ( -20.59270190486383356, -18.27842527154038521, 49.52966884056656482 ) ) ;
#5841 = ORIENTED_EDGE ( 'NONE', *, *, #2705, .F. ) ;
#5842 = CARTESIAN_POINT ( 'NONE',  ( -13.17588093101833557, -17.89387621085224822, 49.52966884056656482 ) ) ;
#5843 = ORIENTED_EDGE ( 'NONE', *, *, #20324, .T. ) ;
#5844 = CARTESIAN_POINT ( 'NONE',  ( -11.78701489841286332, -10.65889831958446976, 74.73884969804157663 ) ) ;
#5845 = DIRECTION ( 'NONE',  ( 3.071710424422018668E-17, -6.404604876783312462E-16, -1.000000000000000000 ) ) ;
#5847 = EDGE_CURVE ( 'NONE', #15076, #11000, #36576, .T. ) ;
#5846 = ORIENTED_EDGE ( 'NONE', *, *, #10170, .T. ) ;
#5848 = CARTESIAN_POINT ( 'NONE',  ( -17.42409385541300892, -14.80920654474439679, 47.99999999999994316 ) ) ;
#5849 = CARTESIAN_POINT ( 'NONE',  ( -10.40127108354264429, -12.32249413655887871, 57.51352655450988749 ) ) ;
#5850 = CARTESIAN_POINT ( 'NONE',  ( -17.08574859075978480, -7.366143556642608559, 74.14673579026420214 ) ) ;
#5851 = CARTESIAN_POINT ( 'NONE',  ( -36.42409385541304800, -8.109206544743658540, 50.50000000000030553 ) ) ;
#5852 = VERTEX_POINT ( 'NONE', #11977 ) ;
#5853 = FACE_OUTER_BOUND ( 'NONE', #793, .T. ) ;
#5854 = FACE_OUTER_BOUND ( 'NONE', #32632, .T. ) ;
#5855 =( BOUNDED_SURFACE ( )  B_SPLINE_SURFACE ( 3, 1, ( 
 ( #46425, #34594 ),
 ( #39019, #878 ),
 ( #4816, #46177 ),
 ( #34839, #5062 ),
 ( #35326, #20070 ),
 ( #35074, #12680 ),
 ( #47869, #17571 ) ),
 .UNSPECIFIED., .T., .F., .F. ) 
 B_SPLINE_SURFACE_WITH_KNOTS ( ( 4, 3, 4 ),
 ( 2, 2 ),
 ( 0.000000000000000000, 0.5000000000000000000, 1.000000000000000000 ),
 ( 0.000000000000000000, 1.000000000000000000 ),
 .UNSPECIFIED. ) 
 GEOMETRIC_REPRESENTATION_ITEM ( )  RATIONAL_B_SPLINE_SURFACE ( (
 ( 1.000000000000000000, 1.000000000000000000),
 ( 0.3333333333333335369, 0.3333333333333330373),
 ( 0.3333333333333335369, 0.3333333333333330373),
 ( 1.000000000000000000, 1.000000000000000000),
 ( 0.3333333333333333703, 0.3333333333333333703),
 ( 0.3333333333333333703, 0.3333333333333333703),
 ( 1.000000000000000000, 1.000000000000000000) ) ) 
 REPRESENTATION_ITEM ( '' )  SURFACE ( )  );
#5856 = ORIENTED_EDGE ( 'NONE', *, *, #13548, .T. ) ;
#5857 = CARTESIAN_POINT ( 'NONE',  ( -10.61052024580041930, -11.79586507274399310, 74.71873631039885311 ) ) ;
#5858 = AXIS2_PLACEMENT_3D ( 'NONE', #41718, #122, #15105 ) ;
#5859 = CARTESIAN_POINT ( 'NONE',  ( -12.13668540368383653, -10.14142895936130628, 60.44429485117178302 ) ) ;
#5860 = AXIS2_PLACEMENT_3D ( 'NONE', #953, #42073, #15951 ) ;
#5861 = VERTEX_POINT ( 'NONE', #9188 ) ;
#5862 = EDGE_LOOP ( 'NONE', ( #13480, #12073, #1278, #12309 ) ) ;
#5863 = CARTESIAN_POINT ( 'NONE',  ( -14.81833918149647822, -21.30619657749716112, 58.18120369631310496 ) ) ;
#5864 = LINE ( 'NONE', #39349, #24141 ) ;
#5865 = CARTESIAN_POINT ( 'NONE',  ( -19.96994565995125015, -21.32983830779690848, 72.70478737306767414 ) ) ;
#5866 = CARTESIAN_POINT ( 'NONE',  ( -17.46159385650551599, -9.295667164867525756, 49.30633214617472504 ) ) ;
#5867 = CARTESIAN_POINT ( 'NONE',  ( -24.45390269921422188, -14.27548703327989621, 69.65275280629234089 ) ) ;
#5868 = CARTESIAN_POINT ( 'NONE',  ( -19.55842747286782313, -21.47588638780701942, 62.18606779526226092 ) ) ;
#5869 = CARTESIAN_POINT ( 'NONE',  ( -12.29704640786070158, -19.57524266776748334, 57.92682366959790130 ) ) ;
#5870 = CARTESIAN_POINT ( 'NONE',  ( -11.14886767096676934, -11.58796814604482250, 64.14881821840825182 ) ) ;
#5871 =( BOUNDED_SURFACE ( )  B_SPLINE_SURFACE ( 3, 1, ( 
 ( #31396, #35077 ),
 ( #16364, #12917 ),
 ( #16109, #26978 ),
 ( #8274, #42967 ),
 ( #23290, #16609 ),
 ( #633, #1601 ),
 ( #27940, #39022 ) ),
 .UNSPECIFIED., .T., .F., .F. ) 
 B_SPLINE_SURFACE_WITH_KNOTS ( ( 4, 3, 4 ),
 ( 2, 2 ),
 ( 0.000000000000000000, 0.5000000000000000000, 1.000000000000000000 ),
 ( 0.000000000000000000, 1.000000000000000000 ),
 .UNSPECIFIED. ) 
 GEOMETRIC_REPRESENTATION_ITEM ( )  RATIONAL_B_SPLINE_SURFACE ( (
 ( 1.000000000000000000, 1.000000000000000000),
 ( 0.3333333333333335369, 0.3333333333333330373),
 ( 0.3333333333333335369, 0.3333333333333330373),
 ( 1.000000000000000000, 1.000000000000000000),
 ( 0.3333333333333333703, 0.3333333333333333703),
 ( 0.3333333333333333703, 0.3333333333333333703),
 ( 1.000000000000000000, 1.000000000000000000) ) ) 
 REPRESENTATION_ITEM ( '' )  SURFACE ( )  );
#5872 = EDGE_CURVE ( 'NONE', #44873, #34640, #34160, .T. ) ;
#5873 = CARTESIAN_POINT ( 'NONE',  ( -16.70460144941857195, -22.22450915091796020, 68.81843766967561749 ) ) ;
#5874 = VERTEX_POINT ( 'NONE', #24206 ) ;
#5875 = ORIENTED_EDGE ( 'NONE', *, *, #22439, .F. ) ;
#5876 = CARTESIAN_POINT ( 'NONE',  ( -18.83586040784625126, -7.494106175837369044, 70.48572642001049360 ) ) ;
#5877 = ADVANCED_FACE ( 'NONE', ( #26752 ), #41772, .T. ) ;
#5878 = EDGE_CURVE ( 'NONE', #29913, #1863, #8056, .T. ) ;
#5879 = DIRECTION ( 'NONE',  ( 1.000000000000000000, 0.000000000000000000, 0.000000000000000000 ) ) ;
#5880 = CARTESIAN_POINT ( 'NONE',  ( -22.01318819962695983, -20.09513598245419885, 58.83730921330041497 ) ) ;
#5881 = CARTESIAN_POINT ( 'NONE',  ( -41.15852941833841783, -25.10920654474410441, 56.99999999999997868 ) ) ;
#5882 = CARTESIAN_POINT ( 'NONE',  ( -20.36919052476639180, -21.22336078664356407, 58.78908032405391992 ) ) ;
#5883 = ORIENTED_EDGE ( 'NONE', *, *, #45298, .T. ) ;
#5884 = CARTESIAN_POINT ( 'NONE',  ( -20.10030308072983374, -21.76202485516048668, 72.51983413602351902 ) ) ;
#5885 = PLANE ( 'NONE',  #40255 ) ;
#5886 = CARTESIAN_POINT ( 'NONE',  ( -16.39156059917436181, -21.78318494029796781, 62.05568132351888977 ) ) ;
#5887 = CARTESIAN_POINT ( 'NONE',  ( -10.09291371782238045, -16.13494220690481384, 68.16263107114907882 ) ) ;
#5888 = ORIENTED_EDGE ( 'NONE', *, *, #45159, .T. ) ;
#5889 = CARTESIAN_POINT ( 'NONE',  ( -17.99631655628617466, -7.779455715877602984, 60.49549448422539655 ) ) ;
#5890 = EDGE_CURVE ( 'NONE', #2631, #18891, #10070, .T. ) ;
#5891 = AXIS2_PLACEMENT_3D ( 'NONE', #11367, #45611, #22959 ) ;
#5892 = SPHERICAL_SURFACE ( 'NONE', #12647, 4.000000000000000000 ) ;
#5893 = CARTESIAN_POINT ( 'NONE',  ( -17.35166681046315773, -7.759430071869731549, 67.31479834546361474 ) ) ;
#5894 = CARTESIAN_POINT ( 'NONE',  ( -11.13707727077725096, -10.81211843560235053, 57.31629078479772943 ) ) ;
#5895 = CARTESIAN_POINT ( 'NONE',  ( -16.06904454444675778, -7.890656075740461795, 63.67011029959335389 ) ) ;
#5896 = ORIENTED_EDGE ( 'NONE', *, *, #17120, .F. ) ;
#5897 = LINE ( 'NONE', #17920, #20475 ) ;
#5898 = VERTEX_POINT ( 'NONE', #30452 ) ;
#5899 = DIRECTION ( 'NONE',  ( -3.071710424422018668E-17, 6.404604876783312462E-16, 1.000000000000000000 ) ) ;
#5900 = CARTESIAN_POINT ( 'NONE',  ( -10.23808006521456093, -12.84309671393774721, 67.86115469475366524 ) ) ;
#5901 = ORIENTED_EDGE ( 'NONE', *, *, #12149, .T. ) ;
#5902 = CARTESIAN_POINT ( 'NONE',  ( -13.70551016122406018, -21.26485310498106429, 68.56286810530107800 ) ) ;
#5903 = CARTESIAN_POINT ( 'NONE',  ( -14.90534385650551918, -8.801233750844183135, 48.81488406609782515 ) ) ;
#5904 = EDGE_CURVE ( 'NONE', #32131, #5574, #7347, .T. ) ;
#5905 = ORIENTED_EDGE ( 'NONE', *, *, #7303, .F. ) ;
#5906 = CARTESIAN_POINT ( 'NONE',  ( -17.92189206272508883, -7.825646655266591090, 60.30890604785338382 ) ) ;
#5907 = CARTESIAN_POINT ( 'NONE',  ( -16.72330486927764426, -21.83230113783351101, 61.91134987066439521 ) ) ;
#5908 = ORIENTED_EDGE ( 'NONE', *, *, #48622, .T. ) ;
#5909 = PLANE ( 'NONE',  #16064 ) ;
#5910 = CARTESIAN_POINT ( 'NONE',  ( -41.66527032600129132, -14.80920654474410725, 69.07058823529411029 ) ) ;
#5911 = B_SPLINE_CURVE_WITH_KNOTS ( 'NONE', 3,
 ( #38560, #30951, #45963, #4848, #19867, #8792, #34865, #23809, #38810, #6537 ),
 .UNSPECIFIED., .F., .F.,
 ( 4, 2, 2, 2, 4 ),
 ( 0.000000000000000000, 0.2500000000000000000, 0.5000000000000000000, 0.7500000000000000000, 1.000000000000000000 ),
 .UNSPECIFIED. ) ;
#5912 = CARTESIAN_POINT ( 'NONE',  ( -12.93051514224950260, -9.376680094107033625, 71.14365550519747217 ) ) ;
#5913 = CARTESIAN_POINT ( 'NONE',  ( -17.42409385541299471, -14.80920654474435771, 49.52966884056655772 ) ) ;
#5914 = ORIENTED_EDGE ( 'NONE', *, *, #16358, .F. ) ;
#5915 = VERTEX_POINT ( 'NONE', #43159 ) ;
#5916 = CYLINDRICAL_SURFACE ( 'NONE', #2339, 0.1500000000000065448 ) ;
#5917 = CARTESIAN_POINT ( 'NONE',  ( -10.02995815481606634, -13.89786978184575794, 57.63320425522585566 ) ) ;
#5918 = ORIENTED_EDGE ( 'NONE', *, *, #41490, .T. ) ;
#5919 = LINE ( 'NONE', #21660, #48472 ) ;
#5920 = CARTESIAN_POINT ( 'NONE',  ( -21.99178500617274779, -9.439039195359631762, 59.72171213140594404 ) ) ;
#5921 = CARTESIAN_POINT ( 'NONE',  ( -18.78659385759798894, -7.222650657624104298, 49.61879703869476543 ) ) ;
#5922 = CARTESIAN_POINT ( 'NONE',  ( -10.42805625848568596, -15.04470190113622685, 74.90664863841101351 ) ) ;
#5923 = PLANE ( 'NONE',  #44000 ) ;
#5924 = CARTESIAN_POINT ( 'NONE',  ( -15.88442554950127139, -7.926310505211968227, 71.02478706424572863 ) ) ;
#5925 = AXIS2_PLACEMENT_3D ( 'NONE', #28273, #34981, #24596 ) ;
#5926 = ORIENTED_EDGE ( 'NONE', *, *, #10220, .F. ) ;
#5927 = CARTESIAN_POINT ( 'NONE',  ( -11.77169895589660698, -10.59578386207264700, 74.43885051664024388 ) ) ;
#5928 = ADVANCED_FACE ( 'NONE', ( #30696 ), #24116, .T. ) ;
#5929 = AXIS2_PLACEMENT_3D ( 'NONE', #23912, #16731, #46067 ) ;
#5930 = CARTESIAN_POINT ( 'NONE',  ( -24.87384330655416420, -14.87999779688033719, 59.35804910119406230 ) ) ;
#5931 = CARTESIAN_POINT ( 'NONE',  ( -19.42896492416523913, -21.56812594671148275, 61.99503644571810668 ) ) ;
#5932 = ORIENTED_EDGE ( 'NONE', *, *, #42350, .T. ) ;
#5933 = EDGE_CURVE ( 'NONE', #22219, #32319, #8280, .T. ) ;
#5934 = EDGE_CURVE ( 'NONE', #8273, #13357, #5597, .T. ) ;
#5935 = ORIENTED_EDGE ( 'NONE', *, *, #15590, .F. ) ;
#5936 = DIRECTION ( 'NONE',  ( 0.000000000000000000, 0.000000000000000000, 1.000000000000000000 ) ) ;
#5937 =( NAMED_UNIT ( * ) PLANE_ANGLE_UNIT ( ) SI_UNIT ( $, .RADIAN. ) );
#5938 = EDGE_CURVE ( 'NONE', #41531, #29759, #39461, .T. ) ;
#5939 = LINE ( 'NONE', #47314, #47305 ) ;
#5940 = SHAPE_REPRESENTATION ( 'Cylinder Alignment Washers', ( #29031 ), #10942 ) ;
#5941 = EDGE_CURVE ( 'NONE', #6262, #23858, #38451, .T. ) ;
#5942 = ORIENTED_EDGE ( 'NONE', *, *, #41610, .T. ) ;
#5943 = CARTESIAN_POINT ( 'NONE',  ( -17.42409385541299471, -14.80920654474435771, 49.52966884056655772 ) ) ;
#5944 = CARTESIAN_POINT ( 'NONE',  ( -18.46801905451614445, -7.836623195388688679, 74.12592262855558545 ) ) ;
#5945 = EDGE_CURVE ( 'NONE', #1365, #20228, #26985, .T. ) ;
#5946 = ORIENTED_EDGE ( 'NONE', *, *, #47317, .F. ) ;
#5947 = CARTESIAN_POINT ( 'NONE',  ( -10.92563986671175691, -18.45389586190763964, 57.99369949602996854 ) ) ;
#5948 = CARTESIAN_POINT ( 'NONE',  ( -17.84029764213619984, -21.79726099838181597, 62.15919343507878381 ) ) ;
#5949 = ORIENTED_EDGE ( 'NONE', *, *, #22285, .T. ) ;
#5950 = CARTESIAN_POINT ( 'NONE',  ( -22.33376602745314798, -19.86903051493498040, 69.18890041286789483 ) ) ;
#5951 = ORIENTED_EDGE ( 'NONE', *, *, #40609, .F. ) ;
#5952 = CARTESIAN_POINT ( 'NONE',  ( -13.47245400663725690, -21.12492667118925382, 65.10133491818508844 ) ) ;
#5953 = VECTOR ( 'NONE', #8014, 1000.000000000000000 ) ;
#5954 = ORIENTED_EDGE ( 'NONE', *, *, #40077, .F. ) ;
#5955 = DIRECTION ( 'NONE',  ( 0.9687793358424819923, -0.2479245821708678799, 3.596521012361014201E-17 ) ) ;
#5956 = CARTESIAN_POINT ( 'NONE',  ( -19.37616744185158879, -21.99900390342548206, 58.71002665166666645 ) ) ;
#5957 = ORIENTED_EDGE ( 'NONE', *, *, #9103, .F. ) ;
#5958 = DIRECTION ( 'NONE',  ( 0.000000000000000000, 0.000000000000000000, 1.000000000000000000 ) ) ;
#5959 = CYLINDRICAL_SURFACE ( 'NONE', #2982, 2.000000000000001776 ) ;
#5960 = DIRECTION ( 'NONE',  ( 0.8394943004421989707, -0.3114503813636536056, -0.4452504682462418151 ) ) ;
#5961 = DIRECTION ( 'NONE',  ( -0.5097212845717550289, 0.8603395911234820170, 0.000000000000000000 ) ) ;
#5962 = CARTESIAN_POINT ( 'NONE',  ( -21.06702863216100141, -20.84540773593991148, 65.86981821684420879 ) ) ;
#5963 = ORIENTED_EDGE ( 'NONE', *, *, #21393, .T. ) ;
#5964 = CARTESIAN_POINT ( 'NONE',  ( -11.68672781637937419, -10.05669048882576533, 67.68392176937598492 ) ) ;
#5965 = DIRECTION ( 'NONE',  ( -0.9441784275685842776, 0.3294345108122634369, 1.993146885055995131E-08 ) ) ;
#5966 = CARTESIAN_POINT ( 'NONE',  ( -13.16557854728010746, -20.92211907906095547, 58.14626439336120711 ) ) ;
#5967 = CARTESIAN_POINT ( 'NONE',  ( -27.42409385541305156, -15.80920654474410725, 74.99999999999998579 ) ) ;
#5968 = CARTESIAN_POINT ( 'NONE',  ( -14.03034385650551563, -9.794322478646142471, 51.19202720610083190 ) ) ;
#5969 = ORIENTED_EDGE ( 'NONE', *, *, #22653, .F. ) ;
#5970 = DIRECTION ( 'NONE',  ( 0.000000000000000000, 0.000000000000000000, 1.000000000000000000 ) ) ;
#5971 = CARTESIAN_POINT ( 'NONE',  ( -22.51726247777427758, -19.68384842258191370, 72.94400547081133368 ) ) ;
#5972 = ORIENTED_EDGE ( 'NONE', *, *, #20383, .T. ) ;
#5973 = CARTESIAN_POINT ( 'NONE',  ( -10.37821464302998109, -14.49231327520767465, 71.74271303568544056 ) ) ;
#5974 = LINE ( 'NONE', #13821, #8593 ) ;
#5975 = PLANE ( 'NONE',  #5094 ) ;
#5976 = CARTESIAN_POINT ( 'NONE',  ( -15.42641777070416609, -21.57041088783041971, 72.05135256464748750 ) ) ;
#5977 = ADVANCED_FACE ( 'NONE', ( #20263 ), #35270, .T. ) ;
#5978 = ORIENTED_EDGE ( 'NONE', *, *, #27278, .T. ) ;
#5979 = CARTESIAN_POINT ( 'NONE',  ( -23.88506645939990847, -17.50400960575725406, 66.22740630230595116 ) ) ;
#5980 = DIRECTION ( 'NONE',  ( 0.8839923186919886877, -0.4675014229855999348, 2.842058574697910628E-08 ) ) ;
#5981 = CARTESIAN_POINT ( 'NONE',  ( -23.74125355947768767, -17.82500418272770659, 59.30378426403790115 ) ) ;
#5982 = ADVANCED_FACE ( 'NONE', ( #17522 ), #40653, .T. ) ;
#5983 = ORIENTED_EDGE ( 'NONE', *, *, #34771, .T. ) ;
#5984 = CYLINDRICAL_SURFACE ( 'NONE', #23540, 1.250000000000001110 ) ;
#5985 = DIRECTION ( 'NONE',  ( -2.662580024931131981E-06, 1.091441817331640981E-05, -0.9999999999368931469 ) ) ;
#5986 = CARTESIAN_POINT ( 'NONE',  ( -23.44004476468150600, -11.23011772834392730, 73.66193342791716248 ) ) ;
#5987 = CARTESIAN_POINT ( 'NONE',  ( -24.15927579118118373, -17.99354550443843692, 59.10404166857890829 ) ) ;
#5988 =( BOUNDED_SURFACE ( )  B_SPLINE_SURFACE ( 3, 1, ( 
 ( #46746, #38865 ),
 ( #4653, #12517 ),
 ( #5142, #42809 ),
 ( #27780, #24095 ),
 ( #12989, #28017 ),
 ( #34922, #5638 ),
 ( #35640, #31959 ) ),
 .UNSPECIFIED., .T., .F., .F. ) 
 B_SPLINE_SURFACE_WITH_KNOTS ( ( 4, 3, 4 ),
 ( 2, 2 ),
 ( 0.000000000000000000, 0.5000000000000000000, 1.000000000000000000 ),
 ( 0.000000000000000000, 1.000000000000000000 ),
 .UNSPECIFIED. ) 
 GEOMETRIC_REPRESENTATION_ITEM ( )  RATIONAL_B_SPLINE_SURFACE ( (
 ( 1.000000000000000000, 1.000000000000000000),
 ( 0.3333333333333335369, 0.3333333333333330373),
 ( 0.3333333333333335369, 0.3333333333333330373),
 ( 1.000000000000000000, 1.000000000000000000),
 ( 0.3333333333333333703, 0.3333333333333333703),
 ( 0.3333333333333333703, 0.3333333333333333703),
 ( 1.000000000000000000, 1.000000000000000000) ) ) 
 REPRESENTATION_ITEM ( '' )  SURFACE ( )  );
#5989 = FACE_OUTER_BOUND ( 'NONE', #14351, .T. ) ;
#5990 = CARTESIAN_POINT ( 'NONE',  ( -17.42409385541300892, -14.80920654474439502, 75.49999999999994316 ) ) ;
#5991 = VERTEX_POINT ( 'NONE', #25638 ) ;
#5992 = AXIS2_PLACEMENT_3D ( 'NONE', #20121, #30497, #38586 ) ;
#5993 = ORIENTED_EDGE ( 'NONE', *, *, #28984, .T. ) ;
#5994 = AXIS2_PLACEMENT_3D ( 'NONE', #15546, #4253, #19262 ) ;
#5995 = CARTESIAN_POINT ( 'NONE',  ( -17.85534385541304303, -8.623186033802570094, 49.24843789510466507 ) ) ;
#5996 = CARTESIAN_POINT ( 'NONE',  ( -13.27361356051800456, -9.172254427053855963, 63.90946478016504528 ) ) ;
#5997 = ADVANCED_FACE ( 'NONE', ( #28620 ), #43414, .T. ) ;
#5998 = CARTESIAN_POINT ( 'NONE',  ( -14.10256395084115866, -8.140532207465255965, 70.84462205307964666 ) ) ;
#5999 = EDGE_CURVE ( 'NONE', #16677, #19285, #38387, .T. ) ;
#6000 =( BOUNDED_CURVE ( )  B_SPLINE_CURVE ( 3, ( #34237, #15028, #11854, #22697 ),
 .UNSPECIFIED., .F., .F. ) 
 B_SPLINE_CURVE_WITH_KNOTS ( ( 4, 4 ),
 ( 0.9074455897393707282, 1.000000000000000000 ),
 .UNSPECIFIED. ) 
 CURVE ( )  GEOMETRIC_REPRESENTATION_ITEM ( )  RATIONAL_B_SPLINE_CURVE ( ( 0.6983129098261133816, 0.7760317562607157438, 0.8765941196520112833, 1.000000000000000000 ) ) 
 REPRESENTATION_ITEM ( '' )  );
#6001 = DIRECTION ( 'NONE',  ( 3.413470714839332458E-33, -1.190614954331866791E-16, 1.000000000000000000 ) ) ;
#6002 = ORIENTED_EDGE ( 'NONE', *, *, #38018, .T. ) ;
#6003 = CARTESIAN_POINT ( 'NONE',  ( -21.10139403845883876, -20.76557291098659164, 65.65741929463816007 ) ) ;
#6004 = DIRECTION ( 'NONE',  ( 0.000000000000000000, 0.000000000000000000, 1.000000000000000000 ) ) ;
#6005 = EDGE_CURVE ( 'NONE', #35820, #17561, #36947, .T. ) ;
#6006 = ORIENTED_EDGE ( 'NONE', *, *, #9217, .T. ) ;
#6007 = CARTESIAN_POINT ( 'NONE',  ( -24.41887989321793739, -14.52796132729743839, 66.19909327358298867 ) ) ;
#6008 = FACE_OUTER_BOUND ( 'NONE', #9653, .T. ) ;
#6009 =( BOUNDED_SURFACE ( )  B_SPLINE_SURFACE ( 3, 1, ( 
 ( #20104, #5095 ),
 ( #35111, #1378 ),
 ( #16397, #31425 ),
 ( #30637, #4513 ),
 ( #1064, #15575 ),
 ( #12383, #4047 ),
 ( #27406, #38228 ) ),
 .UNSPECIFIED., .T., .F., .F. ) 
 B_SPLINE_SURFACE_WITH_KNOTS ( ( 4, 3, 4 ),
 ( 2, 2 ),
 ( 0.000000000000000000, 0.5000000000000000000, 1.000000000000000000 ),
 ( 0.000000000000000000, 1.000000000000000000 ),
 .UNSPECIFIED. ) 
 GEOMETRIC_REPRESENTATION_ITEM ( )  RATIONAL_B_SPLINE_SURFACE ( (
 ( 1.000000000000000000, 1.000000000000000000),
 ( 0.3333333333333335369, 0.3333333333333330373),
 ( 0.3333333333333335369, 0.3333333333333330373),
 ( 1.000000000000000000, 1.000000000000000000),
 ( 0.3333333333333333703, 0.3333333333333333703),
 ( 0.3333333333333333703, 0.3333333333333333703),
 ( 1.000000000000000000, 1.000000000000000000) ) ) 
 REPRESENTATION_ITEM ( '' )  SURFACE ( )  );
#6010 = ORIENTED_EDGE ( 'NONE', *, *, #961, .F. ) ;
#6011 = DIRECTION ( 'NONE',  ( 1.000000000000000000, -0.000000000000000000, -2.406186529621654511E-16 ) ) ;
#6012 = FACE_OUTER_BOUND ( 'NONE', #47417, .T. ) ;
#6013 = ORIENTED_EDGE ( 'NONE', *, *, #12947, .F. ) ;
#6014 = DIRECTION ( 'NONE',  ( -0.000000000000000000, -1.000000000000000000, -0.000000000000000000 ) ) ;
#6015 = CARTESIAN_POINT ( 'NONE',  ( -17.92409385541305511, -14.80920654474410725, 47.99999999999998579 ) ) ;
#6016 = DIRECTION ( 'NONE',  ( -2.866981220435666553E-17, 1.000000000000000000, 1.190614954331866791E-16 ) ) ;
#6017 = CARTESIAN_POINT ( 'NONE',  ( -24.70004435018021383, -13.20802528152527877, 59.46929592674912612 ) ) ;
#6018 = EDGE_LOOP ( 'NONE', ( #2379, #40890, #14152, #35053 ) ) ;
#6019 = CARTESIAN_POINT ( 'NONE',  ( -14.41058011727219501, -8.490943137660508455, 67.55975084671482023 ) ) ;
#6020 = DIRECTION ( 'NONE',  ( 3.071710424422018668E-17, -6.404604876783312462E-16, -1.000000000000000000 ) ) ;
#6021 = DIRECTION ( 'NONE',  ( 0.6771828760946864145, -0.7358147540815750398, 3.419290845356542170E-09 ) ) ;
#6022 = VECTOR ( 'NONE', #22957, 1000.000000000000000 ) ;
#6023 = VECTOR ( 'NONE', #5344, 1000.000000000000000 ) ;
#6024 = PLANE ( 'NONE',  #6929 ) ;
#6025 = CARTESIAN_POINT ( 'NONE',  ( -20.12289122552838094, -7.865124802246414859, 73.90591932823114973 ) ) ;
#6026 = CYLINDRICAL_SURFACE ( 'NONE', #9766, 0.1499999999999963862 ) ;
#6027 = DIRECTION ( 'NONE',  ( -2.866981220435666553E-17, 1.000000000000000000, 1.190614954331866791E-16 ) ) ;
#6028 = DIRECTION ( 'NONE',  ( 3.071710424422018668E-17, -6.404604876783312462E-16, -1.000000000000000000 ) ) ;
#6029 = ORIENTED_EDGE ( 'NONE', *, *, #22622, .F. ) ;
#6030 = FACE_OUTER_BOUND ( 'NONE', #41333, .T. ) ;
#6031 = CARTESIAN_POINT ( 'NONE',  ( -16.55451525393793233, -12.46531383050667863, 77.49999999999994316 ) ) ;
#6032 = CARTESIAN_POINT ( 'NONE',  ( -13.34910288913403065, -20.50135726297604677, 58.06266769909647962 ) ) ;
#6033 = EDGE_CURVE ( 'NONE', #35489, #22569, #22660, .T. ) ;
#6034 = ORIENTED_EDGE ( 'NONE', *, *, #1284, .F. ) ;
#6035 = CARTESIAN_POINT ( 'NONE',  ( -19.48731947536727915, -21.55887828695198039, 69.07915298548451233 ) ) ;
#6036 = ORIENTED_EDGE ( 'NONE', *, *, #23706, .T. ) ;
#6037 = ORIENTED_EDGE ( 'NONE', *, *, #47973, .F. ) ;
#6038 = ORIENTED_EDGE ( 'NONE', *, *, #824, .F. ) ;
#6039 = CARTESIAN_POINT ( 'NONE',  ( -10.03202132150386383, -15.73778161007442833, 61.17642517804716817 ) ) ;
#6040 = CARTESIAN_POINT ( 'NONE',  ( -23.11919578175225354, -18.88151874835563859, 66.05219398271668751 ) ) ;
#6041 = CARTESIAN_POINT ( 'NONE',  ( -15.94639903137639791, -7.966892978607620357, 63.74298973210061803 ) ) ;
#6042 = FACE_OUTER_BOUND ( 'NONE', #16859, .T. ) ;
#6043 = VERTEX_POINT ( 'NONE', #43651 ) ;
#6044 = ORIENTED_EDGE ( 'NONE', *, *, #1616, .F. ) ;
#6045 = CARTESIAN_POINT ( 'NONE',  ( -20.19284385650551528, -7.406986770994973490, 48.81910596585309747 ) ) ;
#6046 = EDGE_CURVE ( 'NONE', #10797, #43519, #32862, .T. ) ;
#6047 = CARTESIAN_POINT ( 'NONE',  ( -20.66122932390920752, -21.07544863110783950, 62.52960166509647166 ) ) ;
#6048 = CARTESIAN_POINT ( 'NONE',  ( -24.09731288006578609, -16.92300596032393045, 72.99222104724324822 ) ) ;
#6049 = ADVANCED_FACE ( 'NONE', ( #36467 ), #46116, .T. ) ;
#6050 = CARTESIAN_POINT ( 'NONE',  ( -17.54909385650551812, -8.104110260919579645, 48.81699501597546487 ) ) ;
#6051 = VECTOR ( 'NONE', #19863, 1000.000000000000000 ) ;
#6052 = CIRCLE ( 'NONE', #33551, 2.000000000000001332 ) ;
#6053 = ORIENTED_EDGE ( 'NONE', *, *, #10371, .T. ) ;
#6054 = ADVANCED_FACE ( 'NONE', ( #40188 ), #6460, .T. ) ;
#6055 = CARTESIAN_POINT ( 'NONE',  ( -24.80769047312930553, -15.80232199467591947, 69.71802767292497549 ) ) ;
#6056 = EDGE_CURVE ( 'NONE', #35176, #14422, #2271, .T. ) ;
#6057 = AXIS2_PLACEMENT_3D ( 'NONE', #40460, #21526, #36506 ) ;
#6058 = ORIENTED_EDGE ( 'NONE', *, *, #1641, .T. ) ;
#6059 = CARTESIAN_POINT ( 'NONE',  ( -11.27324661094954550, -11.46480969376360726, 67.84694496584526746 ) ) ;
#6060 = B_SPLINE_CURVE_WITH_KNOTS ( 'NONE', 3,
 ( #8433, #23461, #16281, #38461, #9411, #19768, #31321, #35245, #5226, #4745 ),
 .UNSPECIFIED., .F., .F.,
 ( 4, 2, 2, 2, 4 ),
 ( 0.000000000000000000, 0.2500000000000000000, 0.5000000000000000000, 0.7500000000000000000, 1.000000000000000000 ),
 .UNSPECIFIED. ) ;
#6061 = ORIENTED_EDGE ( 'NONE', *, *, #46657, .F. ) ;
#6062 = B_SPLINE_CURVE_WITH_KNOTS ( 'NONE', 3,
 ( #40157, #21681, #6900, #36664, #20958, #2949, #25607, #17961, #32980, #48023 ),
 .UNSPECIFIED., .F., .F.,
 ( 4, 2, 2, 2, 4 ),
 ( 0.6272669072976775340, 0.7522669073147194574, 0.8772669073317613808, 1.002266907348803304, 1.127266907365845228 ),
 .UNSPECIFIED. ) ;
#6063 = DIRECTION ( 'NONE',  ( -1.702402328345533783E-17, 7.068183862238070054E-18, -1.000000000000000000 ) ) ;
#6064 = CARTESIAN_POINT ( 'NONE',  ( -22.07805708657739885, -20.69058616546009333, 47.99999999999994316 ) ) ;
#6065 = CARTESIAN_POINT ( 'NONE',  ( -14.47983227664519212, -7.965588925009814858, 63.90483403727078837 ) ) ;
#6066 = ORIENTED_EDGE ( 'NONE', *, *, #18573, .T. ) ;
#6067 = LINE ( 'NONE', #44008, #30542 ) ;
#6068 = EDGE_CURVE ( 'NONE', #26756, #32237, #30286, .T. ) ;
#6069 = CARTESIAN_POINT ( 'NONE',  ( -17.01159385541303593, -8.990409506049202193, 49.61344411288074951 ) ) ;
#6070 = DIRECTION ( 'NONE',  ( -0.8459089628457129306, -0.5333273165489313961, 7.771812504399799980E-08 ) ) ;
#6071 = VERTEX_POINT ( 'NONE', #29341 ) ;
#6072 = FACE_OUTER_BOUND ( 'NONE', #18946, .T. ) ;
#6073 = ADVANCED_FACE ( 'NONE', ( #2985 ), #17994, .T. ) ;
#6074 = ORIENTED_EDGE ( 'NONE', *, *, #14584, .F. ) ;
#6075 = CARTESIAN_POINT ( 'NONE',  ( -24.40658474706614101, -15.78251040532600769, 69.68307488409816131 ) ) ;
#6076 = CARTESIAN_POINT ( 'NONE',  ( -16.25049871934676204, -21.71175505818405682, 61.86641321701562646 ) ) ;
#6077 = ORIENTED_EDGE ( 'NONE', *, *, #6521, .T. ) ;
#6078 = CARTESIAN_POINT ( 'NONE',  ( -13.17786431350945797, -8.687616865786688791, 60.56137482248813342 ) ) ;
#6079 = CARTESIAN_POINT ( 'NONE',  ( -24.11881394502254849, -17.01995806294775448, 73.16863963025599560 ) ) ;
#6080 = CARTESIAN_POINT ( 'NONE',  ( -13.49267557974227394, -8.956801037788498121, 60.45422421514565059 ) ) ;
#6081 = CYLINDRICAL_SURFACE ( 'NONE', #45558, 0.1500000000000007716 ) ;
#6082 = EDGE_LOOP ( 'NONE', ( #4939, #15803 ) ) ;
#6083 = CARTESIAN_POINT ( 'NONE',  ( -14.96223302779666398, -10.63593772014186101, 52.02966884056656482 ) ) ;
#6084 = UNCERTAINTY_MEASURE_WITH_UNIT (LENGTH_MEASURE( 1.000000000000000082E-05 ), #6365, 'distance_accuracy_value', 'NONE');
#6085 = CARTESIAN_POINT ( 'NONE',  ( -23.80338573481879294, -11.80731802715296119, 59.76763678108634537 ) ) ;
#6086 = B_SPLINE_CURVE_WITH_KNOTS ( 'NONE', 3,
 ( #40261, #21546, #36529, #26206, #23017, #33314, #11420, #34064, #48354, #40979 ),
 .UNSPECIFIED., .F., .F.,
 ( 4, 2, 2, 2, 4 ),
 ( 0.000000000000000000, 0.2500000000000000000, 0.5000000000000000000, 0.7500000000000000000, 1.000000000000000000 ),
 .UNSPECIFIED. ) ;
#6087 = ADVANCED_FACE ( 'NONE', ( #48530 ), #29581, .T. ) ;
#6088 = CARTESIAN_POINT ( 'NONE',  ( -16.54207536886490004, -21.80396438979022022, 65.23124200709338538 ) ) ;
#6089 = EDGE_LOOP ( 'NONE', ( #8115, #16826, #33797, #30175 ) ) ;
#6090 = CARTESIAN_POINT ( 'NONE',  ( -11.18274741528775884, -18.87723868614961731, 64.85432942596317218 ) ) ;
#6091 = AXIS2_PLACEMENT_3D ( 'NONE', #22162, #17713, #48013 ) ;
#6092 = CARTESIAN_POINT ( 'NONE',  ( -12.23301264461619553, -10.03852782535897958, 60.84446034103241630 ) ) ;
#6093 = VERTEX_POINT ( 'NONE', #22949 ) ;
#6094 = VERTEX_POINT ( 'NONE', #45601 ) ;
#6095 = CARTESIAN_POINT ( 'NONE',  ( -24.43112999227502513, -15.58634490091466951, 73.00303748142292193 ) ) ;
#6096 = DIRECTION ( 'NONE',  ( 0.9687793358424821033, -0.2479245821708677133, 0.000000000000000000 ) ) ;
#6097 = DIRECTION ( 'NONE',  ( 0.9687793358424804380, -0.2479245821708741804, 0.000000000000000000 ) ) ;
#6098 = AXIS2_PLACEMENT_3D ( 'NONE', #35627, #43027, #47688 ) ;
#6099 = CARTESIAN_POINT ( 'NONE',  ( -17.74284385650551599, -8.811426318492348031, 52.18089403414751359 ) ) ;
#6100 = LINE ( 'NONE', #2409, #28203 ) ;
#6101 = CARTESIAN_POINT ( 'NONE',  ( -10.40689392953442294, -15.49001398589273393, 57.86233024654485035 ) ) ;
#6102 = CARTESIAN_POINT ( 'NONE',  ( -12.40380818233537141, -19.68739593843253033, 61.69678633575567517 ) ) ;
#6103 = CARTESIAN_POINT ( 'NONE',  ( -14.92409385541306044, -14.80920654474411080, 75.49999999999998579 ) ) ;
#6104 = CARTESIAN_POINT ( 'NONE',  ( -13.90002763284361365, -21.37314463245085250, 72.04794927803091298 ) ) ;
#6105 = EDGE_LOOP ( 'NONE', ( #42446, #33619, #41323, #21958, #39428 ) ) ;
#6106 = VERTEX_POINT ( 'NONE', #25889 ) ;
#6107 = CARTESIAN_POINT ( 'NONE',  ( -24.35094580881710513, -16.14095786638556973, 59.12332159045481461 ) ) ;
#6108 = B_SPLINE_CURVE_WITH_KNOTS ( 'NONE', 1,
 ( #43125, #24421 ),
 .UNSPECIFIED., .F., .F.,
 ( 2, 2 ),
 ( 0.000000000000000000, 1.000000000000000000 ),
 .UNSPECIFIED. ) ;
#6109 = DIRECTION ( 'NONE',  ( 0.3688590060343583388, -0.9294853595766559007, 0.000000000000000000 ) ) ;
#6110 = CARTESIAN_POINT ( 'NONE',  ( -17.50221816081645798, -7.047512361584055363, 53.27966884056655061 ) ) ;
#6111 = CARTESIAN_POINT ( 'NONE',  ( -12.43058792219793141, -16.43013174195301218, 49.52966884056655772 ) ) ;
#6112 = DIRECTION ( 'NONE',  ( 0.07061531369766044230, 0.9975036227860933913, 1.268851335910971019E-08 ) ) ;
#6113 = B_SPLINE_CURVE_WITH_KNOTS ( 'NONE', 3,
 ( #27177, #16071, #19800, #35280, #31114, #35035, #34551, #38234, #12875, #12159 ),
 .UNSPECIFIED., .F., .F.,
 ( 4, 2, 2, 2, 4 ),
 ( 0.1272669073658370675, 0.2522669073488581493, 0.3772669073318791755, 0.5022669073149002017, 0.6272669072979213389 ),
 .UNSPECIFIED. ) ;
#6114 = CARTESIAN_POINT ( 'NONE',  ( -20.44284385650551883, -8.811426318492348031, 52.18089403414751359 ) ) ;
#6115 = ORIENTED_EDGE ( 'NONE', *, *, #27796, .F. ) ;
#6116 = EDGE_CURVE ( 'NONE', #38445, #41647, #11120, .T. ) ;
#6117 = CARTESIAN_POINT ( 'NONE',  ( -23.58616520728616806, -18.99640775243969060, 66.00884813586510802 ) ) ;
#6118 = LINE ( 'NONE', #2428, #31611 ) ;
#6119 = APPLICATION_CONTEXT ( 'automotive_design' ) ;
#6120 = EDGE_CURVE ( 'NONE', #24736, #45017, #14734, .T. ) ;
#6121 = AXIS2_PLACEMENT_3D ( 'NONE', #21531, #40466, #37237 ) ;
#6122 = DIRECTION ( 'NONE',  ( -3.071710424422018668E-17, 6.404604876783312462E-16, 1.000000000000000000 ) ) ;
#6123 = ORIENTED_EDGE ( 'NONE', *, *, #1705, .T. ) ;
#6124 = CIRCLE ( 'NONE', #11613, 4.686499999999997890 ) ;
#6125 = VECTOR ( 'NONE', #33862, 1000.000000000000000 ) ;
#6126 = CYLINDRICAL_SURFACE ( 'NONE', #42444, 0.1499999999999948874 ) ;
#6127 = CARTESIAN_POINT ( 'NONE',  ( -12.74585782473854145, -9.602005322742989790, 74.39210991189573008 ) ) ;
#6128 = AXIS2_PLACEMENT_3D ( 'NONE', #1738, #27590, #16004 ) ;
#6129 = CARTESIAN_POINT ( 'NONE',  ( -24.59706333651279664, -12.79617740830267891, 66.48742133194130588 ) ) ;
#6130 =( BOUNDED_SURFACE ( )  B_SPLINE_SURFACE ( 3, 1, ( 
 ( #42424, #27388 ),
 ( #1048, #31324 ),
 ( #24185, #27868 ),
 ( #38210, #42668 ),
 ( #20006, #8693 ),
 ( #16044, #46355 ),
 ( #35248, #46105 ) ),
 .UNSPECIFIED., .T., .F., .F. ) 
 B_SPLINE_SURFACE_WITH_KNOTS ( ( 4, 3, 4 ),
 ( 2, 2 ),
 ( 0.000000000000000000, 0.5000000000000000000, 1.000000000000000000 ),
 ( 0.000000000000000000, 1.000000000000000000 ),
 .UNSPECIFIED. ) 
 GEOMETRIC_REPRESENTATION_ITEM ( )  RATIONAL_B_SPLINE_SURFACE ( (
 ( 1.000000000000000000, 1.000000000000000000),
 ( 0.3333333333333335369, 0.3333333333333330373),
 ( 0.3333333333333335369, 0.3333333333333330373),
 ( 1.000000000000000000, 1.000000000000000000),
 ( 0.3333333333333333703, 0.3333333333333333703),
 ( 0.3333333333333333703, 0.3333333333333333703),
 ( 1.000000000000000000, 1.000000000000000000) ) ) 
 REPRESENTATION_ITEM ( '' )  SURFACE ( )  );
#6131 = ADVANCED_FACE ( 'NONE', ( #44863 ), #11851, .T. ) ;
#6132 = CARTESIAN_POINT ( 'NONE',  ( -16.19792114999740562, -7.866354181730329742, 60.48556343814865954 ) ) ;
#6133 = VERTEX_POINT ( 'NONE', #3726 ) ;
#6134 = DIRECTION ( 'NONE',  ( -3.071710424422018668E-17, 6.404604876783312462E-16, 1.000000000000000000 ) ) ;
#6135 = AXIS2_PLACEMENT_3D ( 'NONE', #12096, #8897, #16010 ) ;
#6136 = EDGE_CURVE ( 'NONE', #13199, #20304, #36031, .T. ) ;
#6137 = ORIENTED_EDGE ( 'NONE', *, *, #7030, .T. ) ;
#6138 = CARTESIAN_POINT ( 'NONE',  ( -23.83043763270304183, -11.86620476845630101, 59.48235732590898550 ) ) ;
#6139 = CARTESIAN_POINT ( 'NONE',  ( -10.21961014573118121, -12.91218125089532265, 67.93106486834143709 ) ) ;
#6140 = VERTEX_POINT ( 'NONE', #7433 ) ;
#6141 = ADVANCED_FACE ( 'NONE', ( #521, #14519 ), #22440, .T. ) ;
#6142 = ADVANCED_FACE ( 'NONE', ( #37431 ), #37938, .T. ) ;
#6143 = EDGE_CURVE ( 'NONE', #39245, #46590, #31309, .T. ) ;
#6144 = PLANE ( 'NONE',  #28171 ) ;
#6145 = CARTESIAN_POINT ( 'NONE',  ( -12.74836358285320159, -20.08597126951521261, 71.82125749157572159 ) ) ;
#6146 = ORIENTED_EDGE ( 'NONE', *, *, #41113, .F. ) ;
#6147 = DIRECTION ( 'NONE',  ( -2.866981220435666553E-17, 1.000000000000000000, 1.190614954331866791E-16 ) ) ;
#6148 = FACE_OUTER_BOUND ( 'NONE', #14736, .T. ) ;
#6149 = CARTESIAN_POINT ( 'NONE',  ( -14.97035482569482312, -21.41873484682592377, 61.92128389535452015 ) ) ;
#6150 = EDGE_LOOP ( 'NONE', ( #26876, #22920 ) ) ;
#6151 = CARTESIAN_POINT ( 'NONE',  ( -18.16355857556227349, -7.327338257757846307, 53.76227901944321985 ) ) ;
#6152 =( BOUNDED_CURVE ( )  B_SPLINE_CURVE ( 3, ( #43395, #1778, #24439, #20733 ),
 .UNSPECIFIED., .F., .F. ) 
 B_SPLINE_CURVE_WITH_KNOTS ( ( 4, 4 ),
 ( 0.9074455897393637338, 1.000000000000000000 ),
 .UNSPECIFIED. ) 
 CURVE ( )  GEOMETRIC_REPRESENTATION_ITEM ( )  RATIONAL_B_SPLINE_CURVE ( ( 0.6983129098260837386, 0.7760317562606902086, 0.8765941196519956291, 1.000000000000000000 ) ) 
 REPRESENTATION_ITEM ( '' )  );
#6153 = CARTESIAN_POINT ( 'NONE',  ( -10.96500202619968256, -18.52180277100054795, 58.00052909868417572 ) ) ;
#6154 = CARTESIAN_POINT ( 'NONE',  ( -12.00560918470589122, -10.37740546741846615, 67.51399311695257666 ) ) ;
#6155 = CARTESIAN_POINT ( 'NONE',  ( -26.42409385541305511, -15.80920654474410725, 47.99999999999997868 ) ) ;
#6156 = EDGE_LOOP ( 'NONE', ( #35115, #39314, #34346, #11811, #10661 ) ) ;
#6157 = ORIENTED_EDGE ( 'NONE', *, *, #31153, .F. ) ;
#6158 = DIRECTION ( 'NONE',  ( 2.117869074558178593E-07, 2.255668799892331646E-07, 0.9999999999999520384 ) ) ;
#6159 = CARTESIAN_POINT ( 'NONE',  ( -24.30032712313099807, -16.12036388816417798, 62.89328623440644606 ) ) ;
#6160 = ORIENTED_EDGE ( 'NONE', *, *, #9830, .F. ) ;
#6161 = CARTESIAN_POINT ( 'NONE',  ( -17.00410623003636346, -7.771727578618798482, 74.11018273220987851 ) ) ;
#6162 = CARTESIAN_POINT ( 'NONE',  ( -20.19284385759799605, -8.630756214087126565, 51.74842643355248129 ) ) ;
#6163 = CARTESIAN_POINT ( 'NONE',  ( -15.85230412793554144, -7.936612759385449856, 67.44007248260970755 ) ) ;
#6164 = AXIS2_PLACEMENT_3D ( 'NONE', #3991, #15282, #8178 ) ;
#6165 = PLANE ( 'NONE',  #750 ) ;
#6166 = CARTESIAN_POINT ( 'NONE',  ( -20.58582848812473642, -8.063211782720200560, 66.92070701425123502 ) ) ;
#6167 = AXIS2_PLACEMENT_3D ( 'NONE', #27403, #42438, #8708 ) ;
#6168 = VECTOR ( 'NONE', #7061, 1000.000000000000114 ) ;
#6169 = ORIENTED_EDGE ( 'NONE', *, *, #11792, .T. ) ;
#6170 = CARTESIAN_POINT ( 'NONE',  ( -11.89386644692969597, -19.18772505311030230, 71.68685609106418610 ) ) ;
#6171 = EDGE_CURVE ( 'NONE', #1629, #26191, #9027, .T. ) ;
#6172 = CARTESIAN_POINT ( 'NONE',  ( -13.01353307917097268, -8.804980454159759162, 64.09441913135431435 ) ) ;
#6173 = AXIS2_PLACEMENT_3D ( 'NONE', #39512, #9240, #13863 ) ;
#6174 = LINE ( 'NONE', #38933, #1234 ) ;
#6175 = CARTESIAN_POINT ( 'NONE',  ( -50.42609385541305755, -14.80920654474421205, 67.95882352941174531 ) ) ;
#6176 = ORIENTED_EDGE ( 'NONE', *, *, #18895, .T. ) ;
#6177 = ORIENTED_EDGE ( 'NONE', *, *, #16020, .F. ) ;
#6178 = CARTESIAN_POINT ( 'NONE',  ( -17.52853272358826686, -7.759682304905023642, 63.83584969886392457 ) ) ;
#6179 = CARTESIAN_POINT ( 'NONE',  ( -13.93897074462874919, -20.93787812888889377, 68.74153005185598886 ) ) ;
#6180 = CARTESIAN_POINT ( 'NONE',  ( -10.00588775665706898, -14.11983824440616075, 61.07854638698739791 ) ) ;
#6181 = ORIENTED_EDGE ( 'NONE', *, *, #14611, .T. ) ;
#6182 = CARTESIAN_POINT ( 'NONE',  ( -23.95182099924141994, -17.47225880813607901, 65.94357235735444078 ) ) ;
#6183 = CARTESIAN_POINT ( 'NONE',  ( -12.65882755920527458, -9.609488432089360543, 74.20434181795738482 ) ) ;
#6184 = EDGE_LOOP ( 'NONE', ( #38419, #5706, #45178, #34527 ) ) ;
#6185 = PLANE ( 'NONE',  #36271 ) ;
#6186 = VECTOR ( 'NONE', #44368, 1000.000000000000000 ) ;
#6187 = CARTESIAN_POINT ( 'NONE',  ( -12.88213326721828089, -9.482801177541238857, 71.04028493289825974 ) ) ;
#6188 = PRESENTATION_LAYER_ASSIGNMENT (  '', '', ( #41558 ) ) ;
#6189 = CARTESIAN_POINT ( 'NONE',  ( -23.13015969901951863, -18.95476373626217281, 58.76921843841908810 ) ) ;
#6190 = ORIENTED_EDGE ( 'NONE', *, *, #46226, .F. ) ;
#6191 = CARTESIAN_POINT ( 'NONE',  ( -14.72778340125292651, -21.32322296975913289, 58.46617885012761917 ) ) ;
#6192 = AXIS2_PLACEMENT_3D ( 'NONE', #4986, #1266, #27141 ) ;
#6193 = ORIENTED_EDGE ( 'NONE', *, *, #28020, .T. ) ;
#6194 = CARTESIAN_POINT ( 'NONE',  ( -24.87384330655416420, -14.87999779688033719, 59.35804910119406230 ) ) ;
#6195 = CARTESIAN_POINT ( 'NONE',  ( -13.51000599947710690, -20.67303722014981204, 61.52206147836523087 ) ) ;
#6196 = DIRECTION ( 'NONE',  ( 0.000000000000000000, 1.000000000000000000, -0.000000000000000000 ) ) ;
#6197 = ORIENTED_EDGE ( 'NONE', *, *, #34630, .T. ) ;
#6198 = FACE_OUTER_BOUND ( 'NONE', #37888, .T. ) ;
#6199 = EDGE_CURVE ( 'NONE', #4984, #8191, #4593, .T. ) ;
#6200 = EDGE_CURVE ( 'NONE', #40467, #23280, #26374, .T. ) ;
#6201 = CARTESIAN_POINT ( 'NONE',  ( -20.15891617451884699, -21.73914053226047827, 72.51140444708435950 ) ) ;
#6202 = CARTESIAN_POINT ( 'NONE',  ( -12.74071866071660075, -9.015263582886822391, 70.96429948631303830 ) ) ;
#6203 = AXIS2_PLACEMENT_3D ( 'NONE', #38287, #12691, #30936 ) ;
#6204 = FACE_OUTER_BOUND ( 'NONE', #28060, .T. ) ;
#6205 = CARTESIAN_POINT ( 'NONE',  ( -14.82422806554511929, -10.90997840001177366, 52.02966884056656482 ) ) ;
#6206 = CARTESIAN_POINT ( 'NONE',  ( -20.64396943983181743, -21.02470340508176250, 58.94475165022391394 ) ) ;
#6207 = VERTEX_POINT ( 'NONE', #7682 ) ;
#6208 = DIRECTION ( 'NONE',  ( -5.297746385676333075E-06, -8.914243328957358747E-06, -0.9999999999462351186 ) ) ;
#6209 = CARTESIAN_POINT ( 'NONE',  ( -11.87947861617434064, -19.08215629584865525, 71.91359129046459486 ) ) ;
#6210 = CARTESIAN_POINT ( 'NONE',  ( -22.68035891289124351, -20.08887660193805047, 69.28079699623869203 ) ) ;
#6211 = EDGE_CURVE ( 'NONE', #37990, #15682, #23215, .T. ) ;
#6212 = ADVANCED_FACE ( 'NONE', ( #38671 ), #4702, .T. ) ;
#6213 = DIRECTION ( 'NONE',  ( 0.3688590060343584498, -0.9294853595766556786, 0.000000000000000000 ) ) ;
#6214 = DIRECTION ( 'NONE',  ( -1.000000000000000000, -2.866981220435666553E-17, 0.000000000000000000 ) ) ;
#6215 = CARTESIAN_POINT ( 'NONE',  ( -13.07409385650551847, -9.792211528768506312, 50.49490371617623197 ) ) ;
#6216 = VERTEX_POINT ( 'NONE', #42859 ) ;
#6217 = VERTEX_POINT ( 'NONE', #24146 ) ;
#6218 = DIRECTION ( 'NONE',  ( -0.9848822020395751053, 0.1732254256905498280, 7.367703375004543066E-08 ) ) ;
#6219 = VERTEX_POINT ( 'NONE', #8396 ) ;
#6220 = CARTESIAN_POINT ( 'NONE',  ( -11.67943375510494697, -18.89645239624664441, 68.50217487844219022 ) ) ;
#6222 = DIRECTION ( 'NONE',  ( -3.071710424422018668E-17, 6.404604876783312462E-16, 1.000000000000000000 ) ) ;
#6221 = CARTESIAN_POINT ( 'NONE',  ( -50.42609385541305755, -14.90920654474410512, 56.99999999999998579 ) ) ;
#6223 = CARTESIAN_POINT ( 'NONE',  ( -22.58023486647882550, -9.989541079992143580, 66.69749311060769514 ) ) ;
#6224 = CARTESIAN_POINT ( 'NONE',  ( -18.86784385541312048, -9.357632978296351212, 49.97845033065735265 ) ) ;
#6225 = CARTESIAN_POINT ( 'NONE',  ( -16.96658279966119309, -22.24515547448776331, 72.26519595204030111 ) ) ;
#6226 = EDGE_LOOP ( 'NONE', ( #15030, #18307, #15418, #35070 ) ) ;
#6227 = B_SPLINE_CURVE_WITH_KNOTS ( 'NONE', 3,
 ( #16741, #16508, #19976, #46576, #31783, #39162, #35695, #13048, #27841, #8902 ),
 .UNSPECIFIED., .F., .F.,
 ( 4, 2, 2, 2, 4 ),
 ( 0.1272669073658277972, 0.2522669073439269827, 0.3772669073220261127, 0.5022669073001252427, 0.6272669072782244282 ),
 .UNSPECIFIED. ) ;
#6228 = CARTESIAN_POINT ( 'NONE',  ( -12.74613139958686503, -9.010845216743291530, 71.02738122373636998 ) ) ;
#6229 = CARTESIAN_POINT ( 'NONE',  ( -45.55409385541306477, -12.91120565595568692, 71.69928697514914973 ) ) ;
#6230 = CARTESIAN_POINT ( 'NONE',  ( -20.88122380307280324, -20.95354100073119241, 62.40911604053530226 ) ) ;
#6231 = CARTESIAN_POINT ( 'NONE',  ( -20.24919536711601964, -8.341303680600599790, 63.46688622775676691 ) ) ;
#6232 = B_SPLINE_CURVE_WITH_KNOTS ( 'NONE', 3,
 ( #17686, #16953, #47270, #17456, #47509, #13509, #43338, #28553, #9611, #20682 ),
 .UNSPECIFIED., .F., .F.,
 ( 4, 2, 2, 2, 4 ),
 ( 0.1272669073657963779, 0.2522669073462850964, 0.3772669073267738149, 0.5022669073072625334, 0.6272669072877512519 ),
 .UNSPECIFIED. ) ;
#6233 = ADVANCED_FACE ( 'NONE', ( #31529 ), #19963, .T. ) ;
#6234 = ORIENTED_EDGE ( 'NONE', *, *, #10241, .T. ) ;
#6235 = CARTESIAN_POINT ( 'NONE',  ( -21.42170527289675164, -17.27794275993632667, 52.02966884056656482 ) ) ;
#6236 = CARTESIAN_POINT ( 'NONE',  ( -12.17409406592225629, -14.80771982110106677, 52.02966884056656482 ) ) ;
#6237 = CIRCLE ( 'NONE', #34545, 1.999999999999998446 ) ;
#6238 =( BOUNDED_CURVE ( )  B_SPLINE_CURVE ( 2, ( #12223, #906, #39721, #34620, #8790, #47602, #38807, #23806, #2289 ),
 .UNSPECIFIED., .F., .F. ) 
 B_SPLINE_CURVE_WITH_KNOTS ( ( 3, 2, 2, 2, 3 ),
 ( 0.01180254302363409509, 0.01278595105271147780, 0.01376935908178886399, 0.01475276711086624844, 0.01573617513994363115 ),
 .UNSPECIFIED. ) 
 CURVE ( )  GEOMETRIC_REPRESENTATION_ITEM ( )  RATIONAL_B_SPLINE_CURVE ( ( 0.9999999999995410338, 0.9238795325117457047, 1.000000000000000000, 0.9238795325112867385, 1.000000000000000000, 0.9238795325112867385, 1.000000000000000000, 0.9238795325117954427, 0.9999999999994912958 ) ) 
 REPRESENTATION_ITEM ( '' )  );
#6239 = CARTESIAN_POINT ( 'NONE',  ( -13.20366469342568294, -8.669938804193677129, 60.63939044432547831 ) ) ;
#6240 = AXIS2_PLACEMENT_3D ( 'NONE', #31246, #35651, #46988 ) ;
#6241 = CARTESIAN_POINT ( 'NONE',  ( -24.59706363142188934, -12.79617847886399140, 66.48742024426742603 ) ) ;
#6242 = CARTESIAN_POINT ( 'NONE',  ( -13.86839427437450745, -20.83888320357228352, 65.17731955186617654 ) ) ;
#6243 = CARTESIAN_POINT ( 'NONE',  ( -16.39155882215229099, -21.78318466615559146, 61.90568132352964881 ) ) ;
#6244 = CIRCLE ( 'NONE', #33726, 4.686499999999998778 ) ;
#6245 = VECTOR ( 'NONE', #6528, 1000.000000000000114 ) ;
#6246 = EDGE_LOOP ( 'NONE', ( #7899, #31176, #19146, #15541 ) ) ;
#6247 = ORIENTED_EDGE ( 'NONE', *, *, #20266, .F. ) ;
#6248 = CARTESIAN_POINT ( 'NONE',  ( -17.63034385541304516, -6.857644439848013640, 49.98602051094139398 ) ) ;
#6249 = PLANE ( 'NONE',  #43748 ) ;
#6250 = CARTESIAN_POINT ( 'NONE',  ( -19.99112977906324318, -8.296885409642934306, 74.02096600045412345 ) ) ;
#6251 = VECTOR ( 'NONE', #44934, 1000.000000000000227 ) ;
#6252 = CARTESIAN_POINT ( 'NONE',  ( -15.68503317936312413, -7.977064329016499755, 70.60989839961001735 ) ) ;
#6253 = CARTESIAN_POINT ( 'NONE',  ( -13.94386542258548189, -20.88289783676623657, 68.45625091214465385 ) ) ;
#6254 = ORIENTED_EDGE ( 'NONE', *, *, #23073, .F. ) ;
#6255 = CARTESIAN_POINT ( 'NONE',  ( -11.00024241808776004, -11.03596260037739007, 60.78547452563873321 ) ) ;
#6256 = DIRECTION ( 'NONE',  ( 0.9687793358424819923, -0.2479245821708678243, 0.000000000000000000 ) ) ;
#6257 = EDGE_LOOP ( 'NONE', ( #33567, #38090, #44823, #45476, #28498 ) ) ;
#6258 = DIRECTION ( 'NONE',  ( 1.000000000000000000, 0.000000000000000000, 1.927470528863119295E-16 ) ) ;
#6259 = ORIENTED_EDGE ( 'NONE', *, *, #6547, .F. ) ;
#6260 = CARTESIAN_POINT ( 'NONE',  ( -45.92409385541306222, -14.20920654474410760, 70.50000000000000000 ) ) ;
#6261 = FACE_OUTER_BOUND ( 'NONE', #22854, .T. ) ;
#6262 = VERTEX_POINT ( 'NONE', #39150 ) ;
#6263 = CARTESIAN_POINT ( 'NONE',  ( -11.71918404020638427, -18.95175453447548009, 71.70158022526054253 ) ) ;
#6264 = EDGE_CURVE ( 'NONE', #27202, #7586, #27912, .T. ) ;
#6265 = VECTOR ( 'NONE', #43453, 1000.000000000000114 ) ;
#6266 = CARTESIAN_POINT ( 'NONE',  ( -16.66975460573832635, -21.76850464344978420, 65.51098995538828262 ) ) ;
#6267 = CARTESIAN_POINT ( 'NONE',  ( -10.77500719466768686, -17.16388024452267302, 57.68760401228323076 ) ) ;
#6268 = VERTEX_POINT ( 'NONE', #12805 ) ;
#6269 = DIRECTION ( 'NONE',  ( -3.071710424422018668E-17, 6.404604876783312462E-16, 1.000000000000000000 ) ) ;
#6270 = AXIS2_PLACEMENT_3D ( 'NONE', #28983, #21838, #39582 ) ;
#6271 = CARTESIAN_POINT ( 'NONE',  ( -23.23616624490289695, -18.79948399208958776, 66.12389430041484673 ) ) ;
#6272 = CARTESIAN_POINT ( 'NONE',  ( -15.04196850781542771, -10.13074752191075234, 49.52966884056655772 ) ) ;
#6273 = ADVANCED_FACE ( 'NONE', ( #5438 ), #27830, .T. ) ;
#6274 = CARTESIAN_POINT ( 'NONE',  ( -20.12289122552838094, -7.865124802246414859, 73.90591932823114973 ) ) ;
#6275 = EDGE_CURVE ( 'NONE', #29888, #12705, #23476, .T. ) ;
#6276 = CARTESIAN_POINT ( 'NONE',  ( -13.29845767883066543, -21.01266560759323809, 61.63150935275904629 ) ) ;
#6277 = CARTESIAN_POINT ( 'NONE',  ( -22.04378365035703879, -20.13510231884741231, 62.24911246861644543 ) ) ;
#6278 = EDGE_LOOP ( 'NONE', ( #2688, #43633, #31732, #30855 ) ) ;
#6279 = CARTESIAN_POINT ( 'NONE',  ( -17.42409385541299471, -14.80920654474435771, 49.52966884056655772 ) ) ;
#6280 = CIRCLE ( 'NONE', #34591, 4.686499999999999666 ) ;
#6281 = EDGE_CURVE ( 'NONE', #17592, #30297, #22842, .T. ) ;
#6282 = FACE_OUTER_BOUND ( 'NONE', #15412, .T. ) ;
#6283 = DIRECTION ( 'NONE',  ( 0.9687793358424822143, -0.2479245821708672415, 0.000000000000000000 ) ) ;
#6284 =( BOUNDED_SURFACE ( )  B_SPLINE_SURFACE ( 3, 1, ( 
 ( #46324, #39648 ),
 ( #42639, #8899 ),
 ( #39411, #38920 ),
 ( #20206, #35218 ),
 ( #24400, #24154 ),
 ( #16505, #39159 ),
 ( #5446, #16738 ) ),
 .UNSPECIFIED., .T., .F., .F. ) 
 B_SPLINE_SURFACE_WITH_KNOTS ( ( 4, 3, 4 ),
 ( 2, 2 ),
 ( 0.000000000000000000, 0.5000000000000000000, 1.000000000000000000 ),
 ( 0.000000000000000000, 1.000000000000000000 ),
 .UNSPECIFIED. ) 
 GEOMETRIC_REPRESENTATION_ITEM ( )  RATIONAL_B_SPLINE_SURFACE ( (
 ( 1.000000000000000000, 1.000000000000000000),
 ( 0.3333333333333335369, 0.3333333333333330373),
 ( 0.3333333333333335369, 0.3333333333333330373),
 ( 1.000000000000000000, 1.000000000000000000),
 ( 0.3333333333333333703, 0.3333333333333333703),
 ( 0.3333333333333333703, 0.3333333333333333703),
 ( 1.000000000000000000, 1.000000000000000000) ) ) 
 REPRESENTATION_ITEM ( '' )  SURFACE ( )  );
#6285 = ORIENTED_EDGE ( 'NONE', *, *, #4971, .F. ) ;
#6286 = DIRECTION ( 'NONE',  ( -0.7300417127692488961, -0.6834025882427879894, -6.612978995310452690E-09 ) ) ;
#6287 = ORIENTED_EDGE ( 'NONE', *, *, #9883, .F. ) ;
#6288 = ORIENTED_EDGE ( 'NONE', *, *, #21154, .F. ) ;
#6289 = ORIENTED_EDGE ( 'NONE', *, *, #7217, .T. ) ;
#6290 = FACE_OUTER_BOUND ( 'NONE', #18932, .T. ) ;
#6291 = DIRECTION ( 'NONE',  ( 1.896855589267346620E-06, 2.136244919385519396E-06, 0.9999999999959191532 ) ) ;
#6292 = CARTESIAN_POINT ( 'NONE',  ( -12.86353962931362283, -9.432586330540292607, 74.33395128836551180 ) ) ;
#6293 =( BOUNDED_CURVE ( )  B_SPLINE_CURVE ( 3, ( #27843, #42873, #9142, #5452 ),
 .UNSPECIFIED., .F., .F. ) 
 B_SPLINE_CURVE_WITH_KNOTS ( ( 4, 4 ),
 ( 0.5000000000000000000, 0.9074455897393632897 ),
 .UNSPECIFIED. ) 
 CURVE ( )  GEOMETRIC_REPRESENTATION_ITEM ( )  RATIONAL_B_SPLINE_CURVE ( ( 1.000000000000006217, 0.4567392136813389625, 0.3561768502900283240, 0.6983129098260811851 ) ) 
 REPRESENTATION_ITEM ( '' )  );
#6294 = EDGE_LOOP ( 'NONE', ( #40544, #15403 ) ) ;
#6295 = VERTEX_POINT ( 'NONE', #16496 ) ;
#6296 = CARTESIAN_POINT ( 'NONE',  ( -17.94284385650551528, -8.811426318492348031, 52.18089403414751359 ) ) ;
#6297 = B_SPLINE_CURVE_WITH_KNOTS ( 'NONE', 3,
 ( #9958, #18048, #22007, #43704, #10453, #6513, #47147, #25691, #2800, #39996 ),
 .UNSPECIFIED., .F., .F.,
 ( 4, 2, 2, 2, 4 ),
 ( 0.000000000000000000, 0.2500000000000000000, 0.5000000000000000000, 0.7500000000000000000, 1.000000000000000000 ),
 .UNSPECIFIED. ) ;
#6298 = AXIS2_PLACEMENT_3D ( 'NONE', #14950, #30010, #11526 ) ;
#6299 = CARTESIAN_POINT ( 'NONE',  ( -14.32933440466380048, -7.972462762251764978, 54.15157107980258644 ) ) ;
#6300 = CARTESIAN_POINT ( 'NONE',  ( -23.19494370299929287, -18.77118727246694263, 65.82389430425217824 ) ) ;
#6301 = B_SPLINE_CURVE_WITH_KNOTS ( 'NONE', 1,
 ( #31454, #8826 ),
 .UNSPECIFIED., .F., .F.,
 ( 2, 2 ),
 ( 0.000000000000000000, 1.000000000000000000 ),
 .UNSPECIFIED. ) ;
#6302 = CARTESIAN_POINT ( 'NONE',  ( -17.94284385650551528, -8.811426318492348031, 52.18089403414751359 ) ) ;
#6303 = CIRCLE ( 'NONE', #33806, 5.249999999999998224 ) ;
#6304 = VERTEX_POINT ( 'NONE', #12570 ) ;
#6305 = DIRECTION ( 'NONE',  ( 0.2853368233144803479, -0.3443586753093368369, 0.8944271909999158554 ) ) ;
#6306 = CYLINDRICAL_SURFACE ( 'NONE', #20510, 0.1499999999999981903 ) ;
#6307 = AXIS2_PLACEMENT_3D ( 'NONE', #28310, #21871, #21159 ) ;
#6308 = ADVANCED_FACE ( 'NONE', ( #30818 ), #12089, .F. ) ;
#6309 = ORIENTED_EDGE ( 'NONE', *, *, #27193, .F. ) ;
#6310 = CARTESIAN_POINT ( 'NONE',  ( -11.21157534608376061, -11.58358818987947814, 67.91864608155252370 ) ) ;
#6311 = ORIENTED_EDGE ( 'NONE', *, *, #33423, .T. ) ;
#6312 = CARTESIAN_POINT ( 'NONE',  ( -14.63391651318349851, -8.330799758808863587, 67.55975079407809858 ) ) ;
#6313 = B_SPLINE_CURVE_WITH_KNOTS ( 'NONE', 3,
 ( #17382, #40514, #6792, #32419, #2127, #36801, #13437, #9776, #32647, #10724 ),
 .UNSPECIFIED., .F., .F.,
 ( 4, 2, 2, 2, 4 ),
 ( 0.000000000000000000, 0.2500000000000000000, 0.5000000000000000000, 0.7500000000000000000, 1.000000000000000000 ),
 .UNSPECIFIED. ) ;
#6314 = DIRECTION ( 'NONE',  ( -0.000000000000000000, -1.000000000000000000, 0.000000000000000000 ) ) ;
#6315 = DIRECTION ( 'NONE',  ( -0.000000000000000000, -1.000000000000000000, 0.000000000000000000 ) ) ;
#6316 = ORIENTED_EDGE ( 'NONE', *, *, #47059, .T. ) ;
#6317 = CARTESIAN_POINT ( 'NONE',  ( -22.79851114622174180, -10.32406479491737983, 63.29859279992308529 ) ) ;
#6318 = CYLINDRICAL_SURFACE ( 'NONE', #33101, 2.000000000000000000 ) ;
#6319 = ORIENTED_EDGE ( 'NONE', *, *, #36631, .F. ) ;
#6320 = DIRECTION ( 'NONE',  ( -0.7506333037770539507, 0.6607190350373940424, 0.000000000000000000 ) ) ;
#6321 = PLANE ( 'NONE',  #38009 ) ;
#6322 = ORIENTED_EDGE ( 'NONE', *, *, #17688, .F. ) ;
#6323 = CARTESIAN_POINT ( 'NONE',  ( -15.65034338963778460, -22.11529786783383145, 54.02312124697527906 ) ) ;
#6324 = DIRECTION ( 'NONE',  ( -0.1555549491741979040, -0.4192882752801621038, 0.8944271909999157444 ) ) ;
#6325 = ORIENTED_EDGE ( 'NONE', *, *, #37987, .T. ) ;
#6326 = LINE ( 'NONE', #13203, #45515 ) ;
#6327 = CARTESIAN_POINT ( 'NONE',  ( -24.65581703702211414, -13.01900205834191127, 62.93240538826285047 ) ) ;
#6328 = CARTESIAN_POINT ( 'NONE',  ( -18.36468646126785842, -12.35805408173462006, 53.52020502545293112 ) ) ;
#6329 = ADVANCED_FACE ( 'NONE', ( #8647 ), #27102, .T. ) ;
#6330 = B_SPLINE_CURVE_WITH_KNOTS ( 'NONE', 1,
 ( #8793, #16391 ),
 .UNSPECIFIED., .F., .F.,
 ( 2, 2 ),
 ( 0.000000000000000000, 1.000000000000000000 ),
 .UNSPECIFIED. ) ;
#6331 = FACE_OUTER_BOUND ( 'NONE', #1599, .T. ) ;
#6332 = ORIENTED_EDGE ( 'NONE', *, *, #38775, .F. ) ;
#6333 = DIRECTION ( 'NONE',  ( -0.05957303659011964347, -0.9982239494779874267, 2.515684304538401319E-08 ) ) ;
#6334 = EDGE_CURVE ( 'NONE', #3912, #42266, #29142, .T. ) ;
#6335 = CARTESIAN_POINT ( 'NONE',  ( -10.89280251029460622, -11.22507333849785027, 64.33377325762776877 ) ) ;
#6336 = DIRECTION ( 'NONE',  ( -3.071710424422018668E-17, 6.404604876783312462E-16, 1.000000000000000000 ) ) ;
#6337 = VERTEX_POINT ( 'NONE', #20198 ) ;
#6338 = CARTESIAN_POINT ( 'NONE',  ( -10.16947401241056248, -13.11399914557070190, 71.31490259464086989 ) ) ;
#6339 = EDGE_CURVE ( 'NONE', #41197, #3121, #8491, .T. ) ;
#6340 = CARTESIAN_POINT ( 'NONE',  ( -24.77336880027706911, -16.03019386047689210, 66.16301287370103523 ) ) ;
#6341 = ORIENTED_EDGE ( 'NONE', *, *, #22179, .F. ) ;
#6342 = ORIENTED_EDGE ( 'NONE', *, *, #9959, .F. ) ;
#6343 = CARTESIAN_POINT ( 'NONE',  ( -14.60783717270099835, -21.70648693424663378, 58.35113322083577003 ) ) ;
#6344 = CARTESIAN_POINT ( 'NONE',  ( -15.55206243756419404, -8.064171445415857065, 70.80092926608037374 ) ) ;
#6345 = CARTESIAN_POINT ( 'NONE',  ( -13.82689732469268407, -20.87277619789260186, 68.47097268802275494 ) ) ;
#6346 = AXIS2_PLACEMENT_3D ( 'NONE', #22278, #30897, #30173 ) ;
#6347 = CARTESIAN_POINT ( 'NONE',  ( -10.10901086070973420, -13.39385379864076242, 74.79162305847758319 ) ) ;
#6349 = ADVANCED_FACE ( 'NONE', ( #45512 ), #29998, .F. ) ;
#6348 = CARTESIAN_POINT ( 'NONE',  ( -19.43549419715917281, -7.635817758345905482, 60.15431310326993497 ) ) ;
#6350 = CARTESIAN_POINT ( 'NONE',  ( -21.22541856475621103, -21.21643550156703384, 65.68430309725735583 ) ) ;
#6351 = CARTESIAN_POINT ( 'NONE',  ( -20.03282965983824226, -21.84088468745754597, 75.49999999999994316 ) ) ;
#6352 = CARTESIAN_POINT ( 'NONE',  ( -17.78355931627749698, -7.367830628488608369, 60.27334926503960588 ) ) ;
#6353 = ORIENTED_EDGE ( 'NONE', *, *, #39944, .F. ) ;
#6354 = ORIENTED_EDGE ( 'NONE', *, *, #38850, .F. ) ;
#6355 = CARTESIAN_POINT ( 'NONE',  ( -24.83245720896766073, -15.59649170587275258, 73.04657806100746598 ) ) ;
#6356 = VECTOR ( 'NONE', #22805, 1000.000000000000000 ) ;
#6357 = CARTESIAN_POINT ( 'NONE',  ( -23.07412303265485320, -9.953122545109609476, 66.71899143667852172 ) ) ;
#6358 = CARTESIAN_POINT ( 'NONE',  ( -14.85449503969317497, -21.32098759628606643, 61.91983833741223719 ) ) ;
#6359 = LINE ( 'NONE', #21855, #27224 ) ;
#6360 = CARTESIAN_POINT ( 'NONE',  ( -24.41897151118743636, -17.37347349776957017, 69.59835227440868266 ) ) ;
#6361 = CARTESIAN_POINT ( 'NONE',  ( -19.03659385650551528, -6.915538690918074494, 49.31353937987644542 ) ) ;
#6362 = ORIENTED_EDGE ( 'NONE', *, *, #8334, .F. ) ;
#6363 = VECTOR ( 'NONE', #13235, 1000.000000000000000 ) ;
#6364 = CARTESIAN_POINT ( 'NONE',  ( -14.79906637807316550, -21.78150152883456059, 61.67954536979805624 ) ) ;
#6365 =( LENGTH_UNIT ( ) NAMED_UNIT ( * ) SI_UNIT ( .MILLI., .METRE. ) );
#6366 = AXIS2_PLACEMENT_3D ( 'NONE', #43771, #18118, #6579 ) ;
#6367 = CARTESIAN_POINT ( 'NONE',  ( -23.54569140518488624, -19.05536029250058050, 65.93894040291287695 ) ) ;
#6368 = CARTESIAN_POINT ( 'NONE',  ( -17.42409385541300182, -14.80920654474440745, 53.27966884056655061 ) ) ;
#6369 = EDGE_CURVE ( 'NONE', #300, #25885, #24415, .T. ) ;
#6370 = ORIENTED_EDGE ( 'NONE', *, *, #43862, .T. ) ;
#6371 = AXIS2_PLACEMENT_3D ( 'NONE', #6975, #21995, #30372 ) ;
#6372 = B_SPLINE_CURVE_WITH_KNOTS ( 'NONE', 1,
 ( #12367, #27389 ),
 .UNSPECIFIED., .F., .F.,
 ( 2, 2 ),
 ( 0.000000000000000000, 1.000000000000000000 ),
 .UNSPECIFIED. ) ;
#6373 = CARTESIAN_POINT ( 'NONE',  ( -10.59464835643876413, -16.34528333370979780, 71.67423614857023040 ) ) ;
#6374 = CARTESIAN_POINT ( 'NONE',  ( -12.84719740098974583, -9.512790884556105553, 74.61923006383901225 ) ) ;
#6375 = AXIS2_PLACEMENT_3D ( 'NONE', #46465, #21077, #13659 ) ;
#6376 = CARTESIAN_POINT ( 'NONE',  ( -15.62101046192594289, -7.580605815997546237, 70.72494447658496597 ) ) ;
#6377 = CARTESIAN_POINT ( 'NONE',  ( -20.78299823145727387, -8.610459808214880439, 59.85597358678664648 ) ) ;
#6378 = VERTEX_POINT ( 'NONE', #41561 ) ;
#6379 = EDGE_CURVE ( 'NONE', #27994, #8183, #42347, .T. ) ;
#6380 = DIRECTION ( 'NONE',  ( 0.9687793358424819923, -0.2479245821708676023, 0.000000000000000000 ) ) ;
#6381 = ORIENTED_EDGE ( 'NONE', *, *, #618, .T. ) ;
#6382 = CARTESIAN_POINT ( 'NONE',  ( -22.23733845922741637, -19.96043711175405733, 66.00421731380804147 ) ) ;
#6383 = B_SPLINE_CURVE_WITH_KNOTS ( 'NONE', 3,
 ( #23591, #42550, #1654, #20126, #4879, #5609, #46485, #39321, #35133, #27030 ),
 .UNSPECIFIED., .F., .F.,
 ( 4, 2, 2, 2, 4 ),
 ( 0.1272669073657147210, 0.2522669073438441600, 0.3772669073219735436, 0.5022669073001029272, 0.6272669072782521837 ),
 .UNSPECIFIED. ) ;
#6384 = ORIENTED_EDGE ( 'NONE', *, *, #36266, .F. ) ;
#6385 = FACE_OUTER_BOUND ( 'NONE', #13373, .T. ) ;
#6386 = VECTOR ( 'NONE', #16843, 1000.000000000000114 ) ;
#6387 = CARTESIAN_POINT ( 'NONE',  ( -14.06159385650551741, -9.295667164867525756, 49.30633214617472504 ) ) ;
#6388 = EDGE_LOOP ( 'NONE', ( #18972, #37630, #10838, #26324, #10534 ) ) ;
#6389 = CYLINDRICAL_SURFACE ( 'NONE', #20548, 2.500000000000000444 ) ;
#6390 = CARTESIAN_POINT ( 'NONE',  ( -20.78299823145727387, -8.610459808214880439, 59.85597358678664648 ) ) ;
#6391 = DIRECTION ( 'NONE',  ( -3.413470714839332458E-33, 1.190614954331866791E-16, -1.000000000000000000 ) ) ;
#6392 = EDGE_LOOP ( 'NONE', ( #42363, #3987, #33703, #38748, #31786, #15695, #7014, #12592 ) ) ;
#6393 = CARTESIAN_POINT ( 'NONE',  ( -24.47217469780903443, -14.64471797168181411, 63.01296487297643267 ) ) ;
#6394 = CARTESIAN_POINT ( 'NONE',  ( -17.22121256223034536, -7.361891212656819228, 70.74681744497029001 ) ) ;
#6395 = EDGE_CURVE ( 'NONE', #27130, #28666, #44265, .T. ) ;
#6396 = DIRECTION ( 'NONE',  ( 0.9687793358424821033, -0.2479245821708679909, 0.000000000000000000 ) ) ;
#6397 = STYLED_ITEM ( 'NONE', ( #20485 ), #31806 ) ;
#6398 = CARTESIAN_POINT ( 'NONE',  ( -45.92409385541305511, -15.80920654474410725, 69.24999999999998579 ) ) ;
#6399 = EDGE_LOOP ( 'NONE', ( #42901, #10915, #47342, #29244, #30626 ) ) ;
#6400 = ORIENTED_EDGE ( 'NONE', *, *, #21745, .F. ) ;
#6401 = VECTOR ( 'NONE', #31165, 1000.000000000000000 ) ;
#6402 = DIRECTION ( 'NONE',  ( -1.000000000000000000, 4.164305804376849172E-17, -1.614929280266638808E-16 ) ) ;
#6403 = CARTESIAN_POINT ( 'NONE',  ( -24.69816866750256779, -16.41902046076232935, 59.16686479676427979 ) ) ;
#6404 = VERTEX_POINT ( 'NONE', #4615 ) ;
#6405 = CARTESIAN_POINT ( 'NONE',  ( -17.26599293058224305, -9.561587646847176103, 49.52966884056655772 ) ) ;
#6406 = EDGE_CURVE ( 'NONE', #33723, #43487, #21114, .T. ) ;
#6407 = CARTESIAN_POINT ( 'NONE',  ( -19.68659385759799108, -7.222650657624104298, 49.61879703869476543 ) ) ;
#6408 = FACE_OUTER_BOUND ( 'NONE', #35842, .T. ) ;
#6409 = FACE_OUTER_BOUND ( 'NONE', #3743, .T. ) ;
#6410 = CARTESIAN_POINT ( 'NONE',  ( -15.62222905942472018, -7.993050613273783966, 70.89517703929612935 ) ) ;
#6411 = CIRCLE ( 'NONE', #21353, 1.250000000000001110 ) ;
#6412 = VERTEX_POINT ( 'NONE', #4373 ) ;
#6413 = CARTESIAN_POINT ( 'NONE',  ( -20.54394416162392289, -8.483752705004535599, 59.72636470710568091 ) ) ;
#6414 = CARTESIAN_POINT ( 'NONE',  ( -14.19282086353638839, -8.542981675383003903, 71.01485553001869278 ) ) ;
#6415 = CIRCLE ( 'NONE', #32366, 4.686499999999997002 ) ;
#6416 = DIRECTION ( 'NONE',  ( -8.993561335472250294E-07, 8.977735684497376994E-07, 0.9999999999991925348 ) ) ;
#6417 = CARTESIAN_POINT ( 'NONE',  ( -17.42409385541299471, -14.80920654474434883, 62.02966884056656482 ) ) ;
#6418 =( BOUNDED_CURVE ( )  B_SPLINE_CURVE ( 3, ( #38981, #19540, #16312, #46132 ),
 .UNSPECIFIED., .F., .F. ) 
 B_SPLINE_CURVE_WITH_KNOTS ( ( 4, 4 ),
 ( 0.4074455897393657322, 0.5000000000000000000 ),
 .UNSPECIFIED. ) 
 CURVE ( )  GEOMETRIC_REPRESENTATION_ITEM ( )  RATIONAL_B_SPLINE_CURVE ( ( 0.6983129098260999479, 0.7760317562606904307, 0.8765941196519864143, 0.9999999999999781286 ) ) 
 REPRESENTATION_ITEM ( '' )  );
#6419 = ADVANCED_FACE ( 'NONE', ( #7597 ), #23334, .T. ) ;
#6420 = EDGE_CURVE ( 'NONE', #30331, #45668, #39063, .T. ) ;
#6421 = ORIENTED_EDGE ( 'NONE', *, *, #31859, .T. ) ;
#6422 = ORIENTED_EDGE ( 'NONE', *, *, #42768, .F. ) ;
#6423 = ADVANCED_FACE ( 'NONE', ( #41309 ), #214, .T. ) ;
#6424 = ADVANCED_FACE ( 'NONE', ( #38091 ), #41073, .T. ) ;
#6425 = CARTESIAN_POINT ( 'NONE',  ( -20.56872696718735938, -8.555305145393857558, 60.03228400242546314 ) ) ;
#6426 = VECTOR ( 'NONE', #30329, 1000.000000000000000 ) ;
#6427 = CARTESIAN_POINT ( 'NONE',  ( -23.63369358133848053, -11.57797282307057607, 63.06104349419704391 ) ) ;
#6428 = B_SPLINE_CURVE_WITH_KNOTS ( 'NONE', 3,
 ( #18008, #2761, #36251, #29356, #36481, #47826, #6709, #5979, #40668, #21001 ),
 .UNSPECIFIED., .F., .F.,
 ( 4, 2, 2, 2, 4 ),
 ( 0.000000000000000000, 0.2500000000000000000, 0.5000000000000000000, 0.7500000000000000000, 1.000000000000000000 ),
 .UNSPECIFIED. ) ;
#6429 = CARTESIAN_POINT ( 'NONE',  ( -45.50908060261262023, -14.20920654474410760, 70.13000000000000966 ) ) ;
#6430 = CARTESIAN_POINT ( 'NONE',  ( -23.28921155407422106, -22.22116534042542213, 53.49999999999995026 ) ) ;
#6431 =( BOUNDED_SURFACE ( )  B_SPLINE_SURFACE ( 3, 1, ( 
 ( #28919, #43963 ),
 ( #6523, #21544 ),
 ( #41215, #3798 ),
 ( #22262, #19055 ),
 ( #7000, #6761 ),
 ( #48119, #29904 ),
 ( #21773, #33558 ) ),
 .UNSPECIFIED., .T., .F., .F. ) 
 B_SPLINE_SURFACE_WITH_KNOTS ( ( 4, 3, 4 ),
 ( 2, 2 ),
 ( 0.000000000000000000, 0.5000000000000000000, 1.000000000000000000 ),
 ( 0.000000000000000000, 1.000000000000000000 ),
 .UNSPECIFIED. ) 
 GEOMETRIC_REPRESENTATION_ITEM ( )  RATIONAL_B_SPLINE_SURFACE ( (
 ( 1.000000000000000000, 1.000000000000000000),
 ( 0.3333333333333335369, 0.3333333333333330373),
 ( 0.3333333333333335369, 0.3333333333333330373),
 ( 1.000000000000000000, 1.000000000000000000),
 ( 0.3333333333333333703, 0.3333333333333333703),
 ( 0.3333333333333333703, 0.3333333333333333703),
 ( 1.000000000000000000, 1.000000000000000000) ) ) 
 REPRESENTATION_ITEM ( '' )  SURFACE ( )  );
#6432 = VERTEX_POINT ( 'NONE', #37353 ) ;
#6433 =( BOUNDED_SURFACE ( )  B_SPLINE_SURFACE ( 3, 1, ( 
 ( #40170, #47787 ),
 ( #32988, #18220 ),
 ( #10381, #25387 ),
 ( #43877, #36673 ),
 ( #10607, #9658 ),
 ( #2960, #48031 ),
 ( #6441, #36929 ) ),
 .UNSPECIFIED., .T., .F., .F. ) 
 B_SPLINE_SURFACE_WITH_KNOTS ( ( 4, 3, 4 ),
 ( 2, 2 ),
 ( 0.000000000000000000, 0.5000000000000000000, 1.000000000000000000 ),
 ( 0.000000000000000000, 1.000000000000000000 ),
 .UNSPECIFIED. ) 
 GEOMETRIC_REPRESENTATION_ITEM ( )  RATIONAL_B_SPLINE_SURFACE ( (
 ( 1.000000000000000000, 1.000000000000000000),
 ( 0.3333333333333335369, 0.3333333333333330373),
 ( 0.3333333333333335369, 0.3333333333333330373),
 ( 1.000000000000000000, 1.000000000000000000),
 ( 0.3333333333333333703, 0.3333333333333333703),
 ( 0.3333333333333333703, 0.3333333333333333703),
 ( 1.000000000000000000, 1.000000000000000000) ) ) 
 REPRESENTATION_ITEM ( '' )  SURFACE ( )  );
#6434 = CARTESIAN_POINT ( 'NONE',  ( -16.24532195521571865, -7.452882185367804446, 60.33995147283161486 ) ) ;
#6435 = B_SPLINE_CURVE_WITH_KNOTS ( 'NONE', 3,
 ( #48434, #6357, #47713, #36135, #28762, #2419, #29485, #21137, #10052, #44770 ),
 .UNSPECIFIED., .F., .F.,
 ( 4, 2, 2, 2, 4 ),
 ( 0.6272669072877826713, 0.7522669073072950630, 0.8772669073268073436, 1.002266907346319735, 1.127266907365832127 ),
 .UNSPECIFIED. ) ;
#6436 = VECTOR ( 'NONE', #23331, 1000.000000000000000 ) ;
#6437 = CARTESIAN_POINT ( 'NONE',  ( -11.09714801257800865, -11.68115280588511773, 64.30448977214732054 ) ) ;
#6438 = ORIENTED_EDGE ( 'NONE', *, *, #45422, .T. ) ;
#6439 = CIRCLE ( 'NONE', #8808, 2.000000000000001776 ) ;
#6440 = CARTESIAN_POINT ( 'NONE',  ( -16.97945985512182787, -21.84517132341290591, 72.16543221430227106 ) ) ;
#6441 = CARTESIAN_POINT ( 'NONE',  ( -24.47066272824306665, -14.57993217219608795, 62.99824437345093031 ) ) ;
#6442 = CARTESIAN_POINT ( 'NONE',  ( -21.95523322170430092, -8.895446802377390938, 66.77654591769551473 ) ) ;
#6443 = ORIENTED_EDGE ( 'NONE', *, *, #12398, .F. ) ;
#6444 = PLANE ( 'NONE',  #23571 ) ;
#6445 =( BOUNDED_SURFACE ( )  B_SPLINE_SURFACE ( 3, 1, ( 
 ( #45830, #27099 ),
 ( #42125, #42372 ),
 ( #8643, #23666 ),
 ( #35206, #1476 ),
 ( #32262, #16236 ),
 ( #39875, #47022 ),
 ( #6149, #16491 ) ),
 .UNSPECIFIED., .T., .F., .F. ) 
 B_SPLINE_SURFACE_WITH_KNOTS ( ( 4, 3, 4 ),
 ( 2, 2 ),
 ( 0.000000000000000000, 0.5000000000000000000, 1.000000000000000000 ),
 ( 0.000000000000000000, 1.000000000000000000 ),
 .UNSPECIFIED. ) 
 GEOMETRIC_REPRESENTATION_ITEM ( )  RATIONAL_B_SPLINE_SURFACE ( (
 ( 1.000000000000000000, 1.000000000000000000),
 ( 0.3333333333333335369, 0.3333333333333330373),
 ( 0.3333333333333335369, 0.3333333333333330373),
 ( 1.000000000000000000, 1.000000000000000000),
 ( 0.3333333333333333703, 0.3333333333333333703),
 ( 0.3333333333333333703, 0.3333333333333333703),
 ( 1.000000000000000000, 1.000000000000000000) ) ) 
 REPRESENTATION_ITEM ( '' )  SURFACE ( )  );
#6446 = ORIENTED_EDGE ( 'NONE', *, *, #18757, .F. ) ;
#6447 = CARTESIAN_POINT ( 'NONE',  ( -24.08638337272136098, -17.13919944035470522, 66.09924551876292753 ) ) ;
#6448 = CARTESIAN_POINT ( 'NONE',  ( -18.67409385759799179, -6.859212275519751323, 50.50378509014259265 ) ) ;
#6449 = CARTESIAN_POINT ( 'NONE',  ( -19.36999377412127288, -21.53330303623953057, 58.63393313907128856 ) ) ;
#6450 = ORIENTED_EDGE ( 'NONE', *, *, #25084, .F. ) ;
#6451 = CARTESIAN_POINT ( 'NONE',  ( -24.47401588439613818, -14.84236418521736312, 59.54300237059217693 ) ) ;
#6452 = CARTESIAN_POINT ( 'NONE',  ( -23.06159385650551386, -9.295667164867525756, 49.30633214617472504 ) ) ;
#6453 = CARTESIAN_POINT ( 'NONE',  ( -13.16616306552584525, -16.76709000361798729, 49.52966884056655772 ) ) ;
#6454 = CARTESIAN_POINT ( 'NONE',  ( -14.17409385759798823, -6.859212275519751323, 50.50378509014259265 ) ) ;
#6455 = CARTESIAN_POINT ( 'NONE',  ( -12.23220172533775241, -19.57856247689574403, 57.92682373937842044 ) ) ;
#6456 = EDGE_LOOP ( 'NONE', ( #32457, #404 ) ) ;
#6457 = FACE_OUTER_BOUND ( 'NONE', #48275, .T. ) ;
#6458 = CARTESIAN_POINT ( 'NONE',  ( -11.87925614048969614, -19.08186516019194201, 71.75973838716171826 ) ) ;
#6459 = CARTESIAN_POINT ( 'NONE',  ( -17.42409385541299471, -14.80920654474435771, 49.52966884056655772 ) ) ;
#6460 = PLANE ( 'NONE',  #13970 ) ;
#6461 = EDGE_CURVE ( 'NONE', #29021, #22071, #877, .T. ) ;
#6462 = CARTESIAN_POINT ( 'NONE',  ( -15.99552465959851233, -21.71601670177824417, 58.70074462513652236 ) ) ;
#6463 = CARTESIAN_POINT ( 'NONE',  ( -11.85162103594838001, -10.49015045520576983, 71.25420998615621215 ) ) ;
#6464 = ORIENTED_EDGE ( 'NONE', *, *, #36837, .F. ) ;
#6465 = VERTEX_POINT ( 'NONE', #34156 ) ;
#6466 = CARTESIAN_POINT ( 'NONE',  ( -13.27161037900033058, -18.02158587759403829, 52.02966884056656482 ) ) ;
#6467 = CARTESIAN_POINT ( 'NONE',  ( -10.86613940586139471, -12.21176972022029972, 57.42037321672007266 ) ) ;
#6468 = EDGE_LOOP ( 'NONE', ( #44910, #38367, #1438, #38617 ) ) ;
#6469 = CARTESIAN_POINT ( 'NONE',  ( -23.47491605241627255, -11.19111043747921208, 73.36193326491972755 ) ) ;
#6471 = CARTESIAN_POINT ( 'NONE',  ( -11.79792992861738909, -18.97409303405279957, 71.98685885147807539 ) ) ;
#6470 = LINE ( 'NONE', #31602, #47113 ) ;
#6472 = CARTESIAN_POINT ( 'NONE',  ( -18.58659385541303521, -7.222650657624098969, 49.61879703869476543 ) ) ;
#6473 = CARTESIAN_POINT ( 'NONE',  ( -22.22371030936713510, -9.111184089457765367, 59.90666523727240644 ) ) ;
#6474 = CARTESIAN_POINT ( 'NONE',  ( -22.78678303852979425, -9.565966637465477262, 54.27966884056655061 ) ) ;
#6475 = FACE_BOUND ( 'NONE', #9485, .T. ) ;
#6476 = LINE ( 'NONE', #13829, #35708 ) ;
#6477 = DIRECTION ( 'NONE',  ( 0.9375570856950864451, -0.3478314405900309603, 3.549360974553816870E-17 ) ) ;
#6478 = B_SPLINE_CURVE_WITH_KNOTS ( 'NONE', 3,
 ( #45291, #45536, #11539, #22888, #11794, #41837, #8110, #38117, #4394, #43289 ),
 .UNSPECIFIED., .F., .F.,
 ( 4, 2, 2, 2, 4 ),
 ( 0.000000000000000000, 0.2500000000000000000, 0.5000000000000000000, 0.7500000000000000000, 1.000000000000000000 ),
 .UNSPECIFIED. ) ;
#6479 = CARTESIAN_POINT ( 'NONE',  ( -20.69652669518947263, -8.116311108972663391, 63.35475588450814399 ) ) ;
#6480 = ORIENTED_EDGE ( 'NONE', *, *, #20116, .T. ) ;
#6481 = LINE ( 'NONE', #10420, #26660 ) ;
#6482 = VECTOR ( 'NONE', #27973, 1000.000000000000000 ) ;
#6483 = CARTESIAN_POINT ( 'NONE',  ( -45.92409385541306222, -14.20920654474410760, 70.50000000000000000 ) ) ;
#6484 = CARTESIAN_POINT ( 'NONE',  ( -18.50517187854146783, -19.38160480531894692, 49.52966884056656482 ) ) ;
#6485 = CARTESIAN_POINT ( 'NONE',  ( -10.70366717127368084, -11.59369238842668359, 71.13214950009151494 ) ) ;
#6486 = CARTESIAN_POINT ( 'NONE',  ( -13.54792730259346456, -8.920061342218058797, 57.25495614889487683 ) ) ;
#6488 = ORIENTED_EDGE ( 'NONE', *, *, #38402, .T. ) ;
#6487 = ADVANCED_FACE ( 'NONE', ( #15427 ), #41815, .T. ) ;
#6489 = EDGE_LOOP ( 'NONE', ( #5469, #11006, #33117, #30223 ) ) ;
#6490 = CARTESIAN_POINT ( 'NONE',  ( -17.01159385541303948, -8.990409506049200417, 49.61344411288074951 ) ) ;
#6491 = B_SPLINE_CURVE_WITH_KNOTS ( 'NONE', 3,
 ( #6343, #19305, #21375, #25967, #40986, #33565, #14847, #15844, #16318, #1309 ),
 .UNSPECIFIED., .F., .F.,
 ( 4, 2, 2, 2, 4 ),
 ( 0.6272669072877875562, 0.7522669073072943968, 0.8772669073268013484, 1.002266907346308189, 1.127266907365815030 ),
 .UNSPECIFIED. ) ;
#6492 = EDGE_CURVE ( 'NONE', #23748, #15544, #32864, .T. ) ;
#6493 = ADVANCED_FACE ( 'NONE', ( #17389 ), #40521, .T. ) ;
#6494 = FACE_OUTER_BOUND ( 'NONE', #48057, .T. ) ;
#6495 = CARTESIAN_POINT ( 'NONE',  ( -11.73157977884637226, -10.00306985186507269, 67.75542791425031908 ) ) ;
#6496 = EDGE_CURVE ( 'NONE', #37312, #48665, #35483, .T. ) ;
#6497 = CARTESIAN_POINT ( 'NONE',  ( -20.41784385759799036, -6.860780111191480124, 51.02154966934376290 ) ) ;
#6498 = CARTESIAN_POINT ( 'NONE',  ( -10.37714865501246564, -15.10143083228766159, 74.68290095780284332 ) ) ;
#6499 = ORIENTED_EDGE ( 'NONE', *, *, #12701, .F. ) ;
#6500 = B_SPLINE_CURVE_WITH_KNOTS ( 'NONE', 3,
 ( #35378, #27990, #12493, #23836, #38836, #43017, #23108, #38099, #4380, #36096 ),
 .UNSPECIFIED., .F., .F.,
 ( 4, 2, 2, 2, 4 ),
 ( 0.6272669072877699037, 0.7522669073072681956, 0.8772669073267664874, 1.002266907346264890, 1.127266907365763071 ),
 .UNSPECIFIED. ) ;
#6501 = CARTESIAN_POINT ( 'NONE',  ( -35.32409385541306079, -2.423472813913224222, 52.29999999999998295 ) ) ;
#6502 = CARTESIAN_POINT ( 'NONE',  ( -20.66122932390920752, -21.07544863110783950, 62.52960166509647166 ) ) ;
#6503 = ORIENTED_EDGE ( 'NONE', *, *, #15362, .F. ) ;
#6504 = LINE ( 'NONE', #18039, #40678 ) ;
#6505 = B_SPLINE_CURVE_WITH_KNOTS ( 'NONE', 3,
 ( #11230, #25748, #18854, #44726, #26485, #37295, #22811, #33119, #21814, #10501 ),
 .UNSPECIFIED., .F., .F.,
 ( 4, 2, 2, 2, 4 ),
 ( 0.1272669073658691807, 0.2522669073463420508, 0.3772669073268148932, 0.5022669073072877355, 0.6272669072877605778 ),
 .UNSPECIFIED. ) ;
#6506 = CARTESIAN_POINT ( 'NONE',  ( -23.27284462870851911, -18.74605969774991010, 66.10917289053097079 ) ) ;
#6507 = ORIENTED_EDGE ( 'NONE', *, *, #39062, .T. ) ;
#6508 = CARTESIAN_POINT ( 'NONE',  ( -13.57572078670752447, -20.65643022133334128, 61.81646323932617548 ) ) ;
#6509 = DIRECTION ( 'NONE',  ( 0.9687793358424817702, -0.2479245821708686570, 0.000000000000000000 ) ) ;
#6510 = ORIENTED_EDGE ( 'NONE', *, *, #46542, .T. ) ;
#6511 = CARTESIAN_POINT ( 'NONE',  ( -11.91343869374197695, -19.82283377674160718, 58.04186948019505365 ) ) ;
#6512 = EDGE_CURVE ( 'NONE', #24347, #44745, #29428, .T. ) ;
#6513 = CARTESIAN_POINT ( 'NONE',  ( -23.32920267011340698, -18.57114636909328453, 72.95295412063659057 ) ) ;
#6514 = CARTESIAN_POINT ( 'NONE',  ( -16.63459736671760325, -21.76466575500571921, 65.52564349350808470 ) ) ;
#6515 = CARTESIAN_POINT ( 'NONE',  ( -24.69661721059186377, -13.19217688614222084, 59.53984779040520436 ) ) ;
#6516 = ORIENTED_EDGE ( 'NONE', *, *, #17217, .F. ) ;
#6517 = FACE_OUTER_BOUND ( 'NONE', #2193, .T. ) ;
#6518 = CARTESIAN_POINT ( 'NONE',  ( -14.60689764421331560, -8.346551857622415582, 63.78978840692986552 ) ) ;
#6519 = DIRECTION ( 'NONE',  ( 3.289814896819423347E-07, 7.277561374119425783E-07, -0.9999999999996811439 ) ) ;
#6520 = CARTESIAN_POINT ( 'NONE',  ( -11.47140389976542529, -10.32934621678965037, 74.69531023250135604 ) ) ;
#6521 = EDGE_CURVE ( 'NONE', #11451, #17592, #31021, .T. ) ;
#6522 = CARTESIAN_POINT ( 'NONE',  ( -16.71379370341422543, -22.22534705626145879, 68.95206582789661809 ) ) ;
#6523 = CARTESIAN_POINT ( 'NONE',  ( -24.24394117090890788, -12.99133827687660059, 59.51834745271546723 ) ) ;
#6524 = ORIENTED_EDGE ( 'NONE', *, *, #28355, .T. ) ;
#6525 = CARTESIAN_POINT ( 'NONE',  ( -24.32109429401129930, -17.62606226209447158, 66.05083068898602505 ) ) ;
#6526 =( BOUNDED_CURVE ( )  B_SPLINE_CURVE ( 3, ( #1804, #20527, #5976, #24219 ),
 .UNSPECIFIED., .F., .F. ) 
 B_SPLINE_CURVE_WITH_KNOTS ( ( 4, 4 ),
 ( 0.4074455897393669535, 0.5000000000000000000 ),
 .UNSPECIFIED. ) 
 CURVE ( )  GEOMETRIC_REPRESENTATION_ITEM ( )  RATIONAL_B_SPLINE_CURVE ( ( 0.6983129098260987266, 0.7760317562606950936, 0.8765941196519931866, 0.9999999999999873435 ) ) 
 REPRESENTATION_ITEM ( '' )  );
#6527 = CARTESIAN_POINT ( 'NONE',  ( -14.28913879486226435, -8.050816564744696535, 67.37479651646088996 ) ) ;
#6528 = DIRECTION ( 'NONE',  ( -0.7847243476406476903, -0.6198448985189423110, 4.433022207822355740E-08 ) ) ;
#6529 = ORIENTED_EDGE ( 'NONE', *, *, #41927, .F. ) ;
#6530 = CARTESIAN_POINT ( 'NONE',  ( -17.42409385541299471, -14.80920654474435771, 49.52966884056655772 ) ) ;
#6531 = VERTEX_POINT ( 'NONE', #17129 ) ;
#6532 = EDGE_LOOP ( 'NONE', ( #17111, #8368, #27777, #35397, #20732 ) ) ;
#6533 = EDGE_LOOP ( 'NONE', ( #40539, #26938, #25202, #33566 ) ) ;
#6534 = VECTOR ( 'NONE', #30679, 1000.000000000000000 ) ;
#6535 = CARTESIAN_POINT ( 'NONE',  ( -18.83586040784625126, -7.494106175837369044, 70.48572642001049360 ) ) ;
#6536 = CARTESIAN_POINT ( 'NONE',  ( -23.72735656903896029, -11.76458228029187936, 59.70909150386957265 ) ) ;
#6537 = CARTESIAN_POINT ( 'NONE',  ( -14.44809135640554487, -8.473323881223761234, 67.55975083863336295 ) ) ;
#6538 = CARTESIAN_POINT ( 'NONE',  ( -12.83255559692156567, -9.459361206898796226, 74.31923029311820983 ) ) ;
#6539 = ORIENTED_EDGE ( 'NONE', *, *, #12516, .T. ) ;
#6540 = ORIENTED_EDGE ( 'NONE', *, *, #10979, .T. ) ;
#6541 = CARTESIAN_POINT ( 'NONE',  ( -17.26784385650551457, -6.428312510596451368, 51.20221977374900035 ) ) ;
#6542 = EDGE_CURVE ( 'NONE', #10524, #26883, #43151, .T. ) ;
#6543 = CARTESIAN_POINT ( 'NONE',  ( 18.07590614458695200, 2.989985547936196753, 50.78361045430852982 ) ) ;
#6544 = LINE ( 'NONE', #33094, #8738 ) ;
#6545 = CARTESIAN_POINT ( 'NONE',  ( -18.05534385650551599, -7.417179338643134834, 52.18511593390279302 ) ) ;
#6546 = ADVANCED_FACE ( 'NONE', ( #9543 ), #20953, .T. ) ;
#6548 = ORIENTED_EDGE ( 'NONE', *, *, #873, .T. ) ;
#6547 = EDGE_CURVE ( 'NONE', #48469, #12722, #3822, .T. ) ;
#6549 = CARTESIAN_POINT ( 'NONE',  ( -15.14815771252334820, -21.49015593068176244, 72.19008430323151515 ) ) ;
#6550 = EDGE_CURVE ( 'NONE', #31760, #20698, #36340, .T. ) ;
#6551 = CARTESIAN_POINT ( 'NONE',  ( -22.58065782673598321, -12.89613362149922438, 53.49899999999994549 ) ) ;
#6552 = EDGE_CURVE ( 'NONE', #29515, #16353, #34452, .T. ) ;
#6553 = ORIENTED_EDGE ( 'NONE', *, *, #22371, .F. ) ;
#6554 = DIRECTION ( 'NONE',  ( 0.6621635203543605463, 0.7493593746073505812, 2.316976118889565779E-08 ) ) ;
#6555 = ORIENTED_EDGE ( 'NONE', *, *, #9154, .F. ) ;
#6556 = B_SPLINE_CURVE_WITH_KNOTS ( 'NONE', 1,
 ( #33242, #25164 ),
 .UNSPECIFIED., .F., .F.,
 ( 2, 2 ),
 ( 0.000000000000000000, 1.000000000000000000 ),
 .UNSPECIFIED. ) ;
#6557 = CARTESIAN_POINT ( 'NONE',  ( -19.37409385541300111, -6.859212275519753099, 50.50378509014300477 ) ) ;
#6558 = CARTESIAN_POINT ( 'NONE',  ( -18.26831188466123024, -21.75822359800944739, 68.81514735240074288 ) ) ;
#6559 = CARTESIAN_POINT ( 'NONE',  ( -11.37040629063227115, -11.19590673242557166, 60.67885808612489029 ) ) ;
#6560 = EDGE_CURVE ( 'NONE', #18524, #44188, #29692, .T. ) ;
#6561 = AXIS2_PLACEMENT_3D ( 'NONE', #27093, #37420, #18718 ) ;
#6562 = ORIENTED_EDGE ( 'NONE', *, *, #33024, .T. ) ;
#6563 = CARTESIAN_POINT ( 'NONE',  ( -12.79645718024698553, -9.490555657722758554, 74.61922982865735321 ) ) ;
#6564 =( BOUNDED_CURVE ( )  B_SPLINE_CURVE ( 3, ( #9706, #33038, #3264, #18268 ),
 .UNSPECIFIED., .F., .F. ) 
 B_SPLINE_CURVE_WITH_KNOTS ( ( 4, 4 ),
 ( 0.5000000000000000000, 0.9074455897393690629 ),
 .UNSPECIFIED. ) 
 CURVE ( )  GEOMETRIC_REPRESENTATION_ITEM ( )  RATIONAL_B_SPLINE_CURVE ( ( 1.000000000000022871, 0.4567392136813325232, 0.3561768502900143352, 0.6983129098260932865 ) ) 
 REPRESENTATION_ITEM ( '' )  );
#6565 = CARTESIAN_POINT ( 'NONE',  ( -18.44528782684011858, -21.78515541812411982, 72.29983070759432451 ) ) ;
#6566 = CYLINDRICAL_SURFACE ( 'NONE', #35480, 0.1500000000000002720 ) ;
#6567 = EDGE_LOOP ( 'NONE', ( #25976, #8133 ) ) ;
#6568 = DIRECTION ( 'NONE',  ( 0.5820088206811424580, -0.8131824719270213109, 7.019974882119936121E-08 ) ) ;
#6569 = CARTESIAN_POINT ( 'NONE',  ( -21.41863048803933012, -8.999699081277377388, 73.61600897546567523 ) ) ;
#6570 = CARTESIAN_POINT ( 'NONE',  ( -15.03263910315855512, -8.176888424288378587, 56.86472059657746314 ) ) ;
#6571 = ORIENTED_EDGE ( 'NONE', *, *, #42142, .F. ) ;
#6572 = CARTESIAN_POINT ( 'NONE',  ( -13.47696527960146895, -8.967565513329615712, 60.44510101887779996 ) ) ;
#6573 = EDGE_LOOP ( 'NONE', ( #2111, #48700, #24313, #16481, #3614 ) ) ;
#6574 = CARTESIAN_POINT ( 'NONE',  ( -10.72530867274958233, -17.00760959713300480, 57.97288447305808745 ) ) ;
#6575 = CARTESIAN_POINT ( 'NONE',  ( -24.65228577264951326, -13.00463492950681754, 62.93925847568694820 ) ) ;
#6576 = DIRECTION ( 'NONE',  ( 0.9687793358424817702, -0.2479245821708688791, 0.000000000000000000 ) ) ;
#6577 = CARTESIAN_POINT ( 'NONE',  ( -14.97188219925329378, -8.199429090594037461, 56.84999999999994458 ) ) ;
#6578 = ORIENTED_EDGE ( 'NONE', *, *, #19366, .F. ) ;
#6579 = DIRECTION ( 'NONE',  ( -5.224165706511165539E-06, 4.853367013834837651E-07, 0.9999999999862362321 ) ) ;
#6580 = FACE_BOUND ( 'NONE', #38055, .T. ) ;
#6581 = CARTESIAN_POINT ( 'NONE',  ( -15.43182990062313742, -8.046249867383863830, 74.36513541778452918 ) ) ;
#6582 = ORIENTED_EDGE ( 'NONE', *, *, #24625, .T. ) ;
#6583 = DIRECTION ( 'NONE',  ( -3.071710424422018668E-17, 6.404604876783312462E-16, 1.000000000000000000 ) ) ;
#6584 =( BOUNDED_CURVE ( )  B_SPLINE_CURVE ( 3, ( #1055, #12373, #98, #31092 ),
 .UNSPECIFIED., .F., .F. ) 
 B_SPLINE_CURVE_WITH_KNOTS ( ( 4, 4 ),
 ( 0.5000000000000000000, 0.9074455897393682857 ),
 .UNSPECIFIED. ) 
 CURVE ( )  GEOMETRIC_REPRESENTATION_ITEM ( )  RATIONAL_B_SPLINE_CURVE ( ( 1.000000000000003331, 0.4567392136813345216, 0.3561768502900287681, 0.6983129098260898449 ) ) 
 REPRESENTATION_ITEM ( '' )  );
#6585 = CARTESIAN_POINT ( 'NONE',  ( -24.66692207690629246, -13.06418342283853562, 63.08910124536953390 ) ) ;
#6586 = ORIENTED_EDGE ( 'NONE', *, *, #23398, .T. ) ;
#6587 = VERTEX_POINT ( 'NONE', #41257 ) ;
#6588 = CARTESIAN_POINT ( 'NONE',  ( -15.15660932275500095, -21.48492473237050859, 65.39124617759186719 ) ) ;
#6589 = LINE ( 'NONE', #28270, #31194 ) ;
#6590 = LINE ( 'NONE', #28753, #31365 ) ;
#6591 = CARTESIAN_POINT ( 'NONE',  ( -23.46013293835336100, -11.16077341686890989, 69.77721965307074470 ) ) ;
#6592 = EDGE_CURVE ( 'NONE', #8287, #1510, #7304, .T. ) ;
#6593 = DIRECTION ( 'NONE',  ( 2.866981220435666553E-17, -1.000000000000000000, -1.190614954331866791E-16 ) ) ;
#6594 = FACE_OUTER_BOUND ( 'NONE', #1570, .T. ) ;
#6595 = CARTESIAN_POINT ( 'NONE',  ( -17.86169286162045111, -7.371900692872102034, 60.22027394188889815 ) ) ;
#6596 = ORIENTED_EDGE ( 'NONE', *, *, #48055, .T. ) ;
#6597 = VERTEX_POINT ( 'NONE', #33121 ) ;
#6598 = EDGE_CURVE ( 'NONE', #15615, #12505, #15492, .T. ) ;
#6599 = AXIS2_PLACEMENT_3D ( 'NONE', #30930, #42495, #26980 ) ;
#6600 = LINE ( 'NONE', #11021, #45659 ) ;
#6601 = CARTESIAN_POINT ( 'NONE',  ( -21.92638982964590255, -9.447133096874894775, 63.38080841974745283 ) ) ;
#6602 = DIRECTION ( 'NONE',  ( -0.000000000000000000, 1.000000000000000000, -0.000000000000000000 ) ) ;
#6603 = CARTESIAN_POINT ( 'NONE',  ( -24.40624982674571086, -15.81067781142186313, 73.09483948631277883 ) ) ;
#6604 = ORIENTED_EDGE ( 'NONE', *, *, #26674, .T. ) ;
#6605 = CARTESIAN_POINT ( 'NONE',  ( -18.13659385650551670, -6.915538690918074494, 49.31353937987644542 ) ) ;
#6606 = ORIENTED_EDGE ( 'NONE', *, *, #41925, .F. ) ;
#6607 = CARTESIAN_POINT ( 'NONE',  ( -22.02980920716174396, -20.08072702813828414, 62.23439177585281357 ) ) ;
#6608 = EDGE_CURVE ( 'NONE', #4181, #20377, #39503, .T. ) ;
#6609 = CARTESIAN_POINT ( 'NONE',  ( -50.42509385541305988, -6.359206544744109735, 49.44999999999998863 ) ) ;
#6610 = CARTESIAN_POINT ( 'NONE',  ( -10.46291082975850806, -15.97406517396614944, 61.19356052171543325 ) ) ;
#6611 = EDGE_CURVE ( 'NONE', #8331, #38907, #48160, .T. ) ;
#6612 = VERTEX_POINT ( 'NONE', #22065 ) ;
#6613 = EDGE_CURVE ( 'NONE', #5216, #48283, #3584, .T. ) ;
#6614 = CARTESIAN_POINT ( 'NONE',  ( -13.59269417415731063, -21.19935819725622039, 65.09973481642835225 ) ) ;
#6615 = CARTESIAN_POINT ( 'NONE',  ( -22.37667958203292784, -9.786583861647388360, 73.48161084599418302 ) ) ;
#6616 = CARTESIAN_POINT ( 'NONE',  ( -17.33262245845742910, -7.759502110702281463, 67.30567542699309058 ) ) ;
#6617 = EDGE_CURVE ( 'NONE', #43505, #25227, #44536, .T. ) ;
#6618 = CARTESIAN_POINT ( 'NONE',  ( -16.26184114368905043, -7.855670183028919062, 60.20028478909662795 ) ) ;
#6619 = ORIENTED_EDGE ( 'NONE', *, *, #34698, .T. ) ;
#6620 = DIRECTION ( 'NONE',  ( -0.2737502900231350011, -0.9618007999124593699, 5.400150802763565900E-08 ) ) ;
#6621 = ORIENTED_EDGE ( 'NONE', *, *, #45360, .T. ) ;
#6622 = AXIS2_PLACEMENT_3D ( 'NONE', #14535, #14063, #21497 ) ;
#6623 =( BOUNDED_CURVE ( )  B_SPLINE_CURVE ( 3, ( #5230, #39197, #39923, #21220 ),
 .UNSPECIFIED., .F., .F. ) 
 B_SPLINE_CURVE_WITH_KNOTS ( ( 4, 4 ),
 ( 0.9074455897393651771, 1.000000000000000000 ),
 .UNSPECIFIED. ) 
 CURVE ( )  GEOMETRIC_REPRESENTATION_ITEM ( )  RATIONAL_B_SPLINE_CURVE ( ( 0.6983129098261127155, 0.7760317562607151887, 0.8765941196520109502, 1.000000000000000000 ) ) 
 REPRESENTATION_ITEM ( '' )  );
#6624 = CARTESIAN_POINT ( 'NONE',  ( -17.42409385541299471, -14.80920654474435594, 52.02966884056656482 ) ) ;
#6625 = CARTESIAN_POINT ( 'NONE',  ( -17.64564815875613846, -7.362378996003227094, 63.72869765717685198 ) ) ;
#6626 = ORIENTED_EDGE ( 'NONE', *, *, #31229, .T. ) ;
#6627 = CARTESIAN_POINT ( 'NONE',  ( -20.43185948505062299, -8.432683554863363184, 66.79576150497511833 ) ) ;
#6628 = VECTOR ( 'NONE', #39400, 1000.000000000000000 ) ;
#6629 = CARTESIAN_POINT ( 'NONE',  ( -12.84615363328625826, -20.17103110633857455, 72.09181604382622766 ) ) ;
#6630 = ORIENTED_EDGE ( 'NONE', *, *, #22871, .T. ) ;
#6631 = CARTESIAN_POINT ( 'NONE',  ( -18.86498748457869468, -7.957467553504502078, 70.48141235020942474 ) ) ;
#6632 = B_SPLINE_CURVE_WITH_KNOTS ( 'NONE', 3,
 ( #47752, #13990, #6154, #32497, #36894, #40367, #17218, #33196, #10575, #47522 ),
 .UNSPECIFIED., .F., .F.,
 ( 4, 2, 2, 2, 4 ),
 ( 0.000000000000000000, 0.2500000000000000000, 0.5000000000000000000, 0.7500000000000000000, 1.000000000000000000 ),
 .UNSPECIFIED. ) ;
#6633 = CARTESIAN_POINT ( 'NONE',  ( 18.07590614458695200, 0.7899956341021162620, 50.77694869565811331 ) ) ;
#6634 = DIRECTION ( 'NONE',  ( -0.1240347345892086062, 1.145860353393066553E-16, -0.9922778767136676281 ) ) ;
#6635 = VERTEX_POINT ( 'NONE', #29450 ) ;
#6636 = DIRECTION ( 'NONE',  ( -3.071710424422018668E-17, 6.404604876783312462E-16, 1.000000000000000000 ) ) ;
#6637 = FACE_OUTER_BOUND ( 'NONE', #6807, .T. ) ;
#6638 = CARTESIAN_POINT ( 'NONE',  ( -23.00454255336054743, -10.50046069577333263, 59.88731295783226471 ) ) ;
#6639 = ORIENTED_EDGE ( 'NONE', *, *, #34501, .F. ) ;
#6640 = ORIENTED_EDGE ( 'NONE', *, *, #11617, .F. ) ;
#6641 = CARTESIAN_POINT ( 'NONE',  ( -11.84809292083425802, -10.57729547379942225, 71.19566414032826174 ) ) ;
#6642 = ORIENTED_EDGE ( 'NONE', *, *, #36773, .T. ) ;
#6643 = DIRECTION ( 'NONE',  ( -0.000000000000000000, -1.000000000000000000, -0.000000000000000000 ) ) ;
#6644 = CARTESIAN_POINT ( 'NONE',  ( -14.84909385759799072, -8.112991634885936776, 51.74999426922421719 ) ) ;
#6645 = CARTESIAN_POINT ( 'NONE',  ( -10.60570718526854961, -17.81143598018131158, 71.68222757358374508 ) ) ;
#6646 = EDGE_CURVE ( 'NONE', #6817, #36333, #5407, .T. ) ;
#6647 = CARTESIAN_POINT ( 'NONE',  ( -12.90353999865511625, -8.887351178413068098, 67.49447498869417927 ) ) ;
#6648 = CARTESIAN_POINT ( 'NONE',  ( -23.67325187062781566, -18.86515452381667757, 69.39397745686399332 ) ) ;
#6649 = DIRECTION ( 'NONE',  ( -0.9584484254710482487, -0.2852658684667118139, 3.516456354099036852E-08 ) ) ;
#6650 = VERTEX_POINT ( 'NONE', #395 ) ;
#6651 = CARTESIAN_POINT ( 'NONE',  ( -11.79630000206883977, -19.05592701419838519, 71.97213747039440079 ) ) ;
#6652 = CARTESIAN_POINT ( 'NONE',  ( -12.41315160057549960, -9.850077812919039388, 57.23935532239169532 ) ) ;
#6653 = DIRECTION ( 'NONE',  ( -0.9687793358424822143, 0.2479245821708672415, 0.000000000000000000 ) ) ;
#6654 = ORIENTED_EDGE ( 'NONE', *, *, #3524, .T. ) ;
#6655 = VECTOR ( 'NONE', #25659, 1000.000000000000114 ) ;
#6656 = VERTEX_POINT ( 'NONE', #14885 ) ;
#6657 = CARTESIAN_POINT ( 'NONE',  ( -45.92409385541305511, -15.80920654474410725, 70.50000000000000000 ) ) ;
#6658 = AXIS2_PLACEMENT_3D ( 'NONE', #1853, #5071, #13398 ) ;
#6659 = CARTESIAN_POINT ( 'NONE',  ( -23.64032756017451220, -11.59062047747720925, 63.17891664429986776 ) ) ;
#6660 = EDGE_CURVE ( 'NONE', #1656, #23182, #17248, .T. ) ;
#6661 = DIRECTION ( 'NONE',  ( 1.000000000000000000, 2.866981220435666553E-17, 0.000000000000000000 ) ) ;
#6662 = FACE_OUTER_BOUND ( 'NONE', #9758, .T. ) ;
#6663 = ORIENTED_EDGE ( 'NONE', *, *, #8009, .F. ) ;
#6664 = DIRECTION ( 'NONE',  ( 0.000000000000000000, 0.000000000000000000, 1.000000000000000000 ) ) ;
#6665 = ADVANCED_FACE ( 'NONE', ( #18592 ), #44728, .T. ) ;
#6666 = CARTESIAN_POINT ( 'NONE',  ( -23.82052202658861972, -17.65274426584190692, 59.19481648357778170 ) ) ;
#6667 = ORIENTED_EDGE ( 'NONE', *, *, #34772, .T. ) ;
#6668 = LINE ( 'NONE', #3451, #28418 ) ;
#6669 = ADVANCED_FACE ( 'NONE', ( #11713 ), #26243, .T. ) ;
#6670 = CARTESIAN_POINT ( 'NONE',  ( -19.69296339593938328, -21.90548865816194635, 65.62632728502332213 ) ) ;
#6671 = CARTESIAN_POINT ( 'NONE',  ( -23.20936678059565494, -18.85217346302747643, 59.03977614772677640 ) ) ;
#6672 = VERTEX_POINT ( 'NONE', #33863 ) ;
#6673 = DIRECTION ( 'NONE',  ( -5.731567514496413899E-31, -1.020425574103664789E-16, -1.000000000000000000 ) ) ;
#6674 = EDGE_LOOP ( 'NONE', ( #6177, #24953 ) ) ;
#6675 = DIRECTION ( 'NONE',  ( 1.000000000000000000, 2.866981220435666553E-17, 0.000000000000000000 ) ) ;
#6676 = B_SPLINE_CURVE_WITH_KNOTS ( 'NONE', 3,
 ( #31802, #38449, #23937, #5219, #12597, #27623, #19761, #1040, #42659, #35238 ),
 .UNSPECIFIED., .F., .F.,
 ( 4, 2, 2, 2, 4 ),
 ( 0.000000000000000000, 0.2500000000000000000, 0.5000000000000000000, 0.7500000000000000000, 1.000000000000000000 ),
 .UNSPECIFIED. ) ;
#6677 = CARTESIAN_POINT ( 'NONE',  ( -24.39889739404874192, -14.21436921164216116, 69.65275261046649291 ) ) ;
#6678 = ORIENTED_EDGE ( 'NONE', *, *, #5336, .T. ) ;
#6679 = CARTESIAN_POINT ( 'NONE',  ( -10.59656512619885227, -13.05092609425065397, 68.02360230423870746 ) ) ;
#6680 = CARTESIAN_POINT ( 'NONE',  ( -23.99887651489391871, -12.24265264118830387, 73.39792675737896843 ) ) ;
#6681 = DIRECTION ( 'NONE',  ( -3.413470714839332458E-33, 1.190614954331866791E-16, -1.000000000000000000 ) ) ;
#6682 = ADVANCED_FACE ( 'NONE', ( #26006 ), #41022, .T. ) ;
#6683 = CARTESIAN_POINT ( 'NONE',  ( -10.04932599622759248, -15.86565813568266492, 64.61497449378698832 ) ) ;
#6684 = CYLINDRICAL_SURFACE ( 'NONE', #33144, 2.000000000000001776 ) ;
#6685 = CARTESIAN_POINT ( 'NONE',  ( -12.38489527708928684, -19.74478370405832806, 58.13502342243108245 ) ) ;
#6686 = VERTEX_POINT ( 'NONE', #164 ) ;
#6687 = DIRECTION ( 'NONE',  ( -9.444166282346144476E-07, 1.975884201625194781E-06, 0.9999999999976019183 ) ) ;
#6688 = EDGE_CURVE ( 'NONE', #38712, #28574, #14261, .T. ) ;
#6689 = CARTESIAN_POINT ( 'NONE',  ( -10.39679176622870038, -14.24023819782134304, 64.40275955115841100 ) ) ;
#6690 = CARTESIAN_POINT ( 'NONE',  ( -22.63560516303400050, -20.13310814558360917, 69.28922553891734992 ) ) ;
#6691 = VECTOR ( 'NONE', #45489, 1000.000000000000000 ) ;
#6692 = CARTESIAN_POINT ( 'NONE',  ( -13.29845860553889203, -21.01266621750898267, 61.63151044148704472 ) ) ;
#6693 = CARTESIAN_POINT ( 'NONE',  ( -18.57019874455824393, -7.903669367688619829, 70.47953930074716311 ) ) ;
#6694 = EDGE_CURVE ( 'NONE', #19021, #6412, #36595, .T. ) ;
#6695 = CARTESIAN_POINT ( 'NONE',  ( -24.25486363958986757, -13.06355980472538469, 63.11792038370487035 ) ) ;
#6696 = AXIS2_PLACEMENT_3D ( 'NONE', #41097, #15897, #7380 ) ;
#6697 = VERTEX_POINT ( 'NONE', #23051 ) ;
#6698 = VERTEX_POINT ( 'NONE', #12433 ) ;
#6699 = DIRECTION ( 'NONE',  ( 0.000000000000000000, 1.000000000000000000, 0.000000000000000000 ) ) ;
#6700 = DIRECTION ( 'NONE',  ( 1.000000000000000000, -1.224646799147353207E-16, 6.695352868347749370E-17 ) ) ;
#6701 = ORIENTED_EDGE ( 'NONE', *, *, #26798, .F. ) ;
#6703 = DIRECTION ( 'NONE',  ( 0.8705373987491421550, -0.4921022631314296292, 4.758021987246392057E-08 ) ) ;
#6702 = CARTESIAN_POINT ( 'NONE',  ( -10.37818533259200748, -17.22973363664382873, 61.27247698181179913 ) ) ;
#6704 = CARTESIAN_POINT ( 'NONE',  ( -24.17271849214968071, -12.95015691860989371, 66.60246741689840633 ) ) ;
#6705 = CARTESIAN_POINT ( 'NONE',  ( -12.10131192688100477, -10.18592936015514638, 64.31442259820508411 ) ) ;
#6706 = CARTESIAN_POINT ( 'NONE',  ( -12.10599122619147749, -20.02663529450013513, 61.58173959111590534 ) ) ;
#6707 =( BOUNDED_CURVE ( )  B_SPLINE_CURVE ( 3, ( #3665, #239, #33679, #26821 ),
 .UNSPECIFIED., .F., .F. ) 
 B_SPLINE_CURVE_WITH_KNOTS ( ( 4, 4 ),
 ( 0.5000000000000000000, 0.9074455897393706172 ),
 .UNSPECIFIED. ) 
 CURVE ( )  GEOMETRIC_REPRESENTATION_ITEM ( )  RATIONAL_B_SPLINE_CURVE ( ( 1.000000000000017986, 0.4567392136813281378, 0.3561768502900162781, 0.6983129098261018353 ) ) 
 REPRESENTATION_ITEM ( '' )  );
#6708 = B_SPLINE_CURVE_WITH_KNOTS ( 'NONE', 3,
 ( #3464, #48043, #44601, #48521, #2081, #17082, #14756, #25629, #6019, #9731 ),
 .UNSPECIFIED., .F., .F.,
 ( 4, 2, 2, 2, 4 ),
 ( 0.000000000000000000, 0.2500000000000000000, 0.5000000000000000000, 0.7500000000000000000, 1.000000000000000000 ),
 .UNSPECIFIED. ) ;
#6709 = CARTESIAN_POINT ( 'NONE',  ( -23.86426264037124056, -17.55550176324236489, 66.17187017368655688 ) ) ;
#6710 = CARTESIAN_POINT ( 'NONE',  ( -11.46205946457914315, -19.27670325764784920, 71.86402743521411196 ) ) ;
#6711 = CARTESIAN_POINT ( 'NONE',  ( -20.82184643845504723, -8.178298495136663959, 63.49776821231386492 ) ) ;
#6712 = VERTEX_POINT ( 'NONE', #46666 ) ;
#6713 = CARTESIAN_POINT ( 'NONE',  ( -16.32575768948312600, -7.844986739114469643, 60.21500614002425777 ) ) ;
#6714 = CARTESIAN_POINT ( 'NONE',  ( -10.69992066440855361, -12.66433694503948004, 67.88265386532016521 ) ) ;
#6715 = CARTESIAN_POINT ( 'NONE',  ( -23.96075645138428101, -17.45014240273063066, 65.94357239682317129 ) ) ;
#6716 = CARTESIAN_POINT ( 'NONE',  ( -22.53375553849141610, -19.66661599265353644, 72.94400550747238299 ) ) ;
#6717 = CARTESIAN_POINT ( 'NONE',  ( -10.70297003644833644, -11.59513240183115279, 71.27356180636090244 ) ) ;
#6718 =( BOUNDED_SURFACE ( )  B_SPLINE_SURFACE ( 3, 1, ( 
 ( #19583, #33602 ),
 ( #23049, #14882 ),
 ( #11229, #162 ),
 ( #33861, #38270 ),
 ( #7790, #34103 ),
 ( #41996, #22547 ),
 ( #30197, #29946 ) ),
 .UNSPECIFIED., .T., .F., .F. ) 
 B_SPLINE_SURFACE_WITH_KNOTS ( ( 4, 3, 4 ),
 ( 2, 2 ),
 ( 0.000000000000000000, 0.5000000000000000000, 1.000000000000000000 ),
 ( 0.000000000000000000, 1.000000000000000000 ),
 .UNSPECIFIED. ) 
 GEOMETRIC_REPRESENTATION_ITEM ( )  RATIONAL_B_SPLINE_SURFACE ( (
 ( 1.000000000000000000, 1.000000000000000000),
 ( 0.3333333333333335369, 0.3333333333333330373),
 ( 0.3333333333333335369, 0.3333333333333330373),
 ( 1.000000000000000000, 1.000000000000000000),
 ( 0.3333333333333333703, 0.3333333333333333703),
 ( 0.3333333333333333703, 0.3333333333333333703),
 ( 1.000000000000000000, 1.000000000000000000) ) ) 
 REPRESENTATION_ITEM ( '' )  SURFACE ( )  );
#6719 = CARTESIAN_POINT ( 'NONE',  ( -16.44450502417200255, -21.74194820930941319, 65.33637549174824244 ) ) ;
#6720 =( BOUNDED_CURVE ( )  B_SPLINE_CURVE ( 3, ( #28601, #43628, #9888, #15491 ),
 .UNSPECIFIED., .F., .F. ) 
 B_SPLINE_CURVE_WITH_KNOTS ( ( 4, 4 ),
 ( 0.5000000000000000000, 0.9074455897393645110 ),
 .UNSPECIFIED. ) 
 CURVE ( )  GEOMETRIC_REPRESENTATION_ITEM ( )  RATIONAL_B_SPLINE_CURVE ( ( 1.000000000000031308, 0.4567392136813358539, 0.3561768502900097833, 0.6983129098260869583 ) ) 
 REPRESENTATION_ITEM ( '' )  );
#6721 = EDGE_LOOP ( 'NONE', ( #9698, #10674, #36944, #26915, #2651 ) ) ;
#6722 = ORIENTED_EDGE ( 'NONE', *, *, #35766, .F. ) ;
#6723 = CARTESIAN_POINT ( 'NONE',  ( -18.64284385541304445, -7.587656875400192291, 49.25157356644813689 ) ) ;
#6724 = ORIENTED_EDGE ( 'NONE', *, *, #5822, .F. ) ;
#6725 = DIRECTION ( 'NONE',  ( 0.000000000000000000, 0.000000000000000000, 1.000000000000000000 ) ) ;
#6726 = CARTESIAN_POINT ( 'NONE',  ( -23.99919889754976410, -17.21122886273513330, 69.71339796235052688 ) ) ;
#6727 = B_SPLINE_CURVE_WITH_KNOTS ( 'NONE', 3,
 ( #41654, #34976, #26640, #15522, #1494, #16250, #531, #31058, #42641, #16507 ),
 .UNSPECIFIED., .F., .F.,
 ( 4, 2, 2, 2, 4 ),
 ( 0.6272669072782977029, 0.7522669073001729823, 0.8772669073220482616, 1.002266907343923652, 1.127266907365798820 ),
 .UNSPECIFIED. ) ;
#6728 =( BOUNDED_SURFACE ( )  B_SPLINE_SURFACE ( 3, 1, ( 
 ( #35661, #31746 ),
 ( #35180, #43063 ),
 ( #42604, #27317 ),
 ( #1941, #23882 ),
 ( #34705, #38642 ),
 ( #15977, #16941 ),
 ( #31983, #46998 ) ),
 .UNSPECIFIED., .T., .F., .F. ) 
 B_SPLINE_SURFACE_WITH_KNOTS ( ( 4, 3, 4 ),
 ( 2, 2 ),
 ( 0.000000000000000000, 0.5000000000000000000, 1.000000000000000000 ),
 ( 0.000000000000000000, 1.000000000000000000 ),
 .UNSPECIFIED. ) 
 GEOMETRIC_REPRESENTATION_ITEM ( )  RATIONAL_B_SPLINE_SURFACE ( (
 ( 1.000000000000000000, 1.000000000000000000),
 ( 0.3333333333333335369, 0.3333333333333330373),
 ( 0.3333333333333335369, 0.3333333333333330373),
 ( 1.000000000000000000, 1.000000000000000000),
 ( 0.3333333333333333703, 0.3333333333333333703),
 ( 0.3333333333333333703, 0.3333333333333333703),
 ( 1.000000000000000000, 1.000000000000000000) ) ) 
 REPRESENTATION_ITEM ( '' )  SURFACE ( )  );
#6729 = AXIS2_PLACEMENT_3D ( 'NONE', #17775, #29365, #32804 ) ;
#6730 = EDGE_CURVE ( 'NONE', #43248, #1779, #42490, .T. ) ;
#6731 = CARTESIAN_POINT ( 'NONE',  ( -10.51729497052147977, -16.22293520194095606, 71.74750383215044280 ) ) ;
#6732 = CARTESIAN_POINT ( 'NONE',  ( -20.84119746710919330, -20.97572115929791892, 62.11471400470772863 ) ) ;
#6733 = ORIENTED_EDGE ( 'NONE', *, *, #14764, .F. ) ;
#6734 = EDGE_CURVE ( 'NONE', #8229, #33983, #36028, .T. ) ;
#6735 = CARTESIAN_POINT ( 'NONE',  ( -13.53325528467554406, -21.16256411608339150, 65.17124155742401115 ) ) ;
#6736 = CARTESIAN_POINT ( 'NONE',  ( -21.06634951290973845, -21.30826427787840771, 62.29966696806321380 ) ) ;
#6737 = ORIENTED_EDGE ( 'NONE', *, *, #44845, .T. ) ;
#6738 = CARTESIAN_POINT ( 'NONE',  ( -17.91451193640577344, -22.24313339626381847, 61.99040498927033127 ) ) ;
#6739 = B_SPLINE_CURVE_WITH_KNOTS ( 'NONE', 3,
 ( #11468, #18597, #41262, #44988, #7802, #11235, #33609, #40526, #36567, #25754 ),
 .UNSPECIFIED., .F., .F.,
 ( 4, 2, 2, 2, 4 ),
 ( 0.1272669073658314609, 0.2522669073463261746, 0.3772669073268208884, 0.5022669073073156021, 0.6272669072878103158 ),
 .UNSPECIFIED. ) ;
#6740 = CARTESIAN_POINT ( 'NONE',  ( -14.90981263331598150, -21.39562362703504306, 61.93600440604521395 ) ) ;
#6741 = VERTEX_POINT ( 'NONE', #12196 ) ;
#6742 = CARTESIAN_POINT ( 'NONE',  ( -23.46741908093438767, -19.16603997859080266, 62.53902161361033052 ) ) ;
#6743 = CARTESIAN_POINT ( 'NONE',  ( -10.05862351292959467, -15.92886012141397245, 64.69266982328383619 ) ) ;
#6744 = B_SPLINE_CURVE_WITH_KNOTS ( 'NONE', 3,
 ( #14441, #40572, #11284, #6852, #44532, #7601, #40823, #37112, #3395, #37602 ),
 .UNSPECIFIED., .F., .F.,
 ( 4, 2, 2, 2, 4 ),
 ( 0.000000000000000000, 0.2500000000000000000, 0.5000000000000000000, 0.7500000000000000000, 1.000000000000000000 ),
 .UNSPECIFIED. ) ;
#6745 = CARTESIAN_POINT ( 'NONE',  ( -22.84116833803633284, -10.28479860924217704, 59.75770304231562591 ) ) ;
#6746 = EDGE_LOOP ( 'NONE', ( #19195, #1390, #29201, #47397, #16087 ) ) ;
#6747 = CYLINDRICAL_SURFACE ( 'NONE', #31735, 4.686499999999997002 ) ;
#6748 = CARTESIAN_POINT ( 'NONE',  ( -24.41897112398753933, -17.37347453850100720, 69.59835118672229726 ) ) ;
#6749 = CARTESIAN_POINT ( 'NONE',  ( -15.07489227400421861, -21.40335501537338203, 65.10596683994182854 ) ) ;
#6750 = CARTESIAN_POINT ( 'NONE',  ( -22.22619359738691003, -20.50513629785891823, 58.94938195453792673 ) ) ;
#6751 = ORIENTED_EDGE ( 'NONE', *, *, #9565, .F. ) ;
#6752 = DIRECTION ( 'NONE',  ( 1.000000000000000000, 0.000000000000000000, 0.000000000000000000 ) ) ;
#6753 = CARTESIAN_POINT ( 'NONE',  ( -14.36038767613011302, -18.37140530287405582, 49.52966884056656482 ) ) ;
#6754 = EDGE_CURVE ( 'NONE', #17630, #4066, #1597, .T. ) ;
#6755 = CARTESIAN_POINT ( 'NONE',  ( -18.06825732353542335, -21.77950449724592730, 62.06639155695750532 ) ) ;
#6756 = EDGE_CURVE ( 'NONE', #14865, #33892, #46414, .T. ) ;
#6757 = EDGE_CURVE ( 'NONE', #43621, #44791, #10209, .T. ) ;
#6758 = CARTESIAN_POINT ( 'NONE',  ( -22.24284385650551954, -8.811426318492348031, 52.18089403414751359 ) ) ;
#6759 = EDGE_CURVE ( 'NONE', #34260, #14295, #15880, .T. ) ;
#6760 = CARTESIAN_POINT ( 'NONE',  ( -16.05890242020153380, -7.889590739215661230, 60.08539615417584656 ) ) ;
#6761 = CARTESIAN_POINT ( 'NONE',  ( -24.72811879990099726, -13.33785195616451169, 59.54923321989076612 ) ) ;
#6762 = VERTEX_POINT ( 'NONE', #8503 ) ;
#6763 = CARTESIAN_POINT ( 'NONE',  ( -24.34502428176253019, -17.56683243011407924, 66.12852677468319484 ) ) ;
#6764 = FACE_OUTER_BOUND ( 'NONE', #35682, .T. ) ;
#6765 = CARTESIAN_POINT ( 'NONE',  ( -22.20320178312271153, -19.92390373660361291, 65.70421731406698029 ) ) ;
#6766 = VERTEX_POINT ( 'NONE', #41998 ) ;
#6767 = CARTESIAN_POINT ( 'NONE',  ( -17.57409385541300395, -6.859212275519753099, 50.50378509014294792 ) ) ;
#6768 = AXIS2_PLACEMENT_3D ( 'NONE', #25204, #32812, #43441 ) ;
#6769 = ORIENTED_EDGE ( 'NONE', *, *, #11670, .T. ) ;
#6770 = ORIENTED_EDGE ( 'NONE', *, *, #22503, .F. ) ;
#6771 = VERTEX_POINT ( 'NONE', #30684 ) ;
#6772 = CARTESIAN_POINT ( 'NONE',  ( -23.15350085761965460, -9.941038866939328145, 54.02312124697527196 ) ) ;
#6773 = CARTESIAN_POINT ( 'NONE',  ( -23.74619265052512773, -11.68934008440960248, 62.95218278636777143 ) ) ;
#6774 = FACE_OUTER_BOUND ( 'NONE', #18468, .T. ) ;
#6775 = VERTEX_POINT ( 'NONE', #27701 ) ;
#6776 = ORIENTED_EDGE ( 'NONE', *, *, #7123, .F. ) ;
#6777 = CARTESIAN_POINT ( 'NONE',  ( -16.98659385650551812, -9.302874398569244363, 51.68646062012417985 ) ) ;
#6778 = B_SPLINE_CURVE_WITH_KNOTS ( 'NONE', 3,
 ( #20404, #38621, #5385, #35406, #8846, #23623, #20150, #23862, #24340, #34683 ),
 .UNSPECIFIED., .F., .F.,
 ( 4, 2, 2, 2, 4 ),
 ( 0.000000000000000000, 0.2500000000000000000, 0.5000000000000000000, 0.7500000000000000000, 1.000000000000000000 ),
 .UNSPECIFIED. ) ;
#6779 = EDGE_CURVE ( 'NONE', #784, #46311, #39591, .T. ) ;
#6780 = CARTESIAN_POINT ( 'NONE',  ( -22.34470957656571599, -19.78791530553215949, 69.47417989488683077 ) ) ;
#6781 = DIRECTION ( 'NONE',  ( 0.6264825908887947659, -0.7794354131762691873, 3.858680029754496192E-08 ) ) ;
#6782 = CARTESIAN_POINT ( 'NONE',  ( -17.83034385650551457, -9.794322478646142471, 51.19202720610083901 ) ) ;
#6783 = VERTEX_POINT ( 'NONE', #630 ) ;
#6784 = CARTESIAN_POINT ( 'NONE',  ( -24.35706380436459995, -15.77560588608014136, 69.83307488757523629 ) ) ;
#6785 = EDGE_CURVE ( 'NONE', #40811, #48635, #11967, .T. ) ;
#6786 = CARTESIAN_POINT ( 'NONE',  ( -20.66696855643225916, -21.06909979829503854, 58.94475164909854925 ) ) ;
#6787 = CARTESIAN_POINT ( 'NONE',  ( -21.36489355414517632, -8.963473290115421932, 73.90128753234840531 ) ) ;
#6788 = EDGE_LOOP ( 'NONE', ( #10456, #40530, #1033, #17296, #12189 ) ) ;
#6789 = CARTESIAN_POINT ( 'NONE',  ( -11.24765530704275385, -11.51409840800856621, 67.90248063513186594 ) ) ;
#6790 = CIRCLE ( 'NONE', #18580, 0.5000000000000004441 ) ;
#6791 = ORIENTED_EDGE ( 'NONE', *, *, #42576, .F. ) ;
#6792 = CARTESIAN_POINT ( 'NONE',  ( -22.44463050228041467, -9.931189664211119705, 73.49663562641346459 ) ) ;
#6793 = CARTESIAN_POINT ( 'NONE',  ( -10.11671990330600579, -16.26064306581185903, 71.57033522450831242 ) ) ;
#6794 = CARTESIAN_POINT ( 'NONE',  ( -21.55974298755023000, -21.00590022698144921, 72.72457636846944240 ) ) ;
#6795 = ORIENTED_EDGE ( 'NONE', *, *, #14224, .T. ) ;
#6796 = FACE_OUTER_BOUND ( 'NONE', #15142, .T. ) ;
#6797 = CARTESIAN_POINT ( 'NONE',  ( -24.18217652367932047, -11.67366674157813122, 59.67509901561481911 ) ) ;
#6798 =( BOUNDED_CURVE ( )  B_SPLINE_CURVE ( 3, ( #36683, #14280, #29568, #24915 ),
 .UNSPECIFIED., .F., .F. ) 
 B_SPLINE_CURVE_WITH_KNOTS ( ( 4, 4 ),
 ( 0.4074455897393635673, 0.5000000000000000000 ),
 .UNSPECIFIED. ) 
 CURVE ( )  GEOMETRIC_REPRESENTATION_ITEM ( )  RATIONAL_B_SPLINE_CURVE ( ( 0.6983129098260953960, 0.7760317562607027542, 0.8765941196520051770, 1.000000000000004219 ) ) 
 REPRESENTATION_ITEM ( '' )  );
#6799 = CARTESIAN_POINT ( 'NONE',  ( -13.17078218117215549, -9.186392337449538203, 67.39414915108072535 ) ) ;
#6800 = CARTESIAN_POINT ( 'NONE',  ( -24.30537484439201990, -16.09989820848641173, 66.13495298149886992 ) ) ;
#6801 = ORIENTED_EDGE ( 'NONE', *, *, #30149, .F. ) ;
#6802 = CARTESIAN_POINT ( 'NONE',  ( -24.83421645677935174, -15.58062944684732365, 73.16337087059751809 ) ) ;
#6803 = LINE ( 'NONE', #18859, #34437 ) ;
#6804 = DIRECTION ( 'NONE',  ( 0.5351595679979623821, 0.8447509909909748371, 0.000000000000000000 ) ) ;
#6805 = VERTEX_POINT ( 'NONE', #26975 ) ;
#6806 = CARTESIAN_POINT ( 'NONE',  ( -15.14522032754860703, -21.97383469840033854, 53.76227901944321275 ) ) ;
#6807 = EDGE_LOOP ( 'NONE', ( #35182, #11770 ) ) ;
#6808 = ADVANCED_FACE ( 'NONE', ( #19585 ), #5855, .T. ) ;
#6809 = EDGE_CURVE ( 'NONE', #17056, #44664, #10882, .T. ) ;
#6810 = CARTESIAN_POINT ( 'NONE',  ( -13.93897074462874919, -20.93787812888889377, 68.74153005185598886 ) ) ;
#6811 = CARTESIAN_POINT ( 'NONE',  ( -42.54285765631804139, -14.90920654474416907, 62.04988959276017368 ) ) ;
#6812 = CARTESIAN_POINT ( 'NONE',  ( -22.65633733904555669, -10.15891943096868744, 70.01178531762562329 ) ) ;
#6813 = ORIENTED_EDGE ( 'NONE', *, *, #34483, .T. ) ;
#6814 = CARTESIAN_POINT ( 'NONE',  ( -10.45863951484398946, -14.11462368554138536, 60.91821294131582931 ) ) ;
#6815 = ORIENTED_EDGE ( 'NONE', *, *, #42546, .F. ) ;
#6816 = CARTESIAN_POINT ( 'NONE',  ( -17.42409385541299471, -14.80920654474435771, 49.52966884056655772 ) ) ;
#6817 = VERTEX_POINT ( 'NONE', #39751 ) ;
#6818 = CARTESIAN_POINT ( 'NONE',  ( -11.20499100338089349, -18.91108562151346462, 64.84683437277969631 ) ) ;
#6819 = EDGE_CURVE ( 'NONE', #3087, #16476, #9346, .T. ) ;
#6820 = ADVANCED_FACE ( 'NONE', ( #32129 ), #9489, .T. ) ;
#6821 = LINE ( 'NONE', #24587, #25142 ) ;
#6822 = ORIENTED_EDGE ( 'NONE', *, *, #12122, .F. ) ;
#6823 = ORIENTED_EDGE ( 'NONE', *, *, #7776, .F. ) ;
#6824 = EDGE_CURVE ( 'NONE', #4227, #29981, #17485, .T. ) ;
#6825 = LINE ( 'NONE', #18374, #5270 ) ;
#6826 = DIRECTION ( 'NONE',  ( -0.000000000000000000, -1.000000000000000000, -0.000000000000000000 ) ) ;
#6827 = CARTESIAN_POINT ( 'NONE',  ( -23.47587192523704047, -19.15443292186558111, 62.51440210027411837 ) ) ;
#6828 = CARTESIAN_POINT ( 'NONE',  ( -12.31054147697317802, -19.59141247267844932, 61.46848823829365216 ) ) ;
#6829 = DIRECTION ( 'NONE',  ( -1.000000000000000000, -2.866981220435666553E-17, -0.000000000000000000 ) ) ;
#6830 = CARTESIAN_POINT ( 'NONE',  ( -17.77594298899184366, -7.367433885636743618, 60.26556189360973548 ) ) ;
#6831 = VECTOR ( 'NONE', #16278, 1000.000000000000114 ) ;
#6832 = AXIS2_PLACEMENT_3D ( 'NONE', #11954, #38521, #23277 ) ;
#6833 = ORIENTED_EDGE ( 'NONE', *, *, #33578, .T. ) ;
#6834 = ORIENTED_EDGE ( 'NONE', *, *, #7030, .F. ) ;
#6835 = PLANE ( 'NONE',  #24970 ) ;
#6836 = ADVANCED_FACE ( 'NONE', ( #27937 ), #43705, .T. ) ;
#6837 = CARTESIAN_POINT ( 'NONE',  ( -50.42609385541305755, -14.90920654474428630, 74.09999999999998010 ) ) ;
#6838 = CARTESIAN_POINT ( 'NONE',  ( -23.65624057141236847, -11.51332318074561911, 66.72214514605295221 ) ) ;
#6839 = DIRECTION ( 'NONE',  ( 1.295331059719046080E-06, -6.890485863767693062E-07, -0.9999999999989236388 ) ) ;
#6840 = FACE_OUTER_BOUND ( 'NONE', #23619, .T. ) ;
#6841 = ORIENTED_EDGE ( 'NONE', *, *, #45027, .F. ) ;
#6842 = CARTESIAN_POINT ( 'NONE',  ( -17.85534385650552025, -7.417179338643134834, 52.18511593390279302 ) ) ;
#6843 = ORIENTED_EDGE ( 'NONE', *, *, #48198, .T. ) ;
#6844 = CYLINDRICAL_SURFACE ( 'NONE', #9162, 0.1499999999999977185 ) ;
#6845 = DIRECTION ( 'NONE',  ( -0.5420872618288283817, -0.8403222004463036798, 7.592316861452270591E-08 ) ) ;
#6846 = FACE_OUTER_BOUND ( 'NONE', #34814, .T. ) ;
#6847 = DIRECTION ( 'NONE',  ( -3.549360974551883545E-17, 6.371834667872732552E-18, 1.000000000000000000 ) ) ;
#6848 = B_SPLINE_CURVE_WITH_KNOTS ( 'NONE', 3,
 ( #39132, #3342, #46774, #14629, #9355, #10729, #36807, #39382, #44725, #20677 ),
 .UNSPECIFIED., .F., .F.,
 ( 4, 2, 2, 2, 4 ),
 ( 0.000000000000000000, 0.2500000000000000000, 0.5000000000000000000, 0.7500000000000000000, 1.000000000000000000 ),
 .UNSPECIFIED. ) ;
#6849 =( BOUNDED_CURVE ( )  B_SPLINE_CURVE ( 3, ( #4769, #12387, #19295, #16557 ),
 .UNSPECIFIED., .F., .F. ) 
 B_SPLINE_CURVE_WITH_KNOTS ( ( 4, 4 ),
 ( 0.4074455897393655657, 0.5000000000000000000 ),
 .UNSPECIFIED. ) 
 CURVE ( )  GEOMETRIC_REPRESENTATION_ITEM ( )  RATIONAL_B_SPLINE_CURVE ( ( 0.6983129098260966172, 0.7760317562606876551, 0.8765941196519846379, 0.9999999999999783507 ) ) 
 REPRESENTATION_ITEM ( '' )  );
#6850 = ORIENTED_EDGE ( 'NONE', *, *, #43579, .T. ) ;
#6851 = CARTESIAN_POINT ( 'NONE',  ( -11.56806251476610115, -18.73522173559940995, 65.03234934376791898 ) ) ;
#6852 = CARTESIAN_POINT ( 'NONE',  ( -21.54646308099719931, -9.151741662630445973, 66.73437983189968747 ) ) ;
#6853 = ORIENTED_EDGE ( 'NONE', *, *, #41449, .T. ) ;
#6854 = CARTESIAN_POINT ( 'NONE',  ( -15.23980195177804831, -21.45974831136452110, 65.17884789245921695 ) ) ;
#6855 = EDGE_CURVE ( 'NONE', #12959, #27894, #19565, .T. ) ;
#6856 = CARTESIAN_POINT ( 'NONE',  ( -6.795509042373261366, -13.90955010341581044, 54.49999999999995026 ) ) ;
#6857 = ORIENTED_EDGE ( 'NONE', *, *, #3068, .F. ) ;
#6858 = CARTESIAN_POINT ( 'NONE',  ( -17.92193066645248578, -21.84160715981037981, 62.02535923543162966 ) ) ;
#6859 =( BOUNDED_SURFACE ( )  B_SPLINE_SURFACE ( 3, 1, ( 
 ( #16155, #19880 ),
 ( #1150, #16403 ),
 ( #4610, #11766 ),
 ( #41808, #27741 ),
 ( #8089, #1388 ),
 ( #34153, #38088 ),
 ( #4369, #45759 ) ),
 .UNSPECIFIED., .T., .F., .F. ) 
 B_SPLINE_SURFACE_WITH_KNOTS ( ( 4, 3, 4 ),
 ( 2, 2 ),
 ( 0.000000000000000000, 0.5000000000000000000, 1.000000000000000000 ),
 ( 0.000000000000000000, 1.000000000000000000 ),
 .UNSPECIFIED. ) 
 GEOMETRIC_REPRESENTATION_ITEM ( )  RATIONAL_B_SPLINE_SURFACE ( (
 ( 1.000000000000000000, 1.000000000000000000),
 ( 0.3333333333333335369, 0.3333333333333330373),
 ( 0.3333333333333335369, 0.3333333333333330373),
 ( 1.000000000000000000, 1.000000000000000000),
 ( 0.3333333333333333703, 0.3333333333333333703),
 ( 0.3333333333333333703, 0.3333333333333333703),
 ( 1.000000000000000000, 1.000000000000000000) ) ) 
 REPRESENTATION_ITEM ( '' )  SURFACE ( )  );
#6860 = AXIS2_PLACEMENT_3D ( 'NONE', #43489, #21321, #28692 ) ;
#6861 = AXIS2_PLACEMENT_3D ( 'NONE', #32934, #47976, #36149 ) ;
#6862 = ORIENTED_EDGE ( 'NONE', *, *, #1030, .F. ) ;
#6863 = CARTESIAN_POINT ( 'NONE',  ( -24.72409385541305582, -14.90920654474422058, 68.96470588235293064 ) ) ;
#6864 = CARTESIAN_POINT ( 'NONE',  ( -18.66311988809301425, -7.868636481342422329, 70.65595886192740238 ) ) ;
#6865 = EDGE_LOOP ( 'NONE', ( #36834, #32445, #18625, #13590 ) ) ;
#6866 = EDGE_CURVE ( 'NONE', #33816, #45314, #16183, .T. ) ;
#6867 = DIRECTION ( 'NONE',  ( -1.616182858256117057E-16, -0.003028072113818697231, 0.9999954153791273948 ) ) ;
#6868 = CARTESIAN_POINT ( 'NONE',  ( -20.24469356570329737, -8.402152009130100296, 70.53483737320162561 ) ) ;
#6869 = EDGE_LOOP ( 'NONE', ( #23322, #29989, #351, #30970, #2624 ) ) ;
#6870 = FACE_OUTER_BOUND ( 'NONE', #7313, .T. ) ;
#6871 = VECTOR ( 'NONE', #17068, 1000.000000000000000 ) ;
#6872 = CARTESIAN_POINT ( 'NONE',  ( -19.77435985551070274, -21.87886194922281646, 65.64981515446680760 ) ) ;
#6873 = CARTESIAN_POINT ( 'NONE',  ( -21.63003847667031820, -8.659812987350562707, 73.74095428391912321 ) ) ;
#6874 = ORIENTED_EDGE ( 'NONE', *, *, #48193, .F. ) ;
#6875 = DIRECTION ( 'NONE',  ( -3.071710424422018668E-17, 6.404604876783312462E-16, 1.000000000000000000 ) ) ;
#6876 = EDGE_CURVE ( 'NONE', #30431, #29199, #35567, .T. ) ;
#6877 = CARTESIAN_POINT ( 'NONE',  ( -21.82233664355339542, -16.46178511230714037, 49.52966884056655772 ) ) ;
#6878 = CARTESIAN_POINT ( 'NONE',  ( -17.42409385541299471, -14.80920654474435771, 49.52966884056655772 ) ) ;
#6879 = ORIENTED_EDGE ( 'NONE', *, *, #5549, .T. ) ;
#6880 = ORIENTED_EDGE ( 'NONE', *, *, #3825, .T. ) ;
#6881 = EDGE_CURVE ( 'NONE', #30739, #25120, #36319, .T. ) ;
#6882 = CARTESIAN_POINT ( 'NONE',  ( -15.80034074178659331, -19.80179363221599687, 50.77966884056656482 ) ) ;
#6883 = CARTESIAN_POINT ( 'NONE',  ( -16.93008532196563820, -7.826600119876228057, 73.97520714747764714 ) ) ;
#6884 = PLANE ( 'NONE',  #40624 ) ;
#6885 = CARTESIAN_POINT ( 'NONE',  ( -15.07409385759798859, -6.859212275519751323, 50.50378509014259265 ) ) ;
#6886 = EDGE_CURVE ( 'NONE', #46504, #39476, #28909, .T. ) ;
#6887 = PLANE ( 'NONE',  #2975 ) ;
#6888 = CARTESIAN_POINT ( 'NONE',  ( -12.84691039585993444, -8.931012183600500975, 67.56438067310742213 ) ) ;
#6889 = CARTESIAN_POINT ( 'NONE',  ( -15.55171241031346696, -7.598245096497682205, 70.79485117658632021 ) ) ;
#6890 = CARTESIAN_POINT ( 'NONE',  ( -14.66287603173356757, -8.376693951416614325, 63.78978834288939481 ) ) ;
#6891 = ORIENTED_EDGE ( 'NONE', *, *, #23324, .F. ) ;
#6892 = DIRECTION ( 'NONE',  ( -0.5729733056696844073, 0.8195740302071246042, 7.403245352187747277E-08 ) ) ;
#6893 = AXIS2_PLACEMENT_3D ( 'NONE', #20975, #32308, #7178 ) ;
#6894 = CARTESIAN_POINT ( 'NONE',  ( -48.17409385541305511, -14.80920654474410547, 61.49999999999999289 ) ) ;
#6895 = CARTESIAN_POINT ( 'NONE',  ( -13.53206638028301434, -8.990422041175579082, 60.72333783371806248 ) ) ;
#6896 = ORIENTED_EDGE ( 'NONE', *, *, #34020, .F. ) ;
#6897 = EDGE_LOOP ( 'NONE', ( #35135, #6316, #21399, #30806, #43864 ) ) ;
#6898 = CYLINDRICAL_SURFACE ( 'NONE', #41419, 1.049999999999998934 ) ;
#6899 = DIRECTION ( 'NONE',  ( -3.071710424422018668E-17, 6.404604876783312462E-16, 1.000000000000000000 ) ) ;
#6900 = CARTESIAN_POINT ( 'NONE',  ( -23.35165829388149561, -19.32240830869099923, 59.04443984693184433 ) ) ;
#6901 = CARTESIAN_POINT ( 'NONE',  ( -24.31482301288783887, -13.31912224170856796, 59.66267924674055223 ) ) ;
#6902 = CIRCLE ( 'NONE', #18666, 1.999999999999999112 ) ;
#6903 = ORIENTED_EDGE ( 'NONE', *, *, #9565, .T. ) ;
#6904 = VECTOR ( 'NONE', #7689, 1000.000000000000114 ) ;
#6905 = CARTESIAN_POINT ( 'NONE',  ( -13.54792730259346456, -8.920061342218058797, 57.25495614889487683 ) ) ;
#6906 = FACE_OUTER_BOUND ( 'NONE', #24024, .T. ) ;
#6907 = ORIENTED_EDGE ( 'NONE', *, *, #17076, .T. ) ;
#6908 = LINE ( 'NONE', #40881, #4073 ) ;
#6909 = CARTESIAN_POINT ( 'NONE',  ( -21.73853604213786639, -16.63919858500264937, 49.52966884056655772 ) ) ;
#6910 = CARTESIAN_POINT ( 'NONE',  ( -10.88209242003807908, -17.29963164818252608, 64.62739380462950578 ) ) ;
#6911 = EDGE_CURVE ( 'NONE', #48283, #4125, #47087, .T. ) ;
#6912 = ORIENTED_EDGE ( 'NONE', *, *, #3335, .F. ) ;
#6913 = CARTESIAN_POINT ( 'NONE',  ( -24.12942661661615418, -12.79921782163564004, 70.07243032623514978 ) ) ;
#6914 = ORIENTED_EDGE ( 'NONE', *, *, #17197, .T. ) ;
#6915 = CARTESIAN_POINT ( 'NONE',  ( -19.49109506855409180, -21.54969648977046148, 62.28031529404344013 ) ) ;
#6916 = CARTESIAN_POINT ( 'NONE',  ( -23.66739264960602540, -11.53441051760089842, 66.42214525760398658 ) ) ;
#6917 = VERTEX_POINT ( 'NONE', #35801 ) ;
#6918 = CARTESIAN_POINT ( 'NONE',  ( -24.18037300165767434, -17.94870813986570113, 59.18873840842728384 ) ) ;
#6919 = CARTESIAN_POINT ( 'NONE',  ( -10.44916039635137039, -15.83526825291551177, 64.50771589744864798 ) ) ;
#6920 = CARTESIAN_POINT ( 'NONE',  ( -22.61159385650551457, -6.922745924619793101, 51.69366785382590024 ) ) ;
#6921 = CIRCLE ( 'NONE', #21094, 5.249999999999998224 ) ;
#6922 = CARTESIAN_POINT ( 'NONE',  ( -33.52409385541305653, -6.359206544744109735, 52.29999999999998295 ) ) ;
#6923 = VECTOR ( 'NONE', #34977, 1000.000000000000114 ) ;
#6924 = CARTESIAN_POINT ( 'NONE',  ( -24.26435699358934883, -17.76123410301217120, 62.51715077956382771 ) ) ;
#6925 = CARTESIAN_POINT ( 'NONE',  ( -22.86648298414092650, -19.29628210902822261, 58.97590826583130763 ) ) ;
#6926 = DIRECTION ( 'NONE',  ( 0.000000000000000000, 0.000000000000000000, 1.000000000000000000 ) ) ;
#6927 = ORIENTED_EDGE ( 'NONE', *, *, #20467, .T. ) ;
#6928 = CARTESIAN_POINT ( 'NONE',  ( -24.87238774844131584, -14.64917985650991206, 62.81322232226264646 ) ) ;
#6929 = AXIS2_PLACEMENT_3D ( 'NONE', #9965, #5561, #35807 ) ;
#6930 = VECTOR ( 'NONE', #46243, 1000.000000000000000 ) ;
#6931 = CARTESIAN_POINT ( 'NONE',  ( -10.70566838141854404, -16.94585318031169763, 57.83760548748448116 ) ) ;
#6932 = DIRECTION ( 'NONE',  ( -3.071710424422018668E-17, 6.404604876783312462E-16, 1.000000000000000000 ) ) ;
#6933 = DIRECTION ( 'NONE',  ( -1.420801289120338746E-06, -1.008342286982562053E-05, 0.9999999999481529178 ) ) ;
#6934 = CARTESIAN_POINT ( 'NONE',  ( -16.26195973558533936, -21.76306465430365122, 58.57113428431811997 ) ) ;
#6935 = CARTESIAN_POINT ( 'NONE',  ( -14.14284385650552167, -8.811426318492348031, 52.18089403414752070 ) ) ;
#6936 = VERTEX_POINT ( 'NONE', #28440 ) ;
#6937 = VERTEX_POINT ( 'NONE', #21295 ) ;
#6938 = EDGE_CURVE ( 'NONE', #40783, #40793, #3025, .T. ) ;
#6939 = FACE_OUTER_BOUND ( 'NONE', #7012, .T. ) ;
#6940 = DIRECTION ( 'NONE',  ( -3.071710424422018668E-17, 6.404604876783312462E-16, 1.000000000000000000 ) ) ;
#6941 = ORIENTED_EDGE ( 'NONE', *, *, #13388, .T. ) ;
#6943 = CARTESIAN_POINT ( 'NONE',  ( -20.72574062298286535, -8.580111251864035893, 59.84125250080548142 ) ) ;
#6942 = CARTESIAN_POINT ( 'NONE',  ( -15.56465948913149333, -7.543361525925791788, 53.27966884056655061 ) ) ;
#6944 = CARTESIAN_POINT ( 'NONE',  ( -15.32650908999326411, -21.54008551964724560, 68.87033137010456585 ) ) ;
#6945 = VECTOR ( 'NONE', #45724, 1000.000000000000000 ) ;
#6946 = CARTESIAN_POINT ( 'NONE',  ( -11.65778227265581712, -18.77778952248012345, 64.85592980783576422 ) ) ;
#6947 = EDGE_CURVE ( 'NONE', #33004, #32745, #28438, .T. ) ;
#6948 = CARTESIAN_POINT ( 'NONE',  ( -12.41310947992116098, -19.76871611099698001, 61.68206578716802113 ) ) ;
#6949 = FACE_BOUND ( 'NONE', #26041, .T. ) ;
#6950 = DIRECTION ( 'NONE',  ( 1.000000000000000000, 0.000000000000000000, 0.000000000000000000 ) ) ;
#6951 = FACE_OUTER_BOUND ( 'NONE', #6294, .T. ) ;
#6952 = EDGE_CURVE ( 'NONE', #15253, #12237, #32522, .T. ) ;
#6953 = CARTESIAN_POINT ( 'NONE',  ( 18.46573386768564973, 2.137037847100790255, 51.75577699556767897 ) ) ;
#6954 = VERTEX_POINT ( 'NONE', #44430 ) ;
#6955 = CARTESIAN_POINT ( 'NONE',  ( -24.12380779853282675, -11.55065473049533686, 63.13031021406904841 ) ) ;
#6956 = CARTESIAN_POINT ( 'NONE',  ( -42.66665856129541368, -14.90920654474415841, 61.05948235294116699 ) ) ;
#6957 = FACE_OUTER_BOUND ( 'NONE', #47813, .T. ) ;
#6958 = CARTESIAN_POINT ( 'NONE',  ( -21.89826263122328953, -8.852228171720549099, 66.84645388252840803 ) ) ;
#6959 = ADVANCED_FACE ( 'NONE', ( #4038 ), #7249, .T. ) ;
#6960 = LINE ( 'NONE', #38875, #27567 ) ;
#6961 = CARTESIAN_POINT ( 'NONE',  ( -16.09877598409873656, -7.881120331165020865, 67.44007573990704429 ) ) ;
#6962 = EDGE_CURVE ( 'NONE', #43029, #34970, #3293, .T. ) ;
#6963 = EDGE_LOOP ( 'NONE', ( #47608, #33860 ) ) ;
#6964 = VERTEX_POINT ( 'NONE', #19043 ) ;
#6965 = CARTESIAN_POINT ( 'NONE',  ( -15.09909385541304339, -8.105421454601382081, 49.25000573077640098 ) ) ;
#6966 = VERTEX_POINT ( 'NONE', #40965 ) ;
#6967 = CARTESIAN_POINT ( 'NONE',  ( -17.35317073117489173, -7.359421519614389062, 67.14226862839939258 ) ) ;
#6968 = VECTOR ( 'NONE', #14827, 1000.000000000000114 ) ;
#6969 = CARTESIAN_POINT ( 'NONE',  ( -18.71951286714620011, -7.876189896296080128, 66.78582905748461940 ) ) ;
#6970 = VECTOR ( 'NONE', #18618, 1000.000000000000000 ) ;
#6971 = AXIS2_PLACEMENT_3D ( 'NONE', #45237, #45473, #26023 ) ;
#6972 = LINE ( 'NONE', #10434, #41039 ) ;
#6973 = CARTESIAN_POINT ( 'NONE',  ( -9.974215871585233373, -14.86485004610319827, 74.91283608227215041 ) ) ;
#6974 = VERTEX_POINT ( 'NONE', #7494 ) ;
#6975 = CARTESIAN_POINT ( 'NONE',  ( -13.11946000997128436, -9.225961346166455357, 67.52942785706356688 ) ) ;
#6976 = CARTESIAN_POINT ( 'NONE',  ( -22.07446999803020660, -20.10798665040887556, 62.23439171591935093 ) ) ;
#6977 = EDGE_LOOP ( 'NONE', ( #46460, #5730, #37325, #740 ) ) ;
#6978 = DIRECTION ( 'NONE',  ( -3.071710424422018668E-17, 6.404604876783312462E-16, 1.000000000000000000 ) ) ;
#6979 = EDGE_CURVE ( 'NONE', #29080, #17056, #41360, .T. ) ;
#6980 = CARTESIAN_POINT ( 'NONE',  ( -41.55277032600130127, -14.80920654474423159, 69.97058823529410176 ) ) ;
#6981 = ORIENTED_EDGE ( 'NONE', *, *, #6033, .T. ) ;
#6982 = CARTESIAN_POINT ( 'NONE',  ( -19.23170823189057543, -21.62663761134119156, 62.40992444795293892 ) ) ;
#6983 = CARTESIAN_POINT ( 'NONE',  ( -20.89619716791787596, -20.95408004043368067, 69.19883325555726117 ) ) ;
#6984 = CYLINDRICAL_SURFACE ( 'NONE', #6121, 5.249999999999998224 ) ;
#6985 = EDGE_LOOP ( 'NONE', ( #45054, #13090, #35602, #32160, #6912, #30278, #27834, #297 ) ) ;
#6986 = CARTESIAN_POINT ( 'NONE',  ( -17.72634075389897035, -21.85272461700124680, 58.55553378267870812 ) ) ;
#6987 = CARTESIAN_POINT ( 'NONE',  ( -24.39403741458288266, -17.44049236422942784, 69.52844466935830781 ) ) ;
#6988 =( BOUNDED_SURFACE ( )  B_SPLINE_SURFACE ( 3, 1, ( 
 ( #42877, #24655 ),
 ( #31546, #1753 ),
 ( #9387, #9641 ),
 ( #43114, #20473 ),
 ( #1988, #1501 ),
 ( #16981, #8907 ),
 ( #20949, #24407 ) ),
 .UNSPECIFIED., .T., .F., .F. ) 
 B_SPLINE_SURFACE_WITH_KNOTS ( ( 4, 3, 4 ),
 ( 2, 2 ),
 ( 0.000000000000000000, 0.5000000000000000000, 1.000000000000000000 ),
 ( 0.000000000000000000, 1.000000000000000000 ),
 .UNSPECIFIED. ) 
 GEOMETRIC_REPRESENTATION_ITEM ( )  RATIONAL_B_SPLINE_SURFACE ( (
 ( 1.000000000000000000, 1.000000000000000000),
 ( 0.3333333333333335369, 0.3333333333333330373),
 ( 0.3333333333333335369, 0.3333333333333330373),
 ( 1.000000000000000000, 1.000000000000000000),
 ( 0.3333333333333333703, 0.3333333333333333703),
 ( 0.3333333333333333703, 0.3333333333333333703),
 ( 1.000000000000000000, 1.000000000000000000) ) ) 
 REPRESENTATION_ITEM ( '' )  SURFACE ( )  );
#6989 = CARTESIAN_POINT ( 'NONE',  ( -14.97037705864080337, -21.36678033093551221, 65.21669700154754423 ) ) ;
#6990 = FACE_OUTER_BOUND ( 'NONE', #43084, .T. ) ;
#6991 = ORIENTED_EDGE ( 'NONE', *, *, #15656, .T. ) ;
#6992 = CARTESIAN_POINT ( 'NONE',  ( -40.92409385541305511, -14.80920654474410725, 74.99999999999998579 ) ) ;
#6993 = EDGE_CURVE ( 'NONE', #2344, #11451, #22528, .T. ) ;
#6994 = CYLINDRICAL_SURFACE ( 'NONE', #5830, 0.1500000000000067668 ) ;
#6995 = CARTESIAN_POINT ( 'NONE',  ( -23.37999588001404661, -18.58199455739222827, 69.57899840282863124 ) ) ;
#6996 = CARTESIAN_POINT ( 'NONE',  ( -22.74909385650551386, -8.104110260919577868, 48.81699501597546487 ) ) ;
#6997 = ORIENTED_EDGE ( 'NONE', *, *, #23807, .F. ) ;
#6998 = B_SPLINE_CURVE_WITH_KNOTS ( 'NONE', 3,
 ( #10980, #41017, #29943, #14385, #22301, #11227, #7299, #44005, #29206, #10258 ),
 .UNSPECIFIED., .F., .F.,
 ( 4, 2, 2, 2, 4 ),
 ( 0.6272669072878331864, 0.7522669073073295909, 0.8772669073268261064, 1.002266907346322622, 1.127266907365819026 ),
 .UNSPECIFIED. ) ;
#6999 = DIRECTION ( 'NONE',  ( 6.651268170491444817E-06, 3.577353459756793540E-06, 0.9999999999714814791 ) ) ;
#7000 = CARTESIAN_POINT ( 'NONE',  ( -24.38570565625541064, -13.64691002463509939, 59.50701104079105619 ) ) ;
#7001 = ORIENTED_EDGE ( 'NONE', *, *, #40614, .F. ) ;
#7002 = CARTESIAN_POINT ( 'NONE',  ( -19.22579309969192707, -21.57336792462666253, 58.52507384993226225 ) ) ;
#7003 = PRODUCT_DEFINITION_FORMATION_WITH_SPECIFIED_SOURCE ( 'ANY', '', #38600, .NOT_KNOWN. ) ;
#7004 = CARTESIAN_POINT ( 'NONE',  ( -24.47401588851211329, -14.84236380343934592, 59.24300237059242136 ) ) ;
#7005 = CARTESIAN_POINT ( 'NONE',  ( -21.33159362617910659, -4.962723823544877177, 53.49999999999995026 ) ) ;
#7006 = VERTEX_POINT ( 'NONE', #3528 ) ;
#7007 =( BOUNDED_CURVE ( )  B_SPLINE_CURVE ( 3, ( #19819, #27194, #1091, #5038 ),
 .UNSPECIFIED., .F., .F. ) 
 B_SPLINE_CURVE_WITH_KNOTS ( ( 4, 4 ),
 ( 0.4074455897393602921, 0.5000000000000000000 ),
 .UNSPECIFIED. ) 
 CURVE ( )  GEOMETRIC_REPRESENTATION_ITEM ( )  RATIONAL_B_SPLINE_CURVE ( ( 0.6983129098260847378, 0.7760317562606872110, 0.8765941196519910772, 0.9999999999999936717 ) ) 
 REPRESENTATION_ITEM ( '' )  );
#7008 = LINE ( 'NONE', #14118, #2676 ) ;
#7009 = AXIS2_PLACEMENT_3D ( 'NONE', #12401, #47830, #28407 ) ;
#7010 = AXIS2_PLACEMENT_3D ( 'NONE', #25113, #43838, #180 ) ;
#7011 = EDGE_CURVE ( 'NONE', #22569, #35836, #11691, .T. ) ;
#7012 = EDGE_LOOP ( 'NONE', ( #28332, #45638, #21521, #274, #1766 ) ) ;
#7013 = ORIENTED_EDGE ( 'NONE', *, *, #39849, .T. ) ;
#7014 = ORIENTED_EDGE ( 'NONE', *, *, #30757, .F. ) ;
#7015 = CARTESIAN_POINT ( 'NONE',  ( -13.86159385650551812, -9.295667164867525756, 49.30633214617472504 ) ) ;
#7016 = EDGE_CURVE ( 'NONE', #43308, #43598, #11899, .T. ) ;
#7017 = EDGE_CURVE ( 'NONE', #1136, #8232, #42427, .T. ) ;
#7018 = CARTESIAN_POINT ( 'NONE',  ( -23.75972628784533569, -10.79550978475970346, 53.49999999999994316 ) ) ;
#7019 = DIRECTION ( 'NONE',  ( -0.3478314405900310158, -0.9375570856950865561, 0.000000000000000000 ) ) ;
#7020 = CARTESIAN_POINT ( 'NONE',  ( -21.97361464010840493, -9.423584070311036953, 60.02171205573912260 ) ) ;
#7021 = B_SPLINE_CURVE_WITH_KNOTS ( 'NONE', 3,
 ( #13511, #33189, #44311, #48222, #25342, #9614, #28557, #18174, #28788, #2913 ),
 .UNSPECIFIED., .F., .F.,
 ( 4, 2, 2, 2, 4 ),
 ( 0.000000000000000000, 0.2500000000000000000, 0.5000000000000000000, 0.7500000000000000000, 1.000000000000000000 ),
 .UNSPECIFIED. ) ;
#7022 = CARTESIAN_POINT ( 'NONE',  ( -12.17409406592225629, -14.80771982110106677, 50.77966884056655772 ) ) ;
#7023 =( BOUNDED_CURVE ( )  B_SPLINE_CURVE ( 3, ( #33708, #11, #8367, #19199 ),
 .UNSPECIFIED., .F., .F. ) 
 B_SPLINE_CURVE_WITH_KNOTS ( ( 4, 4 ),
 ( 0.5000000000000000000, 0.9074455897393643999 ),
 .UNSPECIFIED. ) 
 CURVE ( )  GEOMETRIC_REPRESENTATION_ITEM ( )  RATIONAL_B_SPLINE_CURVE ( ( 1.000000000000001998, 0.4567392136813338555, 0.3561768502900293787, 0.6983129098260909551 ) ) 
 REPRESENTATION_ITEM ( '' )  );
#7024 = VERTEX_POINT ( 'NONE', #26431 ) ;
#7025 = ORIENTED_EDGE ( 'NONE', *, *, #41170, .T. ) ;
#7026 = CARTESIAN_POINT ( 'NONE',  ( -16.08659385650551599, -9.302874398569244363, 51.68646062012417985 ) ) ;
#7027 = CARTESIAN_POINT ( 'NONE',  ( -11.43418267526448417, -10.37927948953321966, 74.63159157388955123 ) ) ;
#7028 = FACE_OUTER_BOUND ( 'NONE', #753, .T. ) ;
#7030 = EDGE_CURVE ( 'NONE', #38940, #23317, #44924, .T. ) ;
#7029 = CARTESIAN_POINT ( 'NONE',  ( -19.96784385650551741, -6.428312510596451368, 51.20221977374900035 ) ) ;
#7031 = ADVANCED_FACE ( 'NONE', ( #18292 ), #15905, .T. ) ;
#7032 = ORIENTED_EDGE ( 'NONE', *, *, #47835, .F. ) ;
#7033 = EDGE_CURVE ( 'NONE', #36030, #47790, #14210, .T. ) ;
#7034 = EDGE_CURVE ( 'NONE', #31755, #32446, #33299, .T. ) ;
#7035 = CARTESIAN_POINT ( 'NONE',  ( -24.37622078247382618, -15.62647719184611184, 69.72410579710512479 ) ) ;
#7036 = AXIS2_PLACEMENT_3D ( 'NONE', #2397, #13698, #21601 ) ;
#7037 = CARTESIAN_POINT ( 'NONE',  ( -18.76269919900832761, -7.938388845612718292, 67.09174861995765582 ) ) ;
#7038 = CARTESIAN_POINT ( 'NONE',  ( -21.31115985637654120, -8.927249709250720144, 73.88656608925673197 ) ) ;
#7039 = VERTEX_POINT ( 'NONE', #27163 ) ;
#7040 = LINE ( 'NONE', #32175, #32760 ) ;
#7041 = VECTOR ( 'NONE', #32205, 1000.000000000000000 ) ;
#7042 = VECTOR ( 'NONE', #44218, 1000.000000000000000 ) ;
#7043 = VERTEX_POINT ( 'NONE', #27645 ) ;
#7044 = CARTESIAN_POINT ( 'NONE',  ( -44.67409385541304800, -15.81020654474410847, 70.50000000000000000 ) ) ;
#7045 = CARTESIAN_POINT ( 'NONE',  ( -10.12771871015461755, -16.31437777856581661, 71.64739150203183726 ) ) ;
#7046 = CARTESIAN_POINT ( 'NONE',  ( -24.42338698107307948, -14.97596128575578511, 59.31470420106809627 ) ) ;
#7047 = CARTESIAN_POINT ( 'NONE',  ( -12.15399301493812878, -9.543295845094297292, 57.20440096431307353 ) ) ;
#7048 = ORIENTED_EDGE ( 'NONE', *, *, #32245, .T. ) ;
#7049 = CARTESIAN_POINT ( 'NONE',  ( -22.44284385759798894, -7.587656875400192291, 49.25157356644813689 ) ) ;
#7050 = AXIS2_PLACEMENT_3D ( 'NONE', #35810, #21543, #14110 ) ;
#7051 = CARTESIAN_POINT ( 'NONE',  ( -24.42568804794990811, -14.79584343669470847, 62.82369473970615559 ) ) ;
#7052 = DIRECTION ( 'NONE',  ( -0.1922068328301543838, -0.9813544382196449645, 7.804899501296265607E-08 ) ) ;
#7053 = DIRECTION ( 'NONE',  ( -2.191687988502693051E-06, 1.258878959409210278E-05, 0.9999999999183594168 ) ) ;
#7054 = ORIENTED_EDGE ( 'NONE', *, *, #36469, .T. ) ;
#7055 = LINE ( 'NONE', #22068, #44870 ) ;
#7056 = CARTESIAN_POINT ( 'NONE',  ( -14.66630222544869078, -8.320656262913125545, 63.80450889863892172 ) ) ;
#7057 = CARTESIAN_POINT ( 'NONE',  ( -18.69688219364054049, -7.467975623574482746, 70.48412626434020467 ) ) ;
#7058 = ORIENTED_EDGE ( 'NONE', *, *, #23944, .F. ) ;
#7059 = FACE_BOUND ( 'NONE', #45629, .T. ) ;
#7060 = EDGE_LOOP ( 'NONE', ( #48713, #11075 ) ) ;
#7061 = DIRECTION ( 'NONE',  ( 0.05202058437830280740, -0.9986460127597464043, 1.657953767687799580E-08 ) ) ;
#7063 = EDGE_CURVE ( 'NONE', #8174, #26823, #20667, .T. ) ;
#7062 = CARTESIAN_POINT ( 'NONE',  ( -13.64037081340465818, -20.69854240475087437, 61.53148696990430011 ) ) ;
#7064 = VECTOR ( 'NONE', #41091, 1000.000000000000227 ) ;
#7065 = CARTESIAN_POINT ( 'NONE',  ( -24.42218830512229388, -14.64588455312011739, 63.01296487252135137 ) ) ;
#7066 =( REPRESENTATION_RELATIONSHIP ('NONE','NONE', #2768, #5940 ) REPRESENTATION_RELATIONSHIP_WITH_TRANSFORMATION ( #43224 )SHAPE_REPRESENTATION_RELATIONSHIP( ) );
#7067 = CARTESIAN_POINT ( 'NONE',  ( -21.41863048803933012, -8.999699081277377388, 73.61600897546567523 ) ) ;
#7068 = VERTEX_POINT ( 'NONE', #11652 ) ;
#7069 = ORIENTED_EDGE ( 'NONE', *, *, #45635, .F. ) ;
#7070 = LINE ( 'NONE', #37315, #32885 ) ;
#7071 = CARTESIAN_POINT ( 'NONE',  ( -15.48628188820593543, -7.614865071177022493, 74.26641013817956605 ) ) ;
#7072 = ORIENTED_EDGE ( 'NONE', *, *, #25606, .T. ) ;
#7073 = CARTESIAN_POINT ( 'NONE',  ( -10.16572694778485442, -13.12977483508055165, 71.38545448699323970 ) ) ;
#7074 = DIRECTION ( 'NONE',  ( 5.935091885992485906E-07, 2.117535305676834604E-07, -0.9999999999998013811 ) ) ;
#7075 = EDGE_CURVE ( 'NONE', #38907, #36780, #16587, .T. ) ;
#7076 = ORIENTED_EDGE ( 'NONE', *, *, #23328, .T. ) ;
#7077 = ORIENTED_EDGE ( 'NONE', *, *, #17029, .F. ) ;
#7078 = CARTESIAN_POINT ( 'NONE',  ( -13.99679447977218061, -20.97040113148658591, 71.94079819673058296 ) ) ;
#7080 = FACE_OUTER_BOUND ( 'NONE', #12844, .T. ) ;
#7079 = AXIS2_PLACEMENT_3D ( 'NONE', #988, #27804, #1714 ) ;
#7081 = CARTESIAN_POINT ( 'NONE',  ( -23.47573984560501259, -19.15461428502270280, 62.49260334658298177 ) ) ;
#7082 = CARTESIAN_POINT ( 'NONE',  ( -10.03581529055505506, -13.85215573028183655, 57.64836240523872846 ) ) ;
#7083 = CARTESIAN_POINT ( 'NONE',  ( -21.23815497595111879, -21.20890771667191999, 65.69115622141528377 ) ) ;
#7084 = CARTESIAN_POINT ( 'NONE',  ( -50.42609385541305755, -14.90920654474426499, 72.08823529411763786 ) ) ;
#7085 = CARTESIAN_POINT ( 'NONE',  ( -20.57133303063786300, -8.056536552513840377, 67.03749994897439990 ) ) ;
#7086 = CIRCLE ( 'NONE', #5513, 1.050000000000002265 ) ;
#7087 = ORIENTED_EDGE ( 'NONE', *, *, #40842, .T. ) ;
#7088 = ORIENTED_EDGE ( 'NONE', *, *, #25562, .F. ) ;
#7089 = CARTESIAN_POINT ( 'NONE',  ( -24.84033948030421968, -15.52542097194404569, 73.11648385888869939 ) ) ;
#7090 = CARTESIAN_POINT ( 'NONE',  ( -19.70639647806698136, -21.90109437720271757, 65.57990800639531415 ) ) ;
#7091 = CARTESIAN_POINT ( 'NONE',  ( -14.60689786731817286, -8.346551761976032324, 63.93978840692965093 ) ) ;
#7092 = AXIS2_PLACEMENT_3D ( 'NONE', #33179, #36393, #20913 ) ;
#7093 = DIRECTION ( 'NONE',  ( -0.5097212845717553620, 0.8603395911234816840, 0.000000000000000000 ) ) ;
#7094 = CARTESIAN_POINT ( 'NONE',  ( -7.424093855413048892, -25.10920654474410441, 63.99999999999998579 ) ) ;
#7095 = ORIENTED_EDGE ( 'NONE', *, *, #20587, .F. ) ;
#7096 = CARTESIAN_POINT ( 'NONE',  ( -20.89284385650552167, -7.406986770994973490, 48.81910596585309747 ) ) ;
#7097 = B_SPLINE_CURVE_WITH_KNOTS ( 'NONE', 3,
 ( #36362, #34071, #7269, #7510, #22515, #25060, #48607, #33320, #23023, #15591 ),
 .UNSPECIFIED., .F., .F.,
 ( 4, 2, 2, 2, 4 ),
 ( 0.000000000000000000, 0.2500000000000000000, 0.5000000000000000000, 0.7500000000000000000, 1.000000000000000000 ),
 .UNSPECIFIED. ) ;
#7098 = ORIENTED_EDGE ( 'NONE', *, *, #16877, .T. ) ;
#7099 = EDGE_CURVE ( 'NONE', #19673, #3400, #41079, .T. ) ;
#7100 = ADVANCED_FACE ( 'NONE', ( #35020 ), #339, .F. ) ;
#7101 = CARTESIAN_POINT ( 'NONE',  ( -20.03282965983824226, -21.84088468745754597, 56.49999999999994316 ) ) ;
#7102 = DIRECTION ( 'NONE',  ( -3.071710424422018668E-17, 6.404604876783312462E-16, 1.000000000000000000 ) ) ;
#7103 = LINE ( 'NONE', #11032, #4796 ) ;
#7104 = ORIENTED_EDGE ( 'NONE', *, *, #24891, .F. ) ;
#7105 = EDGE_CURVE ( 'NONE', #24743, #39816, #4837, .T. ) ;
#7106 = EDGE_CURVE ( 'NONE', #42696, #22914, #23960, .T. ) ;
#7107 = CARTESIAN_POINT ( 'NONE',  ( -18.87585836598739064, -7.910150609727056192, 67.19511962462686938 ) ) ;
#7108 = DIRECTION ( 'NONE',  ( 3.413470714839332458E-33, -1.190614954331866791E-16, 1.000000000000000000 ) ) ;
#7109 = VECTOR ( 'NONE', #48034, 1000.000000000000000 ) ;
#7110 = ORIENTED_EDGE ( 'NONE', *, *, #46959, .T. ) ;
#7111 = CARTESIAN_POINT ( 'NONE',  ( -15.18457398882241449, -21.44135615956592744, 65.39131358081642986 ) ) ;
#7112 = AXIS2_PLACEMENT_3D ( 'NONE', #31268, #12555, #12310 ) ;
#7113 = DIRECTION ( 'NONE',  ( -3.071710424422018668E-17, 6.404604876783312462E-16, 1.000000000000000000 ) ) ;
#7114 = ORIENTED_EDGE ( 'NONE', *, *, #40980, .F. ) ;
#7115 = B_SPLINE_CURVE_WITH_KNOTS ( 'NONE', 1,
 ( #5488, #1533 ),
 .UNSPECIFIED., .F., .F.,
 ( 2, 2 ),
 ( 0.000000000000000000, 1.000000000000000000 ),
 .UNSPECIFIED. ) ;
#7116 = DIRECTION ( 'NONE',  ( 0.9942595023566569434, -0.1069955231469581769, 3.800058679842193584E-08 ) ) ;
#7117 = CIRCLE ( 'NONE', #44882, 6.899999999999999467 ) ;
#7118 = ORIENTED_EDGE ( 'NONE', *, *, #46416, .T. ) ;
#7119 = CYLINDRICAL_SURFACE ( 'NONE', #17133, 1.999999999999999556 ) ;
#7120 = DIRECTION ( 'NONE',  ( -3.159776991290051445E-16, -1.000000000000000000, -6.457808579236824910E-31 ) ) ;
#7121 = EDGE_LOOP ( 'NONE', ( #48578, #25530 ) ) ;
#7122 = CARTESIAN_POINT ( 'NONE',  ( -12.95890174405234241, -8.844667670358365541, 67.56598159878524257 ) ) ;
#7123 = EDGE_CURVE ( 'NONE', #10658, #27516, #23694, .T. ) ;
#7124 = CARTESIAN_POINT ( 'NONE',  ( -18.62040859620581301, -22.16269830898913540, 72.44544270657438290 ) ) ;
#7125 = VERTEX_POINT ( 'NONE', #45885 ) ;
#7126 = DIRECTION ( 'NONE',  ( -0.5263399769092093061, 0.8502742079512978224, 7.678741024442198749E-08 ) ) ;
#7127 = AXIS2_PLACEMENT_3D ( 'NONE', #42213, #11433, #45431 ) ;
#7128 = LINE ( 'NONE', #32720, #5528 ) ;
#7129 = CARTESIAN_POINT ( 'NONE',  ( -24.86571005758334252, -14.45474999747601252, 66.29018563260261487 ) ) ;
#7130 = ORIENTED_EDGE ( 'NONE', *, *, #31131, .T. ) ;
#7131 = FACE_OUTER_BOUND ( 'NONE', #17963, .T. ) ;
#7132 = CARTESIAN_POINT ( 'NONE',  ( -33.52409385541305653, -25.10920654474410441, 52.29999999999998295 ) ) ;
#7133 = FACE_OUTER_BOUND ( 'NONE', #32474, .T. ) ;
#7134 = VERTEX_POINT ( 'NONE', #46118 ) ;
#7135 = ORIENTED_EDGE ( 'NONE', *, *, #14447, .T. ) ;
#7136 = CARTESIAN_POINT ( 'NONE',  ( -22.76532612177806314, -10.19550891705927498, 73.62593845350987465 ) ) ;
#7137 = CARTESIAN_POINT ( 'NONE',  ( -16.87238795883161657, -7.830921832911093894, 74.03306333698706965 ) ) ;
#7138 = FACE_OUTER_BOUND ( 'NONE', #7905, .T. ) ;
#7139 = CARTESIAN_POINT ( 'NONE',  ( -14.68034385759798965, -9.360768649639302552, 51.01397948905922419 ) ) ;
#7140 = CARTESIAN_POINT ( 'NONE',  ( -24.08977912471840810, -11.48169904069885661, 62.99572364416607684 ) ) ;
#7141 = CARTESIAN_POINT ( 'NONE',  ( -13.06813783877040969, -9.265530354883374287, 67.66470656304637998 ) ) ;
#7142 = CARTESIAN_POINT ( 'NONE',  ( -14.45534385759799179, -8.623186033802571870, 49.24843789510467218 ) ) ;
#7143 = CARTESIAN_POINT ( 'NONE',  ( -16.56797618387698279, -22.20990603440958111, 65.41838526417717503 ) ) ;
#7144 = VERTEX_POINT ( 'NONE', #11908 ) ;
#7145 = CYLINDRICAL_SURFACE ( 'NONE', #48547, 0.1500000000000039913 ) ;
#7146 = CARTESIAN_POINT ( 'NONE',  ( -14.43441977789444763, -8.421195553735145722, 71.14446303425738449 ) ) ;
#7147 = AXIS2_PLACEMENT_3D ( 'NONE', #47276, #17930, #29030 ) ;
#7148 = DIRECTION ( 'NONE',  ( -3.071710424422018668E-17, 6.404604876783312462E-16, 1.000000000000000000 ) ) ;
#7149 = DIRECTION ( 'NONE',  ( 3.071710424422018668E-17, -6.404604876783312462E-16, -1.000000000000000000 ) ) ;
#7150 =( BOUNDED_CURVE ( )  B_SPLINE_CURVE ( 3, ( #43493, #27728, #21069, #39538 ),
 .UNSPECIFIED., .F., .F. ) 
 B_SPLINE_CURVE_WITH_KNOTS ( ( 4, 4 ),
 ( 4.712388980384689674, 4.921828490624009511 ),
 .UNSPECIFIED. ) 
 CURVE ( )  GEOMETRIC_REPRESENTATION_ITEM ( )  RATIONAL_B_SPLINE_CURVE ( ( 1.000000000000000000, 0.9963479302455154896, 0.9963479302455154896, 1.000000000000000000 ) ) 
 REPRESENTATION_ITEM ( '' )  );
#7151 = AXIS2_PLACEMENT_3D ( 'NONE', #40231, #28177, #39500 ) ;
#7152 = ORIENTED_EDGE ( 'NONE', *, *, #37434, .T. ) ;
#7153 = ORIENTED_EDGE ( 'NONE', *, *, #44651, .T. ) ;
#7154 = ADVANCED_FACE ( 'NONE', ( #15821 ), #7773, .T. ) ;
#7155 = CARTESIAN_POINT ( 'NONE',  ( -36.42409385541304800, -8.109206544743658540, 50.50000000000030553 ) ) ;
#7156 = CARTESIAN_POINT ( 'NONE',  ( -23.00441852451001523, -19.11762575345012749, 58.88410642058936872 ) ) ;
#7157 = LINE ( 'NONE', #11823, #29190 ) ;
#7158 = PLANE ( 'NONE',  #15420 ) ;
#7159 = B_SPLINE_CURVE_WITH_KNOTS ( 'NONE', 3,
 ( #34126, #7329, #3365, #25775, #11486, #22572, #14650, #22326, #40791, #18371 ),
 .UNSPECIFIED., .F., .F.,
 ( 4, 2, 2, 2, 4 ),
 ( 0.000000000000000000, 0.2500000000000000000, 0.5000000000000000000, 0.7500000000000000000, 1.000000000000000000 ),
 .UNSPECIFIED. ) ;
#7160 = ORIENTED_EDGE ( 'NONE', *, *, #28024, .F. ) ;
#7161 =( BOUNDED_CURVE ( )  B_SPLINE_CURVE ( 3, ( #14014, #17721, #32520, #47062 ),
 .UNSPECIFIED., .F., .F. ) 
 B_SPLINE_CURVE_WITH_KNOTS ( ( 4, 4 ),
 ( 0.5000000000000000000, 0.9074455897393561843 ),
 .UNSPECIFIED. ) 
 CURVE ( )  GEOMETRIC_REPRESENTATION_ITEM ( )  RATIONAL_B_SPLINE_CURVE ( ( 1.000000000000013545, 0.4567392136813450132, 0.3561768502900254374, 0.6983129098260696388 ) ) 
 REPRESENTATION_ITEM ( '' )  );
#7162 = CARTESIAN_POINT ( 'NONE',  ( -23.61204096558246235, -11.53669824655086451, 66.72214514747398084 ) ) ;
#7163 = EDGE_CURVE ( 'NONE', #11354, #38153, #27399, .T. ) ;
#7164 = EDGE_CURVE ( 'NONE', #37281, #44219, #1285, .T. ) ;
#7165 = LINE ( 'NONE', #13552, #29643 ) ;
#7166 = CIRCLE ( 'NONE', #13433, 1.949999999999999956 ) ;
#7167 = VERTEX_POINT ( 'NONE', #43889 ) ;
#7168 = ADVANCED_FACE ( 'NONE', ( #36226 ), #2020, .F. ) ;
#7169 = CARTESIAN_POINT ( 'NONE',  ( -35.42409385541304800, -6.859212275519750435, 50.50378509014258555 ) ) ;
#7170 = CARTESIAN_POINT ( 'NONE',  ( -13.27409385759798965, -6.859212275519751323, 50.50378509014259265 ) ) ;
#7171 = EDGE_CURVE ( 'NONE', #30917, #41834, #39205, .T. ) ;
#7172 = CARTESIAN_POINT ( 'NONE',  ( -22.96481576609224717, -19.16891988936071556, 58.89882756593014790 ) ) ;
#7173 = VERTEX_POINT ( 'NONE', #1786 ) ;
#7174 = CARTESIAN_POINT ( 'NONE',  ( -20.15112924866626187, -10.01741632518351643, 53.69233794759168887 ) ) ;
#7175 = ORIENTED_EDGE ( 'NONE', *, *, #32228, .T. ) ;
#7176 = CARTESIAN_POINT ( 'NONE',  ( -19.44142144650348314, -21.98165757830647138, 62.18158996068683564 ) ) ;
#7177 = B_SPLINE_CURVE_WITH_KNOTS ( 'NONE', 3,
 ( #20683, #40299, #42617, #1464, #31759, #9116, #46299, #5177, #47928, #46779 ),
 .UNSPECIFIED., .F., .F.,
 ( 4, 2, 2, 2, 4 ),
 ( 0.000000000000000000, 0.2500000000000000000, 0.5000000000000000000, 0.7500000000000000000, 1.000000000000000000 ),
 .UNSPECIFIED. ) ;
#7178 = DIRECTION ( 'NONE',  ( -1.669677910507523057E-21, 1.000000000000000000, 0.000000000000000000 ) ) ;
#7179 = ORIENTED_EDGE ( 'NONE', *, *, #14546, .T. ) ;
#7180 = CARTESIAN_POINT ( 'NONE',  ( -24.15358334166845111, -18.00564352615971941, 59.19716716663268130 ) ) ;
#7181 = CARTESIAN_POINT ( 'NONE',  ( -10.39215589072981416, -14.30487699944780289, 64.68803863382906627 ) ) ;
#7182 = EDGE_CURVE ( 'NONE', #9242, #18330, #35738, .T. ) ;
#7183 = CARTESIAN_POINT ( 'NONE',  ( -20.69909385650551670, -8.114302828567740988, 52.18300498402516041 ) ) ;
#7184 = CIRCLE ( 'NONE', #34695, 1.999999999999999112 ) ;
#7185 = CARTESIAN_POINT ( 'NONE',  ( -14.42683419600289341, -8.428067575814653267, 67.55975083869262221 ) ) ;
#7186 = CARTESIAN_POINT ( 'NONE',  ( -14.33942418930512019, -10.56099362034968614, 50.77966884056655772 ) ) ;
#7187 = FACE_OUTER_BOUND ( 'NONE', #24691, .T. ) ;
#7188 = CARTESIAN_POINT ( 'NONE',  ( -50.42609385541305755, -14.80920654474427600, 73.99411764705880046 ) ) ;
#7189 = EDGE_LOOP ( 'NONE', ( #39531, #15160, #45984, #2593 ) ) ;
#7190 = LINE ( 'NONE', #44145, #23128 ) ;
#7191 = CARTESIAN_POINT ( 'NONE',  ( -9.990737576226866423, -14.31032742905966337, 64.43157936802064967 ) ) ;
#7192 = CARTESIAN_POINT ( 'NONE',  ( -14.45653002406802834, -7.975746824180188099, 63.98990036560820016 ) ) ;
#7193 = CARTESIAN_POINT ( 'NONE',  ( -12.55411140858086760, -19.90724249994213935, 65.15202838036978505 ) ) ;
#7194 = B_SPLINE_CURVE_WITH_KNOTS ( 'NONE', 1,
 ( #18867, #44494 ),
 .UNSPECIFIED., .F., .F.,
 ( 2, 2 ),
 ( 0.000000000000000000, 1.000000000000000000 ),
 .UNSPECIFIED. ) ;
#7195 = CARTESIAN_POINT ( 'NONE',  ( -18.71757194967216975, -7.929750632967406787, 70.37068030597254165 ) ) ;
#7196 = CARTESIAN_POINT ( 'NONE',  ( -23.81024829756716343, -18.64597716098235836, 72.94863620959463901 ) ) ;
#7197 = ORIENTED_EDGE ( 'NONE', *, *, #36790, .T. ) ;
#7198 = ORIENTED_EDGE ( 'NONE', *, *, #21519, .F. ) ;
#7199 = DIRECTION ( 'NONE',  ( -2.168404344971008375E-16, 0.000000000000000000, 1.000000000000000000 ) ) ;
#7200 = CARTESIAN_POINT ( 'NONE',  ( -14.86277779823650391, -8.294567775944363675, 57.07673407009221478 ) ) ;
#7201 = EDGE_LOOP ( 'NONE', ( #43513, #21073, #36835, #15298 ) ) ;
#7203 = CARTESIAN_POINT ( 'NONE',  ( -13.17364361214796098, -9.395187332399693503, 49.41428126932424192 ) ) ;
#7202 = CARTESIAN_POINT ( 'NONE',  ( -14.68550372792196335, -21.30572237930008939, 58.17177643121559782 ) ) ;
#7204 = CARTESIAN_POINT ( 'NONE',  ( -17.42409385541306222, -14.80920654474411080, 82.49999999999998579 ) ) ;
#7205 = CARTESIAN_POINT ( 'NONE',  ( -20.68222199850074361, -8.109235517929556991, 63.47154877063784539 ) ) ;
#7206 = CARTESIAN_POINT ( 'NONE',  ( -22.33142775017075010, -9.202805011845722305, 59.90826508960974195 ) ) ;
#7207 = CARTESIAN_POINT ( 'NONE',  ( -11.29219319990544079, -18.28864530752396433, 57.82186711835544912 ) ) ;
#7208 = CARTESIAN_POINT ( 'NONE',  ( -11.07238894598444112, -11.74315414212633080, 67.50375847841529264 ) ) ;
#7209 = CARTESIAN_POINT ( 'NONE',  ( -11.45241200840138340, -19.26367093908298500, 71.79347555607934339 ) ) ;
#7210 = CARTESIAN_POINT ( 'NONE',  ( -16.78865379391102408, -21.78030513117466072, 68.69560651887046276 ) ) ;
#7211 = VERTEX_POINT ( 'NONE', #43406 ) ;
#7212 = CARTESIAN_POINT ( 'NONE',  ( -24.09981952095640167, -11.50204489274636366, 63.15207061483707207 ) ) ;
#7213 = CARTESIAN_POINT ( 'NONE',  ( -21.50517322895428052, -9.056100137350421519, 66.86969788852485408 ) ) ;
#7214 = CARTESIAN_POINT ( 'NONE',  ( -24.70336335543259665, -13.22337356223611060, 59.56256691634375500 ) ) ;
#7215 = CARTESIAN_POINT ( 'NONE',  ( -17.42409385541299471, -14.80920654474435771, 49.52966884056655772 ) ) ;
#7216 = CARTESIAN_POINT ( 'NONE',  ( -24.59748878097435210, -12.79772186451832994, 66.34600794915635902 ) ) ;
#7217 = EDGE_CURVE ( 'NONE', #21955, #5832, #32591, .T. ) ;
#7218 = CARTESIAN_POINT ( 'NONE',  ( -11.83525287003876336, -10.59418596192610096, 74.73885130397258081 ) ) ;
#7219 = DIRECTION ( 'NONE',  ( 0.000000000000000000, 0.000000000000000000, -1.000000000000000000 ) ) ;
#7220 = VERTEX_POINT ( 'NONE', #24689 ) ;
#7221 = ORIENTED_EDGE ( 'NONE', *, *, #22516, .F. ) ;
#7222 = CARTESIAN_POINT ( 'NONE',  ( -13.42364594203567307, -9.064338107776409359, 49.69363550592916567 ) ) ;
#7223 = B_SPLINE_CURVE_WITH_KNOTS ( 'NONE', 1,
 ( #4196, #22917 ),
 .UNSPECIFIED., .F., .F.,
 ( 2, 2 ),
 ( 0.000000000000000000, 1.000000000000000000 ),
 .UNSPECIFIED. ) ;
#7224 = AXIS2_PLACEMENT_3D ( 'NONE', #12951, #13432, #13904 ) ;
#7225 = EDGE_LOOP ( 'NONE', ( #44234, #33031, #9235, #41281 ) ) ;
#7226 = EDGE_CURVE ( 'NONE', #22495, #21028, #9903, .T. ) ;
#7227 = CARTESIAN_POINT ( 'NONE',  ( -22.23733836534369601, -19.96043719841513564, 65.85421731380807842 ) ) ;
#7228 = CARTESIAN_POINT ( 'NONE',  ( -24.01119280393830024, -17.17795836609833415, 69.69874480771339620 ) ) ;
#7229 = CARTESIAN_POINT ( 'NONE',  ( -24.61791017297192852, -12.87185432802827734, 66.48059519668728967 ) ) ;
#7230 = CARTESIAN_POINT ( 'NONE',  ( -17.42409385541299471, -14.80920654474435594, 52.02966884056656482 ) ) ;
#7231 = ORIENTED_EDGE ( 'NONE', *, *, #25336, .T. ) ;
#7232 = EDGE_CURVE ( 'NONE', #27202, #37668, #35737, .T. ) ;
#7233 = CARTESIAN_POINT ( 'NONE',  ( -24.37280409347697230, -15.65865158627326537, 73.28687223815994400 ) ) ;
#7234 = CIRCLE ( 'NONE', #34744, 5.249999999999998224 ) ;
#7235 = LINE ( 'NONE', #15307, #27321 ) ;
#7236 = EDGE_CURVE ( 'NONE', #12395, #32426, #42388, .T. ) ;
#7237 = ORIENTED_EDGE ( 'NONE', *, *, #48000, .F. ) ;
#7238 = CARTESIAN_POINT ( 'NONE',  ( -19.12409385759799108, -9.359200813967568422, 50.49621490985803263 ) ) ;
#7239 = DIRECTION ( 'NONE',  ( 4.115385489419834812E-17, 0.9999954153791273948, 0.003028072113822188795 ) ) ;
#7240 = EDGE_LOOP ( 'NONE', ( #6843, #27671 ) ) ;
#7241 = EDGE_CURVE ( 'NONE', #29883, #30739, #25983, .T. ) ;
#7242 = CARTESIAN_POINT ( 'NONE',  ( -19.50997552649656086, -21.96132259753523996, 62.25149580216906742 ) ) ;
#7243 = CARTESIAN_POINT ( 'NONE',  ( -21.12516169987187098, -20.80993955427394582, 69.06922321213187388 ) ) ;
#7244 = CARTESIAN_POINT ( 'NONE',  ( -13.11946129443726861, -9.225960368241006293, 67.37942785707224402 ) ) ;
#7245 = VERTEX_POINT ( 'NONE', #16785 ) ;
#7246 = CARTESIAN_POINT ( 'NONE',  ( -11.16823349194678627, -11.55205338407005122, 71.50349565124497531 ) ) ;
#7247 = CARTESIAN_POINT ( 'NONE',  ( -11.64235026963700470, -18.84330375823651949, 68.21689631561287115 ) ) ;
#7248 = EDGE_CURVE ( 'NONE', #39514, #4743, #43978, .T. ) ;
#7249 = CYLINDRICAL_SURFACE ( 'NONE', #38426, 1.999999999999999112 ) ;
#7250 = CARTESIAN_POINT ( 'NONE',  ( -46.29409385541305966, -12.70920654474410760, 71.79999999999999716 ) ) ;
#7251 = ORIENTED_EDGE ( 'NONE', *, *, #35624, .T. ) ;
#7252 = CARTESIAN_POINT ( 'NONE',  ( -11.13352401182878459, -11.60862911821036292, 74.70272630447266238 ) ) ;
#7253 = LINE ( 'NONE', #22497, #34471 ) ;
#7254 = CYLINDRICAL_SURFACE ( 'NONE', #30195, 0.1500000000000040190 ) ;
#7255 = DIRECTION ( 'NONE',  ( -0.6043825497304157190, 0.7966942535134532433, -5.656674838623230539E-08 ) ) ;
#7256 = CARTESIAN_POINT ( 'NONE',  ( -19.65534385650552451, -7.417179338643134834, 52.18511593390279302 ) ) ;
#7257 = B_SPLINE_CURVE_WITH_KNOTS ( 'NONE', 3,
 ( #5722, #40171, #14028, #32531, #21690, #43137, #28109, #25149, #9890, #43393 ),
 .UNSPECIFIED., .F., .F.,
 ( 4, 2, 2, 2, 4 ),
 ( 0.6272669072979107918, 0.7522669073148898766, 0.8772669073318688504, 1.002266907348847935, 1.127266907365827020 ),
 .UNSPECIFIED. ) ;
#7258 = ORIENTED_EDGE ( 'NONE', *, *, #19448, .T. ) ;
#7259 = AXIS2_PLACEMENT_3D ( 'NONE', #34312, #18563, #45191 ) ;
#7260 = FACE_OUTER_BOUND ( 'NONE', #5682, .T. ) ;
#7261 = CARTESIAN_POINT ( 'NONE',  ( -18.31357764725860093, -21.80286926110680668, 68.96514702303620936 ) ) ;
#7262 = ORIENTED_EDGE ( 'NONE', *, *, #43370, .F. ) ;
#7263 = CARTESIAN_POINT ( 'NONE',  ( -22.34731130624134465, -19.85564328841742920, 69.17977748773124347 ) ) ;
#7264 = CARTESIAN_POINT ( 'NONE',  ( -21.37409385759799108, -6.859212275519751323, 50.50378509014259265 ) ) ;
#7265 = CARTESIAN_POINT ( 'NONE',  ( -11.69162037657732078, -10.05084142047440565, 67.69171023900449313 ) ) ;
#7266 = B_SPLINE_CURVE_WITH_KNOTS ( 'NONE', 3,
 ( #7195, #17523, #10150, #32783, #6693, #8168, #23180, #45346, #26375, #22950 ),
 .UNSPECIFIED., .F., .F.,
 ( 4, 2, 2, 2, 4 ),
 ( 0.000000000000000000, 0.2500000000000000000, 0.5000000000000000000, 0.7500000000000000000, 1.000000000000000000 ),
 .UNSPECIFIED. ) ;
#7267 = ORIENTED_EDGE ( 'NONE', *, *, #42489, .F. ) ;
#7268 = CARTESIAN_POINT ( 'NONE',  ( -17.91159385541293858, -8.990409506049328314, 49.61344411288062162 ) ) ;
#7269 = CARTESIAN_POINT ( 'NONE',  ( -10.68182963115602924, -12.92559189733731273, 67.75449013086223715 ) ) ;
#7270 = ORIENTED_EDGE ( 'NONE', *, *, #12278, .T. ) ;
#7271 = ORIENTED_EDGE ( 'NONE', *, *, #29716, .F. ) ;
#7272 = CARTESIAN_POINT ( 'NONE',  ( -14.76159385650551847, -9.295667164867525756, 49.30633214617472504 ) ) ;
#7273 = CARTESIAN_POINT ( 'NONE',  ( -13.60238606012557483, -8.884930320952351579, 56.96967755506135234 ) ) ;
#7274 = DIRECTION ( 'NONE',  ( 6.374839753205896285E-22, 0.007114381193220334181, -0.9999746924698833528 ) ) ;
#7275 = EDGE_CURVE ( 'NONE', #6219, #39482, #3690, .T. ) ;
#7276 = CARTESIAN_POINT ( 'NONE',  ( -24.84793640206982701, -14.18443463346696909, 69.83770693398628282 ) ) ;
#7277 = FACE_OUTER_BOUND ( 'NONE', #33472, .T. ) ;
#7278 = VERTEX_POINT ( 'NONE', #31584 ) ;
#7279 = VERTEX_POINT ( 'NONE', #20506 ) ;
#7280 = CARTESIAN_POINT ( 'NONE',  ( -14.28659385650551528, -9.302874398569244363, 51.68646062012417985 ) ) ;
#7281 = B_SPLINE_CURVE_WITH_KNOTS ( 'NONE', 1,
 ( #26922, #30380 ),
 .UNSPECIFIED., .F., .F.,
 ( 2, 2 ),
 ( 0.000000000000000000, 1.000000000000000000 ),
 .UNSPECIFIED. ) ;
#7282 = DIRECTION ( 'NONE',  ( -3.071710424422018668E-17, 6.404604876783312462E-16, 1.000000000000000000 ) ) ;
#7283 = CARTESIAN_POINT ( 'NONE',  ( -10.48067290732983281, -16.03043740265091444, 67.97767830707738312 ) ) ;
#7284 = CARTESIAN_POINT ( 'NONE',  ( -14.84909385650551705, -8.104110260919579645, 48.81699501597546487 ) ) ;
#7285 = VERTEX_POINT ( 'NONE', #12856 ) ;
#7286 = CARTESIAN_POINT ( 'NONE',  ( -17.42409385541299471, -14.80920654474435771, 49.52966884056655772 ) ) ;
#7287 = ADVANCED_FACE ( 'NONE', ( #6204 ), #7448, .T. ) ;
#7288 = CARTESIAN_POINT ( 'NONE',  ( -17.42409385541299471, -14.80920654474434883, 62.02966884056656482 ) ) ;
#7289 = B_SPLINE_CURVE_WITH_KNOTS ( 'NONE', 3,
 ( #26832, #41852, #8124, #11556, #4911, #33958, #12281, #251, #15719, #41603 ),
 .UNSPECIFIED., .F., .F.,
 ( 4, 2, 2, 2, 4 ),
 ( 0.6272669072877233853, 0.7522669073072442147, 0.8772669073267651552, 1.002266907346285985, 1.127266907365806814 ),
 .UNSPECIFIED. ) ;
#7290 = LINE ( 'NONE', #25738, #43820 ) ;
#7291 =( BOUNDED_CURVE ( )  B_SPLINE_CURVE ( 3, ( #32510, #44103, #10357, #33208 ),
 .UNSPECIFIED., .F., .F. ) 
 B_SPLINE_CURVE_WITH_KNOTS ( ( 4, 4 ),
 ( 0.9074455897393668424, 1.000000000000000000 ),
 .UNSPECIFIED. ) 
 CURVE ( )  GEOMETRIC_REPRESENTATION_ITEM ( )  RATIONAL_B_SPLINE_CURVE ( ( 0.6983129098261178225, 0.7760317562607195185, 0.8765941196520136147, 1.000000000000000000 ) ) 
 REPRESENTATION_ITEM ( '' )  );
#7292 = EDGE_LOOP ( 'NONE', ( #4606, #28442, #47581, #8493 ) ) ;
#7293 = CARTESIAN_POINT ( 'NONE',  ( -23.08261055559088248, -18.93003034027461950, 62.65406880913197796 ) ) ;
#7294 = EDGE_LOOP ( 'NONE', ( #19657, #13406, #48208, #16702, #35099 ) ) ;
#7295 = EDGE_CURVE ( 'NONE', #24855, #23931, #48334, .T. ) ;
#7296 = CARTESIAN_POINT ( 'NONE',  ( -13.01353397724842154, -8.804979801064929390, 64.09441804368185558 ) ) ;
#7297 = CARTESIAN_POINT ( 'NONE',  ( -24.82750195234013191, -13.97654432178796569, 73.30766915316792165 ) ) ;
#7298 = CARTESIAN_POINT ( 'NONE',  ( -24.72409385541305582, -14.80920654474428488, 74.09999999999998010 ) ) ;
#7299 = CARTESIAN_POINT ( 'NONE',  ( -9.992295536073678264, -14.28860446562057085, 64.48780235712654019 ) ) ;
#7300 = ORIENTED_EDGE ( 'NONE', *, *, #36737, .T. ) ;
#7301 = CARTESIAN_POINT ( 'NONE',  ( -11.29219319990544079, -18.28864530752396433, 57.82186711835544912 ) ) ;
#7302 = CYLINDRICAL_SURFACE ( 'NONE', #9299, 0.1500000000000050737 ) ;
#7303 = EDGE_CURVE ( 'NONE', #18791, #7630, #2304, .T. ) ;
#7304 = LINE ( 'NONE', #14631, #14778 ) ;
#7305 = CARTESIAN_POINT ( 'NONE',  ( -10.08870644134023387, -16.11102152315157099, 68.17756598889880593 ) ) ;
#7306 = VERTEX_POINT ( 'NONE', #41382 ) ;
#7307 = CARTESIAN_POINT ( 'NONE',  ( -10.55690563545519822, -17.69827471655239037, 68.23575463352698023 ) ) ;
#7308 = CARTESIAN_POINT ( 'NONE',  ( -18.53714847821261458, -22.17566945187693506, 72.54156883610106377 ) ) ;
#7309 =( BOUNDED_CURVE ( )  B_SPLINE_CURVE ( 3, ( #19014, #34018, #19490, #788 ),
 .UNSPECIFIED., .F., .F. ) 
 B_SPLINE_CURVE_WITH_KNOTS ( ( 4, 4 ),
 ( 0.000000000000000000, 0.4074455897393702286 ),
 .UNSPECIFIED. ) 
 CURVE ( )  GEOMETRIC_REPRESENTATION_ITEM ( )  RATIONAL_B_SPLINE_CURVE ( ( 1.000000000000000000, 0.4567392136813277492, 0.3561768502900287126, 0.6983129098261028345 ) ) 
 REPRESENTATION_ITEM ( '' )  );
#7310 = CARTESIAN_POINT ( 'NONE',  ( -10.83536388074712598, -17.31742051234312640, 64.92739380450886699 ) ) ;
#7311 = VERTEX_POINT ( 'NONE', #18476 ) ;
#7312 = FACE_BOUND ( 'NONE', #12358, .T. ) ;
#7313 = EDGE_LOOP ( 'NONE', ( #2415, #6034, #31456, #18092 ) ) ;
#7314 = CARTESIAN_POINT ( 'NONE',  ( -11.29385027892729987, -19.04286830487734861, 68.33194243210506613 ) ) ;
#7315 = CARTESIAN_POINT ( 'NONE',  ( -13.64007738217462062, -20.69835563907848552, 61.80180905510582789 ) ) ;
#7316 = CARTESIAN_POINT ( 'NONE',  ( -16.91478550490786859, -21.84108428878278119, 72.18015306840750611 ) ) ;
#7317 = CARTESIAN_POINT ( 'NONE',  ( -17.80887632446114921, -10.12652590253629903, 49.52966884056655772 ) ) ;
#7318 = ORIENTED_EDGE ( 'NONE', *, *, #37904, .T. ) ;
#7319 = CARTESIAN_POINT ( 'NONE',  ( -10.44762901317458414, -14.23035498823898415, 64.40420498733567456 ) ) ;
#7320 = ORIENTED_EDGE ( 'NONE', *, *, #2131, .F. ) ;
#7321 = CARTESIAN_POINT ( 'NONE',  ( -17.83653785972521177, -7.771132672202180736, 60.08620545617123554 ) ) ;
#7322 = CARTESIAN_POINT ( 'NONE',  ( -10.95349617038790591, -18.50195306419159991, 57.94681249741275764 ) ) ;
#7324 = EDGE_CURVE ( 'NONE', #2752, #31166, #8611, .T. ) ;
#7323 = CARTESIAN_POINT ( 'NONE',  ( -28.42409385541305511, -25.10920654474410441, 45.99999999999998579 ) ) ;
#7325 = ORIENTED_EDGE ( 'NONE', *, *, #17608, .T. ) ;
#7326 = FACE_OUTER_BOUND ( 'NONE', #44405, .T. ) ;
#7327 =( BOUNDED_CURVE ( )  B_SPLINE_CURVE ( 3, ( #3153, #22604, #41075, #7359 ),
 .UNSPECIFIED., .F., .F. ) 
 B_SPLINE_CURVE_WITH_KNOTS ( ( 4, 4 ),
 ( 0.000000000000000000, 0.4074455897393614023 ),
 .UNSPECIFIED. ) 
 CURVE ( )  GEOMETRIC_REPRESENTATION_ITEM ( )  RATIONAL_B_SPLINE_CURVE ( ( 1.000000000000000000, 0.4567392136813356318, 0.3561768502900316546, 0.6983129098260881795 ) ) 
 REPRESENTATION_ITEM ( '' )  );
#7328 = EDGE_CURVE ( 'NONE', #19164, #20160, #29828, .T. ) ;
#7329 = CARTESIAN_POINT ( 'NONE',  ( -13.44722279732532577, -20.56995410411473202, 58.04650027625321940 ) ) ;
#7330 = EDGE_CURVE ( 'NONE', #48127, #7024, #12460, .T. ) ;
#7331 = ORIENTED_EDGE ( 'NONE', *, *, #15055, .F. ) ;
#7332 = EDGE_LOOP ( 'NONE', ( #45098, #25248 ) ) ;
#7333 = CARTESIAN_POINT ( 'NONE',  ( -18.40115675053315059, -19.96748611248585448, 49.52966884056656482 ) ) ;
#7334 = CARTESIAN_POINT ( 'NONE',  ( -20.50783594841701785, -8.027295835816985914, 66.96599399791791996 ) ) ;
#7335 = CARTESIAN_POINT ( 'NONE',  ( -12.74836358285320159, -20.08597126951521261, 71.82125749157572159 ) ) ;
#7336 = CARTESIAN_POINT ( 'NONE',  ( -10.04001549485839995, -13.81937382109866341, 57.57108164808059314 ) ) ;
#7337 = B_SPLINE_CURVE_WITH_KNOTS ( 'NONE', 1,
 ( #47991, #10334 ),
 .UNSPECIFIED., .F., .F.,
 ( 2, 2 ),
 ( 0.000000000000000000, 1.000000000000000000 ),
 .UNSPECIFIED. ) ;
#7338 = LINE ( 'NONE', #45253, #21255 ) ;
#7339 = FACE_OUTER_BOUND ( 'NONE', #30283, .T. ) ;
#7340 = CARTESIAN_POINT ( 'NONE',  ( -22.47245519635065492, -19.73066437834766873, 72.65872596779033188 ) ) ;
#7341 = ORIENTED_EDGE ( 'NONE', *, *, #29731, .F. ) ;
#7342 = ORIENTED_EDGE ( 'NONE', *, *, #9764, .F. ) ;
#7343 = CARTESIAN_POINT ( 'NONE',  ( -22.54166034846558020, -20.22352459525847834, 65.82608991095307260 ) ) ;
#7344 = CARTESIAN_POINT ( 'NONE',  ( -11.12207588469793329, -10.83591208581314369, 57.35903209041984496 ) ) ;
#7345 = DIRECTION ( 'NONE',  ( 0.000000000000000000, 1.000000000000000000, -0.000000000000000000 ) ) ;
#7346 = VERTEX_POINT ( 'NONE', #41145 ) ;
#7347 = B_SPLINE_CURVE_WITH_KNOTS ( 'NONE', 3,
 ( #23298, #4112, #16792, #46852, #4340, #5499, #45467, #2028, #20514, #23064 ),
 .UNSPECIFIED., .F., .F.,
 ( 4, 2, 2, 2, 4 ),
 ( 0.6272669072877261609, 0.7522669073072449919, 0.8772669073267638229, 1.002266907346282654, 1.127266907365801485 ),
 .UNSPECIFIED. ) ;
#7348 = CARTESIAN_POINT ( 'NONE',  ( -17.06784385650551528, -6.428312510596451368, 51.20221977374900035 ) ) ;
#7349 = ORIENTED_EDGE ( 'NONE', *, *, #7033, .T. ) ;
#7350 = B_SPLINE_CURVE_WITH_KNOTS ( 'NONE', 1,
 ( #41979, #15855 ),
 .UNSPECIFIED., .F., .F.,
 ( 2, 2 ),
 ( 0.000000000000000000, 1.000000000000000000 ),
 .UNSPECIFIED. ) ;
#7351 = CARTESIAN_POINT ( 'NONE',  ( -10.68551981713787136, -12.73596763222149164, 64.28308208171728211 ) ) ;
#7352 = CARTESIAN_POINT ( 'NONE',  ( -10.70296955259081351, -11.59513340129999648, 71.27356289404251299 ) ) ;
#7353 = CIRCLE ( 'NONE', #40337, 0.2400000000000006295 ) ;
#7354 = LINE ( 'NONE', #40818, #2433 ) ;
#7355 = EDGE_LOOP ( 'NONE', ( #11017, #16189 ) ) ;
#7356 = DIRECTION ( 'NONE',  ( 1.000000000000000000, 1.669677910507523057E-21, 6.493791346278465266E-22 ) ) ;
#7357 = EDGE_CURVE ( 'NONE', #21857, #20491, #13613, .T. ) ;
#7358 = CARTESIAN_POINT ( 'NONE',  ( -24.17273098822645494, -12.76985232770863021, 69.77243020554645625 ) ) ;
#7359 = CARTESIAN_POINT ( 'NONE',  ( -21.34581862946232889, -20.66775363590295100, 72.52446429492309221 ) ) ;
#7360 = ORIENTED_EDGE ( 'NONE', *, *, #12824, .T. ) ;
#7361 = CARTESIAN_POINT ( 'NONE',  ( -10.43707426929608673, -13.86785048687512756, 57.45384848714355996 ) ) ;
#7362 = CARTESIAN_POINT ( 'NONE',  ( -21.94239094699587511, -20.22099839777041907, 58.91442899523080001 ) ) ;
#7363 = LINE ( 'NONE', #28838, #24479 ) ;
#7364 = ORIENTED_EDGE ( 'NONE', *, *, #11905, .T. ) ;
#7365 = PLANE ( 'NONE',  #6298 ) ;
#7366 = ORIENTED_EDGE ( 'NONE', *, *, #38391, .F. ) ;
#7367 = DIRECTION ( 'NONE',  ( 0.000000000000000000, -0.9999954153791273948, -0.003028072113819838245 ) ) ;
#7368 = CARTESIAN_POINT ( 'NONE',  ( -23.34481640033245853, -18.63641755246780107, 69.59371984262205046 ) ) ;
#7369 = ORIENTED_EDGE ( 'NONE', *, *, #8609, .T. ) ;
#7370 = DIRECTION ( 'NONE',  ( 0.9956360040033425118, -0.09332174201254556101, 0.000000000000000000 ) ) ;
#7371 = CARTESIAN_POINT ( 'NONE',  ( -12.41315173547891781, -9.850077678253004621, 57.38935532239157311 ) ) ;
#7372 = ORIENTED_EDGE ( 'NONE', *, *, #7513, .T. ) ;
#7373 = CARTESIAN_POINT ( 'NONE',  ( -21.35244737031881712, -20.60314787972549055, 72.82446376343101235 ) ) ;
#7374 = CARTESIAN_POINT ( 'NONE',  ( -19.77435985551070274, -21.87886194922281646, 65.64981515446680760 ) ) ;
#7375 = FACE_OUTER_BOUND ( 'NONE', #44179, .T. ) ;
#7376 = EDGE_LOOP ( 'NONE', ( #28946, #22586, #26965, #31523, #35413 ) ) ;
#7377 = CARTESIAN_POINT ( 'NONE',  ( -15.03263910315855512, -8.176888424288378587, 56.86472059657746314 ) ) ;
#7378 = ADVANCED_FACE ( 'NONE', ( #33738 ), #37607, .T. ) ;
#7379 = FACE_OUTER_BOUND ( 'NONE', #36818, .T. ) ;
#7380 = DIRECTION ( 'NONE',  ( 2.027460367431315085E-06, 1.195255636818703571E-05, -0.9999999999265127837 ) ) ;
#7381 = EDGE_CURVE ( 'NONE', #18890, #5301, #40897, .T. ) ;
#7382 = EDGE_CURVE ( 'NONE', #5194, #34163, #39085, .T. ) ;
#7383 = CIRCLE ( 'NONE', #4215, 5.249999999999998224 ) ;
#7384 = VERTEX_POINT ( 'NONE', #9067 ) ;
#7385 = ORIENTED_EDGE ( 'NONE', *, *, #40033, .F. ) ;
#7386 = CARTESIAN_POINT ( 'NONE',  ( -46.29409385541305966, -14.20920654474410760, 71.05212771298751306 ) ) ;
#7387 = DIRECTION ( 'NONE',  ( -0.8447509909909771686, 0.5351595679979589404, 0.000000000000000000 ) ) ;
#7388 = DIRECTION ( 'NONE',  ( -0.5820088206811425691, 0.8131824719270214219, -7.019974882119856712E-08 ) ) ;
#7389 = CARTESIAN_POINT ( 'NONE',  ( 18.62590614458706995, 1.890747609047893185, 50.53028072113869484 ) ) ;
#7390 = CARTESIAN_POINT ( 'NONE',  ( -16.87409385759798752, -6.859212275519751323, 50.50378509014259265 ) ) ;
#7391 = CARTESIAN_POINT ( 'NONE',  ( -20.25191534917341230, -8.350868906188830820, 70.26572394742477456 ) ) ;
#7392 = FACE_OUTER_BOUND ( 'NONE', #38004, .T. ) ;
#7393 = CARTESIAN_POINT ( 'NONE',  ( -36.42409385541304800, -8.109206544743658540, 50.50000000000030553 ) ) ;
#7394 = CARTESIAN_POINT ( 'NONE',  ( -17.15406633445637397, -7.764231093976030174, 70.78476080101584955 ) ) ;
#7395 = ORIENTED_EDGE ( 'NONE', *, *, #30851, .T. ) ;
#7396 = LINE ( 'NONE', #41605, #41482 ) ;
#7397 = CARTESIAN_POINT ( 'NONE',  ( -14.81662578951906184, -8.255127344917362109, 64.08978803669116076 ) ) ;
#7398 = CARTESIAN_POINT ( 'NONE',  ( -12.81450638858427737, -9.474958432310776502, 74.46923006088778152 ) ) ;
#7399 = VERTEX_POINT ( 'NONE', #5128 ) ;
#7400 = ORIENTED_EDGE ( 'NONE', *, *, #47455, .F. ) ;
#7401 = EDGE_CURVE ( 'NONE', #42690, #24436, #35144, .T. ) ;
#7402 = DIRECTION ( 'NONE',  ( -0.7171836970970658642, 0.6968841687240311389, -4.479616660400631173E-09 ) ) ;
#7403 = PRESENTATION_STYLE_ASSIGNMENT (( #30057 ) ) ;
#7404 = CARTESIAN_POINT ( 'NONE',  ( -11.40851146197636012, -18.49244098807202974, 64.83887356883496977 ) ) ;
#7405 = ORIENTED_EDGE ( 'NONE', *, *, #41247, .F. ) ;
#7406 = CARTESIAN_POINT ( 'NONE',  ( -23.46260529264824157, -11.17067950781535579, 73.36193301757424479 ) ) ;
#7407 = AXIS2_PLACEMENT_3D ( 'NONE', #1751, #16743, #31785 ) ;
#7408 = FACE_OUTER_BOUND ( 'NONE', #21590, .T. ) ;
#7409 = ADVANCED_FACE ( 'NONE', ( #46733 ), #46246, .T. ) ;
#7410 = CIRCLE ( 'NONE', #27821, 1.999999999999999556 ) ;
#7411 = ORIENTED_EDGE ( 'NONE', *, *, #42946, .T. ) ;
#7412 = FACE_OUTER_BOUND ( 'NONE', #14050, .T. ) ;
#7413 = ADVANCED_FACE ( 'NONE', ( #22683 ), #16909, .T. ) ;
#7414 = LINE ( 'NONE', #41132, #21032 ) ;
#7415 = CARTESIAN_POINT ( 'NONE',  ( -24.77723877343947478, -16.00713684962007122, 66.24820200538215431 ) ) ;
#7416 = ORIENTED_EDGE ( 'NONE', *, *, #8575, .T. ) ;
#7417 = DIRECTION ( 'NONE',  ( 2.866981220435666553E-17, -1.000000000000000000, -1.190614954331866791E-16 ) ) ;
#7418 = ORIENTED_EDGE ( 'NONE', *, *, #5941, .F. ) ;
#7419 = CARTESIAN_POINT ( 'NONE',  ( -10.44370662133100325, -17.41289724721067600, 64.76705995214548750 ) ) ;
#7420 = CARTESIAN_POINT ( 'NONE',  ( -12.60227155074094441, -19.95281705956671559, 68.35129494334645983 ) ) ;
#7421 = ORIENTED_EDGE ( 'NONE', *, *, #15124, .T. ) ;
#7422 = DIRECTION ( 'NONE',  ( 8.766499717996234600E-07, 3.805972784084494839E-07, -0.9999999999995433653 ) ) ;
#7423 = CARTESIAN_POINT ( 'NONE',  ( -20.12075396405374406, -21.75404021237947916, 72.50504483600978745 ) ) ;
#7424 = CARTESIAN_POINT ( 'NONE',  ( -21.54284385650551314, -8.811426318492348031, 52.18089403414751359 ) ) ;
#7425 = CARTESIAN_POINT ( 'NONE',  ( -21.35693516282594828, -21.13669309701779397, 69.23262968960160890 ) ) ;
#7426 = CARTESIAN_POINT ( 'NONE',  ( -10.05862351292959467, -15.92886012141397245, 64.69266982328383619 ) ) ;
#7427 = DIRECTION ( 'NONE',  ( 0.9942595023566571655, -0.1069955231469582047, 3.800058679842194246E-08 ) ) ;
#7428 = CARTESIAN_POINT ( 'NONE',  ( -16.61119863413175679, -21.81222516549900092, 65.52564366564290310 ) ) ;
#7429 = ORIENTED_EDGE ( 'NONE', *, *, #19200, .T. ) ;
#7430 = CARTESIAN_POINT ( 'NONE',  ( -12.24602769423020199, -10.02462455777539141, 60.85358326865326717 ) ) ;
#7431 = LINE ( 'NONE', #17748, #45514 ) ;
#7432 = CARTESIAN_POINT ( 'NONE',  ( -41.80424091423658695, -14.80920654474421205, 67.95882352941174531 ) ) ;
#7433 = CARTESIAN_POINT ( 'NONE',  ( -10.76785811675247118, -12.48515291162924434, 57.61385273545094066 ) ) ;
#7434 = FACE_OUTER_BOUND ( 'NONE', #14137, .T. ) ;
#7435 = B_SPLINE_CURVE_WITH_KNOTS ( 'NONE', 1,
 ( #31792, #17483 ),
 .UNSPECIFIED., .F., .F.,
 ( 2, 2 ),
 ( 0.000000000000000000, 1.000000000000000000 ),
 .UNSPECIFIED. ) ;
#7436 = CARTESIAN_POINT ( 'NONE',  ( -12.85799447202792045, -15.86467737382985632, 49.52966884056655772 ) ) ;
#7437 = ADVANCED_FACE ( 'NONE', ( #12975 ), #16672, .T. ) ;
#7438 = EDGE_CURVE ( 'NONE', #22280, #3333, #9307, .T. ) ;
#7439 = ORIENTED_EDGE ( 'NONE', *, *, #31904, .T. ) ;
#7440 = ORIENTED_EDGE ( 'NONE', *, *, #33169, .F. ) ;
#7441 = CARTESIAN_POINT ( 'NONE',  ( -17.42409385541299471, -14.80920654474435594, 52.02966884056656482 ) ) ;
#7442 = VERTEX_POINT ( 'NONE', #42794 ) ;
#7444 = DIRECTION ( 'NONE',  ( 0.5540494244615070674, -0.8324837747691378187, 8.494877338007802962E-17 ) ) ;
#7443 = CARTESIAN_POINT ( 'NONE',  ( -14.70574402281689963, -21.31410033361279233, 58.16617881512491550 ) ) ;
#7445 = CYLINDRICAL_SURFACE ( 'NONE', #23200, 1.249999999999998668 ) ;
#7446 = CARTESIAN_POINT ( 'NONE',  ( -15.68725519569583504, -21.64564087395307368, 72.25395315099507343 ) ) ;
#7447 = CARTESIAN_POINT ( 'NONE',  ( -14.60635853056651001, -21.70587488938233278, 58.20971981907628390 ) ) ;
#7448 =( BOUNDED_SURFACE ( )  B_SPLINE_SURFACE ( 3, 1, ( 
 ( #24198, #43152 ),
 ( #17513, #32542 ),
 ( #27881, #44141 ),
 ( #48523, #2976 ),
 ( #22194, #44856 ),
 ( #11112, #21473 ),
 ( #3465, #26133 ) ),
 .UNSPECIFIED., .T., .F., .F. ) 
 B_SPLINE_SURFACE_WITH_KNOTS ( ( 4, 3, 4 ),
 ( 2, 2 ),
 ( 0.000000000000000000, 0.5000000000000000000, 1.000000000000000000 ),
 ( 0.000000000000000000, 1.000000000000000000 ),
 .UNSPECIFIED. ) 
 GEOMETRIC_REPRESENTATION_ITEM ( )  RATIONAL_B_SPLINE_SURFACE ( (
 ( 1.000000000000000000, 1.000000000000000000),
 ( 0.3333333333333335369, 0.3333333333333330373),
 ( 0.3333333333333335369, 0.3333333333333330373),
 ( 1.000000000000000000, 1.000000000000000000),
 ( 0.3333333333333333703, 0.3333333333333333703),
 ( 0.3333333333333333703, 0.3333333333333333703),
 ( 1.000000000000000000, 1.000000000000000000) ) ) 
 REPRESENTATION_ITEM ( '' )  SURFACE ( )  );
#7449 = FACE_BOUND ( 'NONE', #41795, .T. ) ;
#7450 = CARTESIAN_POINT ( 'NONE',  ( -24.29522497960104843, -16.38737818751056352, 59.12332460191262840 ) ) ;
#7451 = AXIS2_PLACEMENT_3D ( 'NONE', #45358, #38184, #11133 ) ;
#7452 = ADVANCED_FACE ( 'NONE', ( #39333, #31706 ), #18985, .T. ) ;
#7453 = ADVANCED_FACE ( 'NONE', ( #20633 ), #287, .T. ) ;
#7454 = LINE ( 'NONE', #30105, #19677 ) ;
#7455 = CARTESIAN_POINT ( 'NONE',  ( -23.70135507383723805, -11.71146680393053607, 62.95218278684509983 ) ) ;
#7456 = ORIENTED_EDGE ( 'NONE', *, *, #9354, .F. ) ;
#7457 = AXIS2_PLACEMENT_3D ( 'NONE', #26026, #18370, #42448 ) ;
#7458 = CARTESIAN_POINT ( 'NONE',  ( -16.54004712951985923, -22.20656829664746468, 65.37564387897450047 ) ) ;
#7459 = CARTESIAN_POINT ( 'NONE',  ( -10.88286923018596575, -17.43962093083235843, 68.11193994895104709 ) ) ;
#7460 = EDGE_CURVE ( 'NONE', #3087, #36239, #42564, .T. ) ;
#7461 = CARTESIAN_POINT ( 'NONE',  ( -42.81012326717776517, -14.80920654474412679, 59.91176470588234793 ) ) ;
#7462 = EDGE_CURVE ( 'NONE', #19053, #36634, #10953, .T. ) ;
#7463 = CYLINDRICAL_SURFACE ( 'NONE', #35819, 0.1500000000000051015 ) ;
#7464 = PLANE ( 'NONE',  #1730 ) ;
#7465 = CARTESIAN_POINT ( 'NONE',  ( -36.42409385541304800, -8.109206544743658540, 50.50000000000030553 ) ) ;
#7466 = CARTESIAN_POINT ( 'NONE',  ( -23.78758865751629514, -10.93498413477609255, 73.40547355347567304 ) ) ;
#7467 =( BOUNDED_CURVE ( )  B_SPLINE_CURVE ( 3, ( #42623, #46306, #38666, #12562 ),
 .UNSPECIFIED., .F., .F. ) 
 B_SPLINE_CURVE_WITH_KNOTS ( ( 4, 4 ),
 ( 1.570796326794896558, 1.780235837034217505 ),
 .UNSPECIFIED. ) 
 CURVE ( )  GEOMETRIC_REPRESENTATION_ITEM ( )  RATIONAL_B_SPLINE_CURVE ( ( 1.000000000000000000, 0.9963479302455154896, 0.9963479302455154896, 1.000000000000000000 ) ) 
 REPRESENTATION_ITEM ( '' )  );
#7468 = VERTEX_POINT ( 'NONE', #26620 ) ;
#7469 = ORIENTED_EDGE ( 'NONE', *, *, #18299, .F. ) ;
#7470 = CARTESIAN_POINT ( 'NONE',  ( -15.43659385541304019, -8.995762431863214559, 51.38120296130585274 ) ) ;
#7471 = VERTEX_POINT ( 'NONE', #28003 ) ;
#7472 = B_SPLINE_CURVE_WITH_KNOTS ( 'NONE', 3,
 ( #36878, #25339, #3165, #48458, #6625, #33185, #21642, #29763, #48220, #44793 ),
 .UNSPECIFIED., .F., .F.,
 ( 4, 2, 2, 2, 4 ),
 ( 0.1272669073658833083, 0.2522669073488315039, 0.3772669073317797550, 0.5022669073147280061, 0.6272669072976762017 ),
 .UNSPECIFIED. ) ;
#7473 = ADVANCED_FACE ( 'NONE', ( #24326 ), #23846, .T. ) ;
#7474 = CARTESIAN_POINT ( 'NONE',  ( -15.80534385759798788, -7.595227055684746986, 51.75156210489594599 ) ) ;
#7475 = DIRECTION ( 'NONE',  ( -3.071710424422018668E-17, 6.404604876783312462E-16, 1.000000000000000000 ) ) ;
#7476 = CARTESIAN_POINT ( 'NONE',  ( -11.26648862653211935, -11.47983201339611981, 64.16384439635776005 ) ) ;
#7477 = CARTESIAN_POINT ( 'NONE',  ( -21.36489679027069499, -8.963475500412677377, 73.60128753237400190 ) ) ;
#7478 = ORIENTED_EDGE ( 'NONE', *, *, #45815, .T. ) ;
#7479 = CARTESIAN_POINT ( 'NONE',  ( -23.12535539932854078, -10.01343808792704237, 66.65686846082743955 ) ) ;
#7480 = DIRECTION ( 'NONE',  ( -5.731567514496413899E-31, -1.020425574103664789E-16, -1.000000000000000000 ) ) ;
#7481 = ORIENTED_EDGE ( 'NONE', *, *, #47868, .T. ) ;
#7482 = CARTESIAN_POINT ( 'NONE',  ( -10.37181755932410532, -14.66692344988656238, 75.09779103571921155 ) ) ;
#7483 = CARTESIAN_POINT ( 'NONE',  ( -23.97105468032384579, -17.28687603139987772, 69.71339789080803939 ) ) ;
#7484 = VECTOR ( 'NONE', #16025, 1000.000000000000000 ) ;
#7485 = ORIENTED_EDGE ( 'NONE', *, *, #19500, .T. ) ;
#7486 = CARTESIAN_POINT ( 'NONE',  ( -22.53429313110963506, -9.952421254863264011, 73.78161091678163075 ) ) ;
#7487 = DIRECTION ( 'NONE',  ( 7.340779720199402358E-07, -8.195271891664201640E-07, 0.9999999999993947064 ) ) ;
#7488 = CARTESIAN_POINT ( 'NONE',  ( -23.16791676868475491, -10.71612278230448823, 60.01692287334890352 ) ) ;
#7489 = ORIENTED_EDGE ( 'NONE', *, *, #26517, .T. ) ;
#7490 = CARTESIAN_POINT ( 'NONE',  ( -10.89650306282988090, -11.21840595405411101, 64.34156176843734443 ) ) ;
#7491 = AXIS2_PLACEMENT_3D ( 'NONE', #19886, #34888, #16161 ) ;
#7492 = LINE ( 'NONE', #22492, #46213 ) ;
#7493 = ADVANCED_FACE ( 'NONE', ( #12504 ), #1667, .F. ) ;
#7494 = CARTESIAN_POINT ( 'NONE',  ( -42.04247620835423760, -14.90920654474420104, 66.05294117647058272 ) ) ;
#7495 = VERTEX_POINT ( 'NONE', #16177 ) ;
#7496 = CARTESIAN_POINT ( 'NONE',  ( -10.85811841353450369, -12.22020323829153554, 74.71407760726656022 ) ) ;
#7497 = DIRECTION ( 'NONE',  ( -3.071710424422018668E-17, 6.404604876783312462E-16, 1.000000000000000000 ) ) ;
#7498 = CARTESIAN_POINT ( 'NONE',  ( -24.72409385541305582, -14.80920654474425291, 71.98235294117645822 ) ) ;
#7499 = CARTESIAN_POINT ( 'NONE',  ( -11.42587710518540334, -11.10406226247761019, 57.49431069621225276 ) ) ;
#7500 = CARTESIAN_POINT ( 'NONE',  ( -19.09284385650552096, -7.406986770994972602, 48.81910596585309747 ) ) ;
#7501 = EDGE_CURVE ( 'NONE', #8065, #7167, #27525, .T. ) ;
#7502 = EDGE_LOOP ( 'NONE', ( #45119, #18041, #33546, #34238, #47057 ) ) ;
#7503 = CARTESIAN_POINT ( 'NONE',  ( -17.77921064978749044, -22.25082400685520057, 58.59048811498988840 ) ) ;
#7504 = CARTESIAN_POINT ( 'NONE',  ( -14.41828383943595959, -8.428772226827717873, 63.67490250008367525 ) ) ;
#7505 = ORIENTED_EDGE ( 'NONE', *, *, #10591, .T. ) ;
#7506 = CARTESIAN_POINT ( 'NONE',  ( -11.32985570452711777, -19.09447181111026381, 68.32351299657294419 ) ) ;
#7507 = CYLINDRICAL_SURFACE ( 'NONE', #30574, 4.686499999999997002 ) ;
#7508 = LINE ( 'NONE', #7005, #27461 ) ;
#7509 = ORIENTED_EDGE ( 'NONE', *, *, #38603, .T. ) ;
#7510 = CARTESIAN_POINT ( 'NONE',  ( -10.69617340855713827, -12.87194068125527302, 67.81002665770238025 ) ) ;
#7511 = ORIENTED_EDGE ( 'NONE', *, *, #10767, .F. ) ;
#7512 = CARTESIAN_POINT ( 'NONE',  ( -13.07409385650551847, -9.792211528768506312, 50.49490371617623197 ) ) ;
#7513 = EDGE_CURVE ( 'NONE', #20304, #12385, #14008, .T. ) ;
#7514 = EDGE_CURVE ( 'NONE', #48327, #40177, #17985, .T. ) ;
#7515 = CARTESIAN_POINT ( 'NONE',  ( -11.03149232240643052, -10.98320184173030256, 60.93531726291125494 ) ) ;
#7516 = LINE ( 'NONE', #3812, #27534 ) ;
#7517 = B_SPLINE_CURVE_WITH_KNOTS ( 'NONE', 3,
 ( #7982, #27394, #4754, #22997, #37985, #15320, #46114, #45651, #7490, #30138 ),
 .UNSPECIFIED., .F., .F.,
 ( 4, 2, 2, 2, 4 ),
 ( 0.1272669073658008188, 0.2522669073439062215, 0.3772669073220116243, 0.5022669073001170270, 0.6272669072782224298 ),
 .UNSPECIFIED. ) ;
#7518 = CARTESIAN_POINT ( 'NONE',  ( -10.76763519559319882, -17.13171766695033327, 61.15743118826002700 ) ) ;
#7519 = ORIENTED_EDGE ( 'NONE', *, *, #37454, .T. ) ;
#7520 = ORIENTED_EDGE ( 'NONE', *, *, #47557, .F. ) ;
#7521 = AXIS2_PLACEMENT_3D ( 'NONE', #12935, #5578, #2822 ) ;
#7522 = CARTESIAN_POINT ( 'NONE',  ( -15.46784385650551918, -6.428312510596451368, 51.20221977374900035 ) ) ;
#7523 = CIRCLE ( 'NONE', #35017, 4.686499999999999666 ) ;
#7524 = DIRECTION ( 'NONE',  ( -0.000000000000000000, -1.000000000000000000, -0.000000000000000000 ) ) ;
#7525 = CARTESIAN_POINT ( 'NONE',  ( -9.534148923395315833, -8.271570107951246698, 53.49999999999995026 ) ) ;
#7526 = ADVANCED_FACE ( 'NONE', ( #39815 ), #35864, .T. ) ;
#7527 = CARTESIAN_POINT ( 'NONE',  ( -16.03034385650551386, -9.794322478646142471, 51.19202720610083901 ) ) ;
#7528 = EDGE_LOOP ( 'NONE', ( #45871, #33952, #9370, #18364 ) ) ;
#7529 = DIRECTION ( 'NONE',  ( 0.9687793358424821033, -0.2479245821708680464, 0.000000000000000000 ) ) ;
#7530 = CARTESIAN_POINT ( 'NONE',  ( -21.67230677980763431, -11.72453687863643701, 49.52966884056655772 ) ) ;
#7531 = ORIENTED_EDGE ( 'NONE', *, *, #39587, .F. ) ;
#7532 = DIRECTION ( 'NONE',  ( -0.9687793358424819923, 0.2479245821708680464, 0.000000000000000000 ) ) ;
#7533 = EDGE_LOOP ( 'NONE', ( #48591, #18366, #42982, #12694, #10875 ) ) ;
#7534 = CARTESIAN_POINT ( 'NONE',  ( -12.58579432961061606, -9.143940464819721115, 74.44206132019799327 ) ) ;
#7535 = CARTESIAN_POINT ( 'NONE',  ( -10.11541557277654313, -16.25427077284050270, 71.60896933323357416 ) ) ;
#7536 = CARTESIAN_POINT ( 'NONE',  ( -16.29155950929526497, -19.35680461458998636, 49.52966884056656482 ) ) ;
#7537 = CARTESIAN_POINT ( 'NONE',  ( -17.46159385541293929, -7.228003583437990542, 51.38655588711998945 ) ) ;
#7538 = ORIENTED_EDGE ( 'NONE', *, *, #29440, .F. ) ;
#7539 = CARTESIAN_POINT ( 'NONE',  ( -20.06975372951847447, -8.274133229585533655, 73.73568642813194174 ) ) ;
#7540 = CARTESIAN_POINT ( 'NONE',  ( -15.32518304399999387, -21.95751765168108349, 72.16080051677664642 ) ) ;
#7541 = EDGE_CURVE ( 'NONE', #42734, #43742, #3072, .T. ) ;
#7542 = CARTESIAN_POINT ( 'NONE',  ( -13.13835185842056674, -9.211395881110181705, 67.37942811378734120 ) ) ;
#7543 = CARTESIAN_POINT ( 'NONE',  ( -19.84608771793053705, -21.43027439227859077, 69.22922701166929471 ) ) ;
#7544 = EDGE_LOOP ( 'NONE', ( #3803, #12389, #16459, #30673 ) ) ;
#7545 = B_SPLINE_CURVE_WITH_KNOTS ( 'NONE', 3,
 ( #800, #30856, #6434, #21454, #5715, #17251, #10372, #13306, #32296, #36207 ),
 .UNSPECIFIED., .F., .F.,
 ( 4, 2, 2, 2, 4 ),
 ( 0.1272669073658491412, 0.2522669073463209566, 0.3772669073267927997, 0.5022669073072645318, 0.6272669072877363750 ),
 .UNSPECIFIED. ) ;
#7546 = CARTESIAN_POINT ( 'NONE',  ( -22.71059208588729561, -10.14448404190931186, 70.02650598627910483 ) ) ;
#7547 = DIRECTION ( 'NONE',  ( -0.9529680021988312655, 0.3030709269876716294, 3.918663088761644638E-08 ) ) ;
#7548 = CARTESIAN_POINT ( 'NONE',  ( -12.57222285659330119, -19.85510226960975899, 64.86674893738813807 ) ) ;
#7549 = AXIS2_PLACEMENT_3D ( 'NONE', #6652, #48016, #6416 ) ;
#7550 = FACE_BOUND ( 'NONE', #46042, .T. ) ;
#7551 = ORIENTED_EDGE ( 'NONE', *, *, #500, .T. ) ;
#7552 = CARTESIAN_POINT ( 'NONE',  ( 18.62590614458706995, 1.890747609047893185, 50.53028072113869484 ) ) ;
#7553 = DIRECTION ( 'NONE',  ( -2.866981220435666553E-17, 1.000000000000000000, 1.190614954331866791E-16 ) ) ;
#7554 = CARTESIAN_POINT ( 'NONE',  ( -13.06813783877040791, -9.265530354883376063, 67.66470656304637998 ) ) ;
#7555 = DIRECTION ( 'NONE',  ( -2.200805985157658208E-07, -3.006001589187115340E-06, -0.9999999999954577445 ) ) ;
#7556 = ORIENTED_EDGE ( 'NONE', *, *, #8949, .T. ) ;
#7557 = CARTESIAN_POINT ( 'NONE',  ( -14.13242279744181573, -8.574497162196568212, 74.21426705364891063 ) ) ;
#7558 = ORIENTED_EDGE ( 'NONE', *, *, #17524, .T. ) ;
#7559 = CARTESIAN_POINT ( 'NONE',  ( -17.81466184404888509, -7.769993126244952641, 60.08060774817733574 ) ) ;
#7560 = FACE_OUTER_BOUND ( 'NONE', #16673, .T. ) ;
#7561 = CARTESIAN_POINT ( 'NONE',  ( -21.61180957605408537, -8.647524312981719419, 73.70854620271380497 ) ) ;
#7562 = ORIENTED_EDGE ( 'NONE', *, *, #42975, .F. ) ;
#7563 = CARTESIAN_POINT ( 'NONE',  ( -10.60286062419423914, -17.80505434777429841, 71.74530924410473176 ) ) ;
#7564 = DIRECTION ( 'NONE',  ( 1.224646799147353207E-16, 1.000000000000000000, -1.912410701131276611E-32 ) ) ;
#7565 = ORIENTED_EDGE ( 'NONE', *, *, #38303, .F. ) ;
#7566 = ORIENTED_EDGE ( 'NONE', *, *, #42142, .T. ) ;
#7567 = ORIENTED_EDGE ( 'NONE', *, *, #48159, .F. ) ;
#7568 = DIRECTION ( 'NONE',  ( -2.866981220435666553E-17, 1.000000000000000000, 1.190614954331866791E-16 ) ) ;
#7569 = EDGE_CURVE ( 'NONE', #6936, #48202, #42676, .T. ) ;
#7570 = FACE_OUTER_BOUND ( 'NONE', #16719, .T. ) ;
#7571 = CARTESIAN_POINT ( 'NONE',  ( -21.15336808330806662, -20.73310000539657949, 69.35450185099439580 ) ) ;
#7572 = EDGE_CURVE ( 'NONE', #946, #37616, #28888, .T. ) ;
#7573 = CARTESIAN_POINT ( 'NONE',  ( -16.79181145072023185, -21.83380975027498039, 65.11075561446135396 ) ) ;
#7574 = CARTESIAN_POINT ( 'NONE',  ( -14.82422806554511929, -10.90997840001177721, 49.52966884056655772 ) ) ;
#7575 = CYLINDRICAL_SURFACE ( 'NONE', #8254, 1.999999999999999112 ) ;
#7576 = CARTESIAN_POINT ( 'NONE',  ( -13.42364920204782841, -9.064338107659910548, 49.69363550579117117 ) ) ;
#7577 = ORIENTED_EDGE ( 'NONE', *, *, #45036, .F. ) ;
#7578 = VERTEX_POINT ( 'NONE', #2863 ) ;
#7579 = B_SPLINE_CURVE_WITH_KNOTS ( 'NONE', 3,
 ( #35519, #43160, #32074, #5746, #46621, #32325, #9434, #16303, #47349, #24459 ),
 .UNSPECIFIED., .F., .F.,
 ( 4, 2, 2, 2, 4 ),
 ( 0.6272669072877639085, 0.7522669073072798529, 0.8772669073267959083, 1.002266907346311964, 1.127266907365827908 ),
 .UNSPECIFIED. ) ;
#7580 = EDGE_CURVE ( 'NONE', #5194, #40684, #47693, .T. ) ;
#7581 = CARTESIAN_POINT ( 'NONE',  ( -16.19792114999740562, -7.866354181730329742, 60.48556343814865954 ) ) ;
#7582 = CARTESIAN_POINT ( 'NONE',  ( -22.48430581236326731, -20.27711595259535571, 65.81926302645771898 ) ) ;
#7583 = DIRECTION ( 'NONE',  ( -3.485387654165294196E-16, 2.355958133329952458E-32, -1.000000000000000000 ) ) ;
#7584 = EDGE_CURVE ( 'NONE', #10113, #38529, #28503, .T. ) ;
#7585 = DIRECTION ( 'NONE',  ( 0.000000000000000000, 0.000000000000000000, 1.000000000000000000 ) ) ;
#7586 = VERTEX_POINT ( 'NONE', #47936 ) ;
#7587 = EDGE_CURVE ( 'NONE', #37103, #4167, #40064, .T. ) ;
#7588 =( BOUNDED_CURVE ( )  B_SPLINE_CURVE ( 3, ( #2595, #14122, #29179, #1864 ),
 .UNSPECIFIED., .F., .F. ) 
 B_SPLINE_CURVE_WITH_KNOTS ( ( 4, 4 ),
 ( 0.4074455897393613468, 0.5000000000000000000 ),
 .UNSPECIFIED. ) 
 CURVE ( )  GEOMETRIC_REPRESENTATION_ITEM ( )  RATIONAL_B_SPLINE_CURVE ( ( 0.6983129098260874024, 0.7760317562606928732, 0.8765941196519969614, 0.9999999999999992228 ) ) 
 REPRESENTATION_ITEM ( '' )  );
#7589 = CARTESIAN_POINT ( 'NONE',  ( -13.97409385650551528, -9.792211528768506312, 50.49490371617623197 ) ) ;
#7590 = VECTOR ( 'NONE', #22126, 1000.000000000000114 ) ;
#7591 = AXIS2_PLACEMENT_3D ( 'NONE', #28532, #46758, #13002 ) ;
#7592 = ORIENTED_EDGE ( 'NONE', *, *, #4205, .T. ) ;
#7593 = PLANE ( 'NONE',  #36641 ) ;
#7594 = LINE ( 'NONE', #41556, #44210 ) ;
#7595 = CARTESIAN_POINT ( 'NONE',  ( -21.99178500617274779, -9.439039195359633538, 59.72171213140594404 ) ) ;
#7596 = ORIENTED_EDGE ( 'NONE', *, *, #36521, .F. ) ;
#7597 = FACE_OUTER_BOUND ( 'NONE', #22535, .T. ) ;
#7598 =( BOUNDED_SURFACE ( )  B_SPLINE_SURFACE ( 3, 1, ( 
 ( #5378, #31469 ),
 ( #28010, #16186 ),
 ( #1911, #35398 ),
 ( #28264, #46014 ),
 ( #1676, #5136 ),
 ( #12267, #38856 ),
 ( #31714, #27290 ) ),
 .UNSPECIFIED., .T., .F., .F. ) 
 B_SPLINE_SURFACE_WITH_KNOTS ( ( 4, 3, 4 ),
 ( 2, 2 ),
 ( 0.000000000000000000, 0.5000000000000000000, 1.000000000000000000 ),
 ( 0.000000000000000000, 1.000000000000000000 ),
 .UNSPECIFIED. ) 
 GEOMETRIC_REPRESENTATION_ITEM ( )  RATIONAL_B_SPLINE_SURFACE ( (
 ( 1.000000000000000000, 1.000000000000000000),
 ( 0.3333333333333335369, 0.3333333333333330373),
 ( 0.3333333333333335369, 0.3333333333333330373),
 ( 1.000000000000000000, 1.000000000000000000),
 ( 0.3333333333333333703, 0.3333333333333333703),
 ( 0.3333333333333333703, 0.3333333333333333703),
 ( 1.000000000000000000, 1.000000000000000000) ) ) 
 REPRESENTATION_ITEM ( '' )  SURFACE ( )  );
#7599 = ADVANCED_FACE ( 'NONE', ( #6331 ), #6081, .T. ) ;
#7600 = CARTESIAN_POINT ( 'NONE',  ( -10.51729497052147977, -16.22293520194095606, 71.74750383215044280 ) ) ;
#7601 = CARTESIAN_POINT ( 'NONE',  ( -21.53401928346354310, -9.142769119308555403, 66.85253116148227548 ) ) ;
#7602 = ORIENTED_EDGE ( 'NONE', *, *, #32541, .T. ) ;
#7603 = LINE ( 'NONE', #22606, #7698 ) ;
#7604 = EDGE_CURVE ( 'NONE', #28537, #12407, #20371, .T. ) ;
#7605 = CARTESIAN_POINT ( 'NONE',  ( -14.41069671968389265, -11.21995593321280360, 49.52966884056655772 ) ) ;
#7606 = DIRECTION ( 'NONE',  ( -0.9501515917649785425, -0.3117883138709295898, 1.594035198720926202E-08 ) ) ;
#7607 = VERTEX_POINT ( 'NONE', #43769 ) ;
#7608 = CARTESIAN_POINT ( 'NONE',  ( -11.14069317138369719, -11.72368909046683072, 71.38860884459683120 ) ) ;
#7609 =( BOUNDED_CURVE ( )  B_SPLINE_CURVE ( 3, ( #17302, #32352, #43679, #44895 ),
 .UNSPECIFIED., .F., .F. ) 
 B_SPLINE_CURVE_WITH_KNOTS ( ( 4, 4 ),
 ( 4.712388980384690562, 4.921828490624010399 ),
 .UNSPECIFIED. ) 
 CURVE ( )  GEOMETRIC_REPRESENTATION_ITEM ( )  RATIONAL_B_SPLINE_CURVE ( ( 1.000000000000000000, 0.9963479302455154896, 0.9963479302455154896, 1.000000000000000000 ) ) 
 REPRESENTATION_ITEM ( '' )  );
#7610 = ORIENTED_EDGE ( 'NONE', *, *, #33760, .F. ) ;
#7611 = CARTESIAN_POINT ( 'NONE',  ( -42.16821150247189109, -14.90920654474419038, 65.04705882352939739 ) ) ;
#7612 = CARTESIAN_POINT ( 'NONE',  ( -11.49187567532494114, -18.52825065318211983, 64.85780276779384224 ) ) ;
#7613 = B_SPLINE_CURVE_WITH_KNOTS ( 'NONE', 3,
 ( #39856, #21633, #36389, #13730, #43809, #25330, #6373, #31989, #2669, #9831 ),
 .UNSPECIFIED., .F., .F.,
 ( 4, 2, 2, 2, 4 ),
 ( 0.000000000000000000, 0.2500000000000000000, 0.5000000000000000000, 0.7500000000000000000, 1.000000000000000000 ),
 .UNSPECIFIED. ) ;
#7614 = ORIENTED_EDGE ( 'NONE', *, *, #8323, .F. ) ;
#7615 = CARTESIAN_POINT ( 'NONE',  ( -13.38504989191835826, -9.021193483636507082, 67.52375889928833885 ) ) ;
#7616 = CARTESIAN_POINT ( 'NONE',  ( -24.53780083649505173, -12.59584922708229904, 69.95738295622972203 ) ) ;
#7617 = CARTESIAN_POINT ( 'NONE',  ( -20.20879974760366693, -8.386827295270064653, 70.25100337495888425 ) ) ;
#7618 = EDGE_LOOP ( 'NONE', ( #13729, #47553 ) ) ;
#7619 = CARTESIAN_POINT ( 'NONE',  ( -16.58751391467172098, -21.80939466075598077, 65.52564390317479592 ) ) ;
#7620 = CARTESIAN_POINT ( 'NONE',  ( -22.20320197231171733, -19.92390356480266433, 66.00421731406686376 ) ) ;
#7621 = DIRECTION ( 'NONE',  ( 0.6538427738826437796, 0.7566304428460743914, -5.916677973025938575E-08 ) ) ;
#7622 = ORIENTED_EDGE ( 'NONE', *, *, #35174, .T. ) ;
#7623 = EDGE_CURVE ( 'NONE', #16942, #5056, #17637, .T. ) ;
#7624 = CARTESIAN_POINT ( 'NONE',  ( -14.99424598590282365, -8.191132179135481195, 56.84999999999990195 ) ) ;
#7625 = VECTOR ( 'NONE', #15246, 999.9999999999998863 ) ;
#7626 = AXIS2_PLACEMENT_3D ( 'NONE', #43060, #27797, #13008 ) ;
#7627 = CARTESIAN_POINT ( 'NONE',  ( -13.38462805196022920, -20.58720062598995426, 58.34650077712429095 ) ) ;
#7628 = CARTESIAN_POINT ( 'NONE',  ( -16.99557573331350824, -4.388301432589208240, 54.58422952202461431 ) ) ;
#7629 = ORIENTED_EDGE ( 'NONE', *, *, #47973, .T. ) ;
#7630 = VERTEX_POINT ( 'NONE', #36578 ) ;
#7631 = CARTESIAN_POINT ( 'NONE',  ( -23.34553101626436700, -10.28815885117376716, 59.79477560945002779 ) ) ;
#7632 = CARTESIAN_POINT ( 'NONE',  ( -10.70671044302858022, -11.58740612280508842, 71.19522567356285947 ) ) ;
#7633 = DIRECTION ( 'NONE',  ( 3.413470714839332458E-33, -1.190614954331866791E-16, 1.000000000000000000 ) ) ;
#7634 = CARTESIAN_POINT ( 'NONE',  ( -10.39679176622870038, -14.24023819782134481, 64.40275955115841100 ) ) ;
#7635 = CARTESIAN_POINT ( 'NONE',  ( -13.72409385759798894, -9.359200813967568422, 50.49621490985803263 ) ) ;
#7636 = CARTESIAN_POINT ( 'NONE',  ( -24.44055745662519641, -14.11932379769929113, 73.13743607903229815 ) ) ;
#7637 = FACE_OUTER_BOUND ( 'NONE', #16896, .T. ) ;
#7638 = CARTESIAN_POINT ( 'NONE',  ( -23.83512934130040861, -17.76108582422602922, 66.08789927488301430 ) ) ;
#7639 = CARTESIAN_POINT ( 'NONE',  ( -21.95370832667365235, -13.56094844357179774, 49.52966884056655772 ) ) ;
#7640 = VERTEX_POINT ( 'NONE', #14167 ) ;
#7641 = EDGE_CURVE ( 'NONE', #8993, #10239, #29223, .T. ) ;
#7642 = CYLINDRICAL_SURFACE ( 'NONE', #29713, 0.1499999999999964140 ) ;
#7643 = B_SPLINE_CURVE_WITH_KNOTS ( 'NONE', 1,
 ( #37065, #33605 ),
 .UNSPECIFIED., .F., .F.,
 ( 2, 2 ),
 ( 0.000000000000000000, 1.000000000000000000 ),
 .UNSPECIFIED. ) ;
#7644 = EDGE_CURVE ( 'NONE', #28963, #25288, #29705, .T. ) ;
#7645 = CARTESIAN_POINT ( 'NONE',  ( -19.90432934692537614, -21.83431937171774706, 69.04987052938618319 ) ) ;
#7646 = B_SPLINE_CURVE_WITH_KNOTS ( 'NONE', 3,
 ( #18360, #44741, #19108, #8278, #34352, #887, #638, #30933, #16614, #1116 ),
 .UNSPECIFIED., .F., .F.,
 ( 4, 2, 2, 2, 4 ),
 ( 0.000000000000000000, 0.2500000000000000000, 0.5000000000000000000, 0.7500000000000000000, 1.000000000000000000 ),
 .UNSPECIFIED. ) ;
#7647 = VERTEX_POINT ( 'NONE', #33878 ) ;
#7648 = EDGE_LOOP ( 'NONE', ( #14952, #28828 ) ) ;
#7649 = CARTESIAN_POINT ( 'NONE',  ( -22.67409364490373491, -14.81069326838761135, 49.52966884056655772 ) ) ;
#7650 = DIRECTION ( 'NONE',  ( 1.927470528863184130E-16, 1.434740771370715221E-29, -1.000000000000000000 ) ) ;
#7651 = CARTESIAN_POINT ( 'NONE',  ( -15.32518304399999387, -21.95751765168108349, 72.16080051677664642 ) ) ;
#7652 = DIRECTION ( 'NONE',  ( 0.9893874368562772803, -0.1453014101478918851, 3.604276813338690116E-17 ) ) ;
#7653 = ADVANCED_FACE ( 'NONE', ( #14643 ), #10997, .T. ) ;
#7654 = VERTEX_POINT ( 'NONE', #45233 ) ;
#7655 = EDGE_CURVE ( 'NONE', #28162, #2827, #7194, .T. ) ;
#7656 = CARTESIAN_POINT ( 'NONE',  ( -20.72574062298286535, -8.580111251864035893, 59.84125250080548852 ) ) ;
#7657 = AXIS2_PLACEMENT_3D ( 'NONE', #7822, #18617, #22092 ) ;
#7658 = PLANE ( 'NONE',  #10763 ) ;
#7659 = ADVANCED_FACE ( 'NONE', ( #8057 ), #19077, .T. ) ;
#7660 = EDGE_CURVE ( 'NONE', #36955, #21913, #26501, .T. ) ;
#7661 = VERTEX_POINT ( 'NONE', #26753 ) ;
#7662 = CARTESIAN_POINT ( 'NONE',  ( 18.07590614458695200, 2.989985547936196753, 50.78361045430852982 ) ) ;
#7663 = CARTESIAN_POINT ( 'NONE',  ( -17.50083907013572571, -21.86240119160683193, 58.49733361235234952 ) ) ;
#7664 = CARTESIAN_POINT ( 'NONE',  ( -24.32132670238839012, -16.30692182044891325, 66.20758098450045281 ) ) ;
#7665 = VERTEX_POINT ( 'NONE', #23065 ) ;
#7666 = DIRECTION ( 'NONE',  ( -0.9930145540378109148, 0.1179919296777755394, 4.526730167978063816E-08 ) ) ;
#7667 = ORIENTED_EDGE ( 'NONE', *, *, #17828, .T. ) ;
#7668 = CARTESIAN_POINT ( 'NONE',  ( -23.82366785274684418, -10.99486113721019009, 73.47697904737684382 ) ) ;
#7669 = CARTESIAN_POINT ( 'NONE',  ( -20.45862069896310231, -8.501076506802965227, 63.59656160843943695 ) ) ;
#7670 = VERTEX_POINT ( 'NONE', #4113 ) ;
#7671 = LINE ( 'NONE', #23168, #23901 ) ;
#7672 = CARTESIAN_POINT ( 'NONE',  ( -20.14513467918862233, -21.74452124448403723, 72.50455117424338880 ) ) ;
#7673 = CARTESIAN_POINT ( 'NONE',  ( -19.51784385650551457, -9.790100578890868377, 49.79778022625163203 ) ) ;
#7674 = FACE_OUTER_BOUND ( 'NONE', #26405, .T. ) ;
#7675 = CARTESIAN_POINT ( 'NONE',  ( 18.07590614458695200, 2.991499583993109113, 50.28361274661895663 ) ) ;
#7676 = CARTESIAN_POINT ( 'NONE',  ( -24.43113031232903865, -15.58634216689856800, 73.30303748141028564 ) ) ;
#7677 = CARTESIAN_POINT ( 'NONE',  ( -15.09544287645192284, -21.46351977604527761, 65.10596681500476279 ) ) ;
#7678 = ORIENTED_EDGE ( 'NONE', *, *, #1289, .T. ) ;
#7679 = CARTESIAN_POINT ( 'NONE',  ( -10.43687275975356599, -14.38543977226298587, 64.40306298683110242 ) ) ;
#7680 = CARTESIAN_POINT ( 'NONE',  ( -10.00073915290244564, -14.17087342314384735, 64.57459177551746166 ) ) ;
#7681 = LINE ( 'NONE', #41641, #41629 ) ;
#7682 = CARTESIAN_POINT ( 'NONE',  ( -10.85841931818429629, -17.37798394237198707, 64.91267318220633342 ) ) ;
#7683 = CARTESIAN_POINT ( 'NONE',  ( -10.39241571269986331, -17.41794234916963191, 47.99999999999994316 ) ) ;
#7684 = CARTESIAN_POINT ( 'NONE',  ( -13.33151401730585306, -20.55006798877650454, 58.06122216312902395 ) ) ;
#7685 = EDGE_CURVE ( 'NONE', #2617, #773, #15972, .T. ) ;
#7686 = ORIENTED_EDGE ( 'NONE', *, *, #43580, .T. ) ;
#7687 = ORIENTED_EDGE ( 'NONE', *, *, #15513, .F. ) ;
#7688 = CARTESIAN_POINT ( 'NONE',  ( -16.83291263600079191, -21.78581067597523813, 72.35470271977608547 ) ) ;
#7689 = DIRECTION ( 'NONE',  ( -0.1240347345892086062, 1.145860353393066553E-16, -0.9922778767136676281 ) ) ;
#7690 = ORIENTED_EDGE ( 'NONE', *, *, #36544, .T. ) ;
#7691 = CARTESIAN_POINT ( 'NONE',  ( -21.00380318978402627, -21.34292366101719196, 62.22975991904223747 ) ) ;
#7692 = DIRECTION ( 'NONE',  ( 4.267285103686815209E-17, -5.292884291094200710E-16, -1.000000000000000000 ) ) ;
#7693 = CARTESIAN_POINT ( 'NONE',  ( -11.61674064386953198, -18.71759577841732280, 65.03241660559515935 ) ) ;
#7694 = CARTESIAN_POINT ( 'NONE',  ( -10.46596968387485305, -15.57428492597166780, 57.64080867646067219 ) ) ;
#7695 = CARTESIAN_POINT ( 'NONE',  ( -40.92409385541305511, -14.80920654474410725, 74.99999999999998579 ) ) ;
#7696 = CARTESIAN_POINT ( 'NONE',  ( -10.79572441526863180, -11.40795732096215254, 67.80359905390240272 ) ) ;
#7697 = FACE_OUTER_BOUND ( 'NONE', #41283, .T. ) ;
#7698 = VECTOR ( 'NONE', #33411, 1000.000000000000000 ) ;
#7699 = CARTESIAN_POINT ( 'NONE',  ( -16.81376820967965457, -9.329655637006117885, 53.69233794759168887 ) ) ;
#7700 = CARTESIAN_POINT ( 'NONE',  ( -24.39640304805111981, -15.43122313838688164, 73.19406873947340841 ) ) ;
#7701 = CARTESIAN_POINT ( 'NONE',  ( -17.42409385541300182, -14.80920654474440745, 54.28066884056654828 ) ) ;
#7702 = PRESENTATION_STYLE_ASSIGNMENT (( #45855 ) ) ;
#7703 = CARTESIAN_POINT ( 'NONE',  ( -12.06147410079331195, -19.98082143093137830, 61.50404465172076840 ) ) ;
#7704 = AXIS2_PLACEMENT_3D ( 'NONE', #30383, #22250, #33298 ) ;
#7705 = DIRECTION ( 'NONE',  ( 0.000000000000000000, 0.000000000000000000, 1.000000000000000000 ) ) ;
#7706 = CARTESIAN_POINT ( 'NONE',  ( -24.59706363142188934, -12.79617847886399140, 66.48742024426742603 ) ) ;
#7707 = LINE ( 'NONE', #312, #19748 ) ;
#7708 = VECTOR ( 'NONE', #12869, 1000.000000000000114 ) ;
#7709 = ORIENTED_EDGE ( 'NONE', *, *, #46210, .T. ) ;
#7710 = ORIENTED_EDGE ( 'NONE', *, *, #11285, .T. ) ;
#7711 = ORIENTED_EDGE ( 'NONE', *, *, #12560, .T. ) ;
#7712 = CARTESIAN_POINT ( 'NONE',  ( -15.52409385759799143, -9.359200813967568422, 50.49621490985803263 ) ) ;
#7713 = DIRECTION ( 'NONE',  ( 0.4461977533473618363, -0.8949343913984794119, -2.476895096511286888E-17 ) ) ;
#7714 = CARTESIAN_POINT ( 'NONE',  ( -11.23206301587313050, -11.54443178946509008, 64.33985160186854557 ) ) ;
#7715 = EDGE_CURVE ( 'NONE', #3256, #20955, #11175, .T. ) ;
#7716 = ADVANCED_FACE ( 'NONE', ( #41517 ), #22562, .T. ) ;
#7717 = CARTESIAN_POINT ( 'NONE',  ( -16.98991503782990975, -22.24662993548692214, 72.35038528954983406 ) ) ;
#7718 = EDGE_LOOP ( 'NONE', ( #37718, #38382 ) ) ;
#7719 = DIRECTION ( 'NONE',  ( 0.8788484374452872894, -0.3260506722428090920, -0.3483050145059486957 ) ) ;
#7720 = AXIS2_PLACEMENT_3D ( 'NONE', #19329, #26969, #20065 ) ;
#7721 = CARTESIAN_POINT ( 'NONE',  ( -16.94712425470457973, -14.65920654474411045, 52.21286476528345588 ) ) ;
#7722 = ORIENTED_EDGE ( 'NONE', *, *, #30365, .F. ) ;
#7723 = CARTESIAN_POINT ( 'NONE',  ( -22.31982660061501633, -20.42496915584003148, 62.39585669079483665 ) ) ;
#7724 = DIRECTION ( 'NONE',  ( 0.9687793358424821033, -0.2479245821708679909, 0.000000000000000000 ) ) ;
#7725 = VECTOR ( 'NONE', #12920, 1000.000000000000000 ) ;
#7726 = VECTOR ( 'NONE', #24446, 1000.000000000000000 ) ;
#7727 = ORIENTED_EDGE ( 'NONE', *, *, #31153, .T. ) ;
#7728 = ADVANCED_FACE ( 'NONE', ( #34118 ), #533, .T. ) ;
#7729 = EDGE_CURVE ( 'NONE', #37849, #7068, #26986, .T. ) ;
#7730 = CARTESIAN_POINT ( 'NONE',  ( -24.72409385541305582, -14.80920654474415699, 62.92941176470587550 ) ) ;
#7731 = CARTESIAN_POINT ( 'NONE',  ( -21.00588228679873382, -20.88502978299158741, 69.46939052609951659 ) ) ;
#7732 = CARTESIAN_POINT ( 'NONE',  ( -17.21423163961297220, -7.362113418316746483, 70.68374130334144922 ) ) ;
#7733 = ORIENTED_EDGE ( 'NONE', *, *, #10699, .T. ) ;
#7734 = CARTESIAN_POINT ( 'NONE',  ( -10.59656512619885227, -13.05092609425065397, 68.02360230423870746 ) ) ;
#7735 = CYLINDRICAL_SURFACE ( 'NONE', #616, 1.249999999999998668 ) ;
#7736 = AXIS2_PLACEMENT_3D ( 'NONE', #39941, #28853, #6213 ) ;
#7737 =( BOUNDED_CURVE ( )  B_SPLINE_CURVE ( 3, ( #35564, #5554, #38776, #34836 ),
 .UNSPECIFIED., .F., .F. ) 
 B_SPLINE_CURVE_WITH_KNOTS ( ( 4, 4 ),
 ( 0.9074455897393708392, 1.000000000000000000 ),
 .UNSPECIFIED. ) 
 CURVE ( )  GEOMETRIC_REPRESENTATION_ITEM ( )  RATIONAL_B_SPLINE_CURVE ( ( 0.6983129098261093848, 0.7760317562607123021, 0.8765941196520091738, 1.000000000000000000 ) ) 
 REPRESENTATION_ITEM ( '' )  );
#7738 = CARTESIAN_POINT ( 'NONE',  ( -24.35831120643470982, -13.52022779156689936, 59.77756816219774549 ) ) ;
#7739 = CARTESIAN_POINT ( 'NONE',  ( -17.61266704711333375, -10.12650194148654137, 49.52966884056655772 ) ) ;
#7740 = ORIENTED_EDGE ( 'NONE', *, *, #23504, .T. ) ;
#7741 = CARTESIAN_POINT ( 'NONE',  ( -11.02242957576233273, -11.85532881267382166, 74.57312195644870201 ) ) ;
#7742 = DIRECTION ( 'NONE',  ( -1.078708504911322448E-05, -7.367657518828247499E-06, -0.9999999999146781393 ) ) ;
#7743 = AXIS2_PLACEMENT_3D ( 'NONE', #20881, #28517, #6096 ) ;
#7744 = CARTESIAN_POINT ( 'NONE',  ( -10.77303304197945621, -12.62668734528506853, 61.09853568451838868 ) ) ;
#7745 = FACE_OUTER_BOUND ( 'NONE', #7240, .T. ) ;
#7746 = CARTESIAN_POINT ( 'NONE',  ( -23.93094852480032486, -11.18081511418321305, 70.01493868496932294 ) ) ;
#7747 = DIRECTION ( 'NONE',  ( 2.866981220435666553E-17, -1.000000000000000000, -1.190614954331866791E-16 ) ) ;
#7748 = CARTESIAN_POINT ( 'NONE',  ( -18.53034385650551741, -9.794322478646142471, 51.19202720610083190 ) ) ;
#7749 = EDGE_CURVE ( 'NONE', #35637, #19053, #21941, .T. ) ;
#7750 = ORIENTED_EDGE ( 'NONE', *, *, #32917, .F. ) ;
#7751 = CARTESIAN_POINT ( 'NONE',  ( -17.73316510640421129, -22.25279988176325574, 58.60564575049652802 ) ) ;
#7752 = CARTESIAN_POINT ( 'NONE',  ( -14.41428275390769365, -7.994163218335415877, 63.97474169571218283 ) ) ;
#7753 = ORIENTED_EDGE ( 'NONE', *, *, #42902, .F. ) ;
#7754 = CARTESIAN_POINT ( 'NONE',  ( -24.40658449907487793, -15.78251210865724907, 69.53307488410803217 ) ) ;
#7755 = CARTESIAN_POINT ( 'NONE',  ( -24.47432067347917695, -14.77756146504815327, 59.52828185648635184 ) ) ;
#7756 = ORIENTED_EDGE ( 'NONE', *, *, #13686, .T. ) ;
#7757 = CARTESIAN_POINT ( 'NONE',  ( -23.54928233522715075, -11.31107727082186720, 66.42214407614666527 ) ) ;
#7758 =( BOUNDED_CURVE ( )  B_SPLINE_CURVE ( 3, ( #9366, #20689, #9617, #18178 ),
 .UNSPECIFIED., .F., .F. ) 
 B_SPLINE_CURVE_WITH_KNOTS ( ( 4, 4 ),
 ( 0.9074455897393697290, 1.000000000000000000 ),
 .UNSPECIFIED. ) 
 CURVE ( )  GEOMETRIC_REPRESENTATION_ITEM ( )  RATIONAL_B_SPLINE_CURVE ( ( 0.6983129098260870693, 0.7760317562606930952, 0.8765941196519974055, 1.000000000000000000 ) ) 
 REPRESENTATION_ITEM ( '' )  );
#7759 = CARTESIAN_POINT ( 'NONE',  ( -10.45859239952313224, -15.89938452881993847, 64.79299464097340433 ) ) ;
#7760 = CARTESIAN_POINT ( 'NONE',  ( -18.40708155023567016, -22.19419919850242806, 68.99231578116254582 ) ) ;
#7761 = ORIENTED_EDGE ( 'NONE', *, *, #36544, .F. ) ;
#7762 = CARTESIAN_POINT ( 'NONE',  ( -15.77409385650551954, -9.792211528768504536, 50.49490371617623197 ) ) ;
#7763 = CARTESIAN_POINT ( 'NONE',  ( -11.32522400900782067, -11.27219014254736074, 60.96413645226084554 ) ) ;
#7764 = VECTOR ( 'NONE', #22510, 1000.000000000000000 ) ;
#7765 = DIRECTION ( 'NONE',  ( -0.9562635972186039890, 0.2925062950340274193, -4.666065131241666896E-08 ) ) ;
#7766 = CARTESIAN_POINT ( 'NONE',  ( -17.42409385541299471, -14.80920654474435594, 52.02966884056656482 ) ) ;
#7767 = CARTESIAN_POINT ( 'NONE',  ( -42.16821150247188399, -14.80920654474410547, 65.04705882352939739 ) ) ;
#7768 = VECTOR ( 'NONE', #44543, 1000.000000000000000 ) ;
#7769 = ORIENTED_EDGE ( 'NONE', *, *, #8538, .F. ) ;
#7770 = ORIENTED_EDGE ( 'NONE', *, *, #46963, .T. ) ;
#7771 = CARTESIAN_POINT ( 'NONE',  ( -15.97409385650551705, -9.792211528768504536, 50.49490371617623197 ) ) ;
#7772 = CARTESIAN_POINT ( 'NONE',  ( -20.38226043987465630, -7.971587899251926679, 70.36605015394232510 ) ) ;
#7773 = TOROIDAL_SURFACE ( 'NONE', #26639, 1.750000000000000000, 0.2500000000000000000 ) ;
#7774 = CARTESIAN_POINT ( 'NONE',  ( -16.31159385650551386, -6.922745924619793101, 51.69366785382590024 ) ) ;
#7775 = CARTESIAN_POINT ( 'NONE',  ( -23.14235562961970416, -18.93896739645850502, 59.09230457533665515 ) ) ;
#7776 = EDGE_CURVE ( 'NONE', #16419, #42266, #1118, .T. ) ;
#7777 = CARTESIAN_POINT ( 'NONE',  ( -10.63004074901718532, -12.92571453866564646, 67.75304464120749515 ) ) ;
#7778 = CARTESIAN_POINT ( 'NONE',  ( -18.77740661349481144, -7.941208124173705585, 67.12745024023926987 ) ) ;
#7779 = CARTESIAN_POINT ( 'NONE',  ( -24.38756562526642213, -15.91227465074932290, 66.34852784166324113 ) ) ;
#7780 = EDGE_LOOP ( 'NONE', ( #10691, #32985 ) ) ;
#7781 = CARTESIAN_POINT ( 'NONE',  ( -24.87206580614764206, -14.63538509624143380, 62.86296487661732613 ) ) ;
#7782 = ORIENTED_EDGE ( 'NONE', *, *, #34151, .F. ) ;
#7783 = EDGE_CURVE ( 'NONE', #22618, #8614, #30698, .T. ) ;
#7784 = CARTESIAN_POINT ( 'NONE',  ( -12.58002213166789041, -9.148928514680237711, 74.43427606957253317 ) ) ;
#7785 = CARTESIAN_POINT ( 'NONE',  ( -21.18000576974785787, -20.77541348745421246, 69.35450184739246993 ) ) ;
#7786 = CARTESIAN_POINT ( 'NONE',  ( -12.52062984216016162, -9.200252406392841920, 74.44110225673207992 ) ) ;
#7787 = DIRECTION ( 'NONE',  ( 0.06498076606345293271, 0.4424675129789839567, 0.8944271909999157444 ) ) ;
#7788 = EDGE_CURVE ( 'NONE', #936, #30190, #42976, .T. ) ;
#7789 = ORIENTED_EDGE ( 'NONE', *, *, #28832, .T. ) ;
#7790 = CARTESIAN_POINT ( 'NONE',  ( -10.65715545825994681, -16.81507633650918976, 61.30175972107676330 ) ) ;
#7791 = VECTOR ( 'NONE', #1287, 1000.000000000000000 ) ;
#7792 = CARTESIAN_POINT ( 'NONE',  ( -24.42310453188136776, -14.68514332193893068, 62.71296481370961118 ) ) ;
#7793 = EDGE_CURVE ( 'NONE', #36602, #33816, #5579, .T. ) ;
#7794 = AXIS2_PLACEMENT_3D ( 'NONE', #2048, #24718, #5985 ) ;
#7795 = CARTESIAN_POINT ( 'NONE',  ( -13.11946129443726861, -9.225960368241006293, 67.37942785707224402 ) ) ;
#7796 = CYLINDRICAL_SURFACE ( 'NONE', #10331, 0.1499999999999986067 ) ;
#7797 = VERTEX_POINT ( 'NONE', #20080 ) ;
#7798 = CARTESIAN_POINT ( 'NONE',  ( -22.98834342787593243, -19.14440809158465839, 62.65407131744080260 ) ) ;
#7799 = CARTESIAN_POINT ( 'NONE',  ( -18.17795515447646792, -21.82680332084924046, 72.42944048533317414 ) ) ;
#7800 = AXIS2_PLACEMENT_3D ( 'NONE', #37699, #14302, #48297 ) ;
#7802 = CARTESIAN_POINT ( 'NONE',  ( -10.73717317386910608, -11.52448149694614443, 71.26673621149227245 ) ) ;
#7801 = CIRCLE ( 'NONE', #45552, 4.686499999999998778 ) ;
#7803 = FACE_BOUND ( 'NONE', #14688, .T. ) ;
#7804 = ORIENTED_EDGE ( 'NONE', *, *, #39962, .F. ) ;
#7805 = CARTESIAN_POINT ( 'NONE',  ( -23.83043763270304538, -11.86620476845630279, 59.48235732590899261 ) ) ;
#7806 = CARTESIAN_POINT ( 'NONE',  ( -17.42409385541299471, -14.80920654474435594, 52.02966884056656482 ) ) ;
#7807 = CARTESIAN_POINT ( 'NONE',  ( -23.27284462870851911, -18.74605969774991010, 66.10917289053097079 ) ) ;
#7808 = CARTESIAN_POINT ( 'NONE',  ( -21.31115985637654120, -8.927249709250721921, 73.88656608925673197 ) ) ;
#7809 = ORIENTED_EDGE ( 'NONE', *, *, #35557, .F. ) ;
#7810 = CARTESIAN_POINT ( 'NONE',  ( -10.13258914451759019, -16.33817228489381179, 71.63245656337019796 ) ) ;
#7811 = VECTOR ( 'NONE', #32667, 1000.000000000000000 ) ;
#7812 = ORIENTED_EDGE ( 'NONE', *, *, #47313, .T. ) ;
#7813 = CARTESIAN_POINT ( 'NONE',  ( -19.20714268997449281, -19.15619313305651161, 52.02966884056656482 ) ) ;
#7814 = LINE ( 'NONE', #29963, #38453 ) ;
#7815 = CARTESIAN_POINT ( 'NONE',  ( -14.54391382047218784, -7.937654553327920581, 63.97634087063163122 ) ) ;
#7816 = VERTEX_POINT ( 'NONE', #45726 ) ;
#7817 = CARTESIAN_POINT ( 'NONE',  ( -11.01268028240570551, -17.61879301183672197, 68.28825229171054900 ) ) ;
#7818 = ORIENTED_EDGE ( 'NONE', *, *, #29388, .T. ) ;
#7819 = EDGE_LOOP ( 'NONE', ( #46777, #19152, #4147, #26110, #7538 ) ) ;
#7820 = ORIENTED_EDGE ( 'NONE', *, *, #33523, .F. ) ;
#7821 = FACE_OUTER_BOUND ( 'NONE', #38897, .T. ) ;
#7822 = CARTESIAN_POINT ( 'NONE',  ( -23.88415220289344276, -17.63235127459526908, 62.62360984996717406 ) ) ;
#7823 = CARTESIAN_POINT ( 'NONE',  ( -13.93897074462874919, -20.93787812888889377, 68.74153005185598886 ) ) ;
#7824 = CARTESIAN_POINT ( 'NONE',  ( -10.57110035550071103, -13.38215360593666325, 74.97817647590578360 ) ) ;
#7825 = CARTESIAN_POINT ( 'NONE',  ( -10.38101357771169653, -17.23783955604091034, 61.35081420447383493 ) ) ;
#7826 = CARTESIAN_POINT ( 'NONE',  ( -14.09914643654217947, -8.649277595337252933, 74.49954655170296292 ) ) ;
#7827 = CARTESIAN_POINT ( 'NONE',  ( -19.32724462824635836, -8.072771342010748086, 60.26093028616645597 ) ) ;
#7828 = ORIENTED_EDGE ( 'NONE', *, *, #44217, .T. ) ;
#7829 = ORIENTED_EDGE ( 'NONE', *, *, #21502, .T. ) ;
#7830 = CARTESIAN_POINT ( 'NONE',  ( -46.92409385541305511, -17.80920654474410370, 62.75000000000000000 ) ) ;
#7831 = CARTESIAN_POINT ( 'NONE',  ( 22.62590614458706639, 1.890747609047612077, 50.53028072113853142 ) ) ;
#7832 = DIRECTION ( 'NONE',  ( 0.3109111061729914471, 0.9504389954427826526, 3.354176643444177759E-08 ) ) ;
#7833 = FACE_OUTER_BOUND ( 'NONE', #15759, .T. ) ;
#7834 = EDGE_LOOP ( 'NONE', ( #23473, #10464, #35662, #36662 ) ) ;
#7835 = EDGE_CURVE ( 'NONE', #10344, #20228, #23299, .T. ) ;
#7836 = CARTESIAN_POINT ( 'NONE',  ( -15.38034385650552061, -6.424090610841176385, 49.80797279389977916 ) ) ;
#7837 = B_SPLINE_CURVE_WITH_KNOTS ( 'NONE', 1,
 ( #20669, #1943 ),
 .UNSPECIFIED., .F., .F.,
 ( 2, 2 ),
 ( 0.000000000000000000, 1.000000000000000000 ),
 .UNSPECIFIED. ) ;
#7838 = VECTOR ( 'NONE', #39698, 1000.000000000000000 ) ;
#7839 = EDGE_LOOP ( 'NONE', ( #27489, #23449, #2237, #42795 ) ) ;
#7840 = CARTESIAN_POINT ( 'NONE',  ( -21.56447292742736721, -9.102906949739807629, 70.13692356594822286 ) ) ;
#7841 = CARTESIAN_POINT ( 'NONE',  ( -10.60570718526854961, -17.81143598018131158, 71.68222757358374508 ) ) ;
#7842 = CYLINDRICAL_SURFACE ( 'NONE', #36995, 0.1500000000000032696 ) ;
#7843 = AXIS2_PLACEMENT_3D ( 'NONE', #45179, #25707, #11417 ) ;
#7844 = ORIENTED_EDGE ( 'NONE', *, *, #38942, .F. ) ;
#7845 = CARTESIAN_POINT ( 'NONE',  ( -20.33883497535441975, -7.953047583504734064, 70.45089127635624493 ) ) ;
#7846 = CARTESIAN_POINT ( 'NONE',  ( -14.66805042590366170, -8.374595077462174686, 60.42882391711909662 ) ) ;
#7847 = DIRECTION ( 'NONE',  ( -3.071710424422018668E-17, 6.404604876783312462E-16, 1.000000000000000000 ) ) ;
#7848 = EDGE_CURVE ( 'NONE', #45644, #39290, #1353, .T. ) ;
#7849 = ORIENTED_EDGE ( 'NONE', *, *, #16016, .T. ) ;
#7850 = CYLINDRICAL_SURFACE ( 'NONE', #11615, 5.249999999999998224 ) ;
#7851 = EDGE_CURVE ( 'NONE', #36492, #43726, #25929, .T. ) ;
#7852 = CARTESIAN_POINT ( 'NONE',  ( -10.12265238338418705, -16.28962619459307604, 71.54776144607544097 ) ) ;
#7853 = CARTESIAN_POINT ( 'NONE',  ( -50.42609385541305755, -14.80920654474411613, 58.00588235294116402 ) ) ;
#7854 = ORIENTED_EDGE ( 'NONE', *, *, #46240, .F. ) ;
#7855 = CARTESIAN_POINT ( 'NONE',  ( -10.51016334156404319, -15.90393143234257067, 64.79306193244994461 ) ) ;
#7856 = ORIENTED_EDGE ( 'NONE', *, *, #18122, .T. ) ;
#7857 = CARTESIAN_POINT ( 'NONE',  ( -17.26599293058224305, -9.561587646847172550, 52.02966884056656482 ) ) ;
#7858 = CARTESIAN_POINT ( 'NONE',  ( -24.74075702715665770, -16.21285080831185965, 62.77823949964436423 ) ) ;
#7859 = ADVANCED_FACE ( 'NONE', ( #42011 ), #46436, .T. ) ;
#7860 = ORIENTED_EDGE ( 'NONE', *, *, #6734, .T. ) ;
#7861 = DIRECTION ( 'NONE',  ( -3.071710424422018668E-17, 6.404604876783312462E-16, 1.000000000000000000 ) ) ;
#7862 = FACE_OUTER_BOUND ( 'NONE', #28431, .T. ) ;
#7863 = CARTESIAN_POINT ( 'NONE',  ( -12.57192052008188199, -9.689650089559323831, 57.18115496948411192 ) ) ;
#7864 = VERTEX_POINT ( 'NONE', #46186 ) ;
#7865 = CARTESIAN_POINT ( 'NONE',  ( -21.38192084656556702, -20.58297848677295150, 72.53948803543819679 ) ) ;
#7866 = EDGE_CURVE ( 'NONE', #47823, #9916, #39282, .T. ) ;
#7867 = FACE_OUTER_BOUND ( 'NONE', #15494, .T. ) ;
#7868 = DIRECTION ( 'NONE',  ( 0.2189141945955470625, -0.9757441136919982050, 0.000000000000000000 ) ) ;
#7869 = ORIENTED_EDGE ( 'NONE', *, *, #48308, .F. ) ;
#7870 = CARTESIAN_POINT ( 'NONE',  ( -24.72694767484942702, -16.28301260341204326, 62.70833288210281609 ) ) ;
#7871 = CARTESIAN_POINT ( 'NONE',  ( -23.30443023073026509, -19.38357886444350342, 59.07748956515449379 ) ) ;
#7872 = EDGE_LOOP ( 'NONE', ( #38232, #31545, #46045, #25751 ) ) ;
#7873 = ORIENTED_EDGE ( 'NONE', *, *, #15376, .T. ) ;
#7874 = PLANE ( 'NONE',  #8681 ) ;
#7875 = CARTESIAN_POINT ( 'NONE',  ( -10.69992486892027372, -11.60142258341215360, 71.21048119115297936 ) ) ;
#7876 = CARTESIAN_POINT ( 'NONE',  ( -21.01334446694451685, -11.79580940901521835, 49.52966884056655772 ) ) ;
#7877 = ORIENTED_EDGE ( 'NONE', *, *, #36498, .T. ) ;
#7878 = VECTOR ( 'NONE', #23107, 1000.000000000000000 ) ;
#7879 = CARTESIAN_POINT ( 'NONE',  ( -22.46784385650551741, -6.428312510596450480, 51.20221977374900035 ) ) ;
#7880 = CARTESIAN_POINT ( 'NONE',  ( -20.31796842471441522, -7.944138697998205600, 70.29454436300783016 ) ) ;
#7881 =( BOUNDED_CURVE ( )  B_SPLINE_CURVE ( 3, ( #18699, #38143, #37155, #30791 ),
 .UNSPECIFIED., .F., .F. ) 
 B_SPLINE_CURVE_WITH_KNOTS ( ( 4, 4 ),
 ( 0.5000000000000000000, 0.9074455897393671755 ),
 .UNSPECIFIED. ) 
 CURVE ( )  GEOMETRIC_REPRESENTATION_ITEM ( )  RATIONAL_B_SPLINE_CURVE ( ( 0.9999999999999786837, 0.4567392136813255288, 0.3561768502900427014, 0.6983129098261070533 ) ) 
 REPRESENTATION_ITEM ( '' )  );
#7882 = CARTESIAN_POINT ( 'NONE',  ( -11.55573855159262386, -10.21941529800896653, 71.15388400389697665 ) ) ;
#7883 = DIRECTION ( 'NONE',  ( 0.8083598999316397027, 0.5886886037477749856, 6.671815825018552065E-08 ) ) ;
#7884 = CARTESIAN_POINT ( 'NONE',  ( -10.51729421260818498, -16.22293138110306998, 71.44750383217574097 ) ) ;
#7885 = ORIENTED_EDGE ( 'NONE', *, *, #44578, .F. ) ;
#7886 = CARTESIAN_POINT ( 'NONE',  ( -12.52591642561268515, -9.195683996340104471, 74.50418400381258266 ) ) ;
#7887 = FACE_OUTER_BOUND ( 'NONE', #44704, .T. ) ;
#7888 = CARTESIAN_POINT ( 'NONE',  ( -15.03427660820159772, -21.44211488324610571, 65.12068745241758450 ) ) ;
#7889 = EDGE_CURVE ( 'NONE', #25586, #22230, #27710, .T. ) ;
#7890 =( BOUNDED_CURVE ( )  B_SPLINE_CURVE ( 2, ( #3976, #18731, #33742, #38, #18990, #33992, #291, #26624, #15269 ),
 .UNSPECIFIED., .F., .F. ) 
 B_SPLINE_CURVE_WITH_KNOTS ( ( 3, 2, 2, 2, 3 ),
 ( 0.007868113086928890665, 0.008851720571105191337, 0.009835328055281493745, 0.01081893553945779268, 0.01180254302363409509 ),
 .UNSPECIFIED. ) 
 CURVE ( )  GEOMETRIC_REPRESENTATION_ITEM ( )  RATIONAL_B_SPLINE_CURVE ( ( 0.9999999999977363663, 0.9238795325135503722, 1.000000000000000000, 0.9238795325112867385, 1.000000000000000000, 0.9238795325112867385, 1.000000000000000000, 0.9238795325108279943, 1.000000000000458744 ) ) 
 REPRESENTATION_ITEM ( '' )  );
#7891 = ORIENTED_EDGE ( 'NONE', *, *, #42221, .F. ) ;
#7892 = ORIENTED_EDGE ( 'NONE', *, *, #698, .T. ) ;
#7893 = LINE ( 'NONE', #3945, #42204 ) ;
#7894 =( NAMED_UNIT ( * ) SI_UNIT ( $, .STERADIAN. ) SOLID_ANGLE_UNIT ( ) );
#7895 = VECTOR ( 'NONE', #6673, 1000.000000000000000 ) ;
#7896 = DIRECTION ( 'NONE',  ( -7.130145686836404013E-06, 1.088473443322539125E-05, 0.9999999999153418306 ) ) ;
#7897 = DIRECTION ( 'NONE',  ( -3.071710424422018668E-17, 6.404604876783312462E-16, 1.000000000000000000 ) ) ;
#7898 = AXIS2_PLACEMENT_3D ( 'NONE', #30135, #10676, #22002 ) ;
#7899 = ORIENTED_EDGE ( 'NONE', *, *, #41754, .F. ) ;
#7900 = ADVANCED_FACE ( 'NONE', ( #42254 ), #11978, .F. ) ;
#7901 = CIRCLE ( 'NONE', #11043, 2.000000000000001332 ) ;
#7902 = DIRECTION ( 'NONE',  ( 0.8565259173193583431, -0.5161040137028850561, 6.301967848571307172E-08 ) ) ;
#7903 =( BOUNDED_CURVE ( )  B_SPLINE_CURVE ( 3, ( #48675, #14921, #11259, #41289 ),
 .UNSPECIFIED., .F., .F. ) 
 B_SPLINE_CURVE_WITH_KNOTS ( ( 4, 4 ),
 ( 0.4074455897393655657, 0.5000000000000000000 ),
 .UNSPECIFIED. ) 
 CURVE ( )  GEOMETRIC_REPRESENTATION_ITEM ( )  RATIONAL_B_SPLINE_CURVE ( ( 0.6983129098261043888, 0.7760317562606969810, 0.8765941196519924095, 0.9999999999999825695 ) ) 
 REPRESENTATION_ITEM ( '' )  );
#7904 = DIRECTION ( 'NONE',  ( -0.6607190350374019250, -0.7506333037770469563, 0.000000000000000000 ) ) ;
#7905 = EDGE_LOOP ( 'NONE', ( #19932, #19808, #19258, #1310, #32469 ) ) ;
#7906 = EDGE_CURVE ( 'NONE', #30992, #16763, #25682, .T. ) ;
#7907 = CARTESIAN_POINT ( 'NONE',  ( -20.85096102773972504, -21.42427126083335764, 58.79475164009666344 ) ) ;
#7908 = AXIS2_PLACEMENT_3D ( 'NONE', #41080, #7113, #41315 ) ;
#7909 = DIRECTION ( 'NONE',  ( -3.549360974551883545E-17, 6.371834667872732552E-18, 1.000000000000000000 ) ) ;
#7910 = CARTESIAN_POINT ( 'NONE',  ( -10.86812120810698801, -17.26293121805600705, 64.92739382021848371 ) ) ;
#7911 = EDGE_LOOP ( 'NONE', ( #33232, #9591, #12350, #47101 ) ) ;
#7912 = CARTESIAN_POINT ( 'NONE',  ( -11.56806251476610115, -18.73522173559940995, 65.03234934376791898 ) ) ;
#7913 = ORIENTED_EDGE ( 'NONE', *, *, #34422, .T. ) ;
#7914 = CARTESIAN_POINT ( 'NONE',  ( -17.21159385759798965, -8.990409506049200417, 49.61344411288074951 ) ) ;
#7915 = EDGE_CURVE ( 'NONE', #15477, #39727, #23833, .T. ) ;
#7916 = CARTESIAN_POINT ( 'NONE',  ( -11.10300763040008398, -10.86615618544839457, 57.39398486019972268 ) ) ;
#7917 = ORIENTED_EDGE ( 'NONE', *, *, #42007, .F. ) ;
#7918 = CARTESIAN_POINT ( 'NONE',  ( -17.42409385541299471, -14.80920654474435594, 52.02966884056656482 ) ) ;
#7919 = CARTESIAN_POINT ( 'NONE',  ( -10.40852245472632198, -14.07667478671615591, 64.68803976623010499 ) ) ;
#7920 = CARTESIAN_POINT ( 'NONE',  ( -22.44284385650551528, -8.811426318492348031, 52.18089403414751359 ) ) ;
#7921 = CYLINDRICAL_SURFACE ( 'NONE', #5576, 0.1499999999999987454 ) ;
#7922 = EDGE_CURVE ( 'NONE', #23869, #30431, #3864, .T. ) ;
#7923 = DIRECTION ( 'NONE',  ( -3.071710424422018668E-17, 6.404604876783312462E-16, 1.000000000000000000 ) ) ;
#7924 = CARTESIAN_POINT ( 'NONE',  ( -23.00442008925061188, -19.11762375203660724, 59.18410642057862248 ) ) ;
#7925 = LINE ( 'NONE', #764, #30606 ) ;
#7926 = ORIENTED_EDGE ( 'NONE', *, *, #7587, .F. ) ;
#7927 = CARTESIAN_POINT ( 'NONE',  ( -23.89200480383413350, -11.11192299349349533, 70.07706151945906470 ) ) ;
#7928 = FACE_OUTER_BOUND ( 'NONE', #16263, .T. ) ;
#7929 = CARTESIAN_POINT ( 'NONE',  ( -22.34687024958758172, -20.40107231831204970, 62.33464913462860579 ) ) ;
#7930 = CARTESIAN_POINT ( 'NONE',  ( -7.424093855413048892, -27.10920654474410796, 56.99999999999997868 ) ) ;
#7931 = PLANE ( 'NONE',  #18487 ) ;
#7932 = EDGE_LOOP ( 'NONE', ( #1770, #41077, #44996, #9290, #13060 ) ) ;
#7933 = ORIENTED_EDGE ( 'NONE', *, *, #17579, .F. ) ;
#7934 = VECTOR ( 'NONE', #3098, 1000.000000000000000 ) ;
#7935 = CARTESIAN_POINT ( 'NONE',  ( -18.49053343615340239, -7.435173160506244550, 73.95409006490955051 ) ) ;
#7936 = FACE_OUTER_BOUND ( 'NONE', #15900, .T. ) ;
#7937 = ORIENTED_EDGE ( 'NONE', *, *, #14758, .F. ) ;
#7938 = CARTESIAN_POINT ( 'NONE',  ( -17.00708550189658652, -7.821638742870105965, 73.96018273346899718 ) ) ;
#7939 = CARTESIAN_POINT ( 'NONE',  ( -16.37589109965827561, -22.18522525038468984, 61.93284991378958892 ) ) ;
#7940 = CARTESIAN_POINT ( 'NONE',  ( -21.88034385759799250, -9.360768649639302552, 51.01397948905921709 ) ) ;
#7941 = CARTESIAN_POINT ( 'NONE',  ( -10.46772245883852115, -15.58952514204506556, 57.75896008322165187 ) ) ;
#7942 = ADVANCED_FACE ( 'NONE', ( #25236 ), #21305, .F. ) ;
#7943 = DIRECTION ( 'NONE',  ( -0.8875028193683940358, -0.4608022847308269609, 4.020963237607658939E-08 ) ) ;
#7944 = DIRECTION ( 'NONE',  ( -3.071710424422018668E-17, 6.404604876783312462E-16, 1.000000000000000000 ) ) ;
#7945 = AXIS2_PLACEMENT_3D ( 'NONE', #2836, #2609, #47435 ) ;
#7946 = ADVANCED_FACE ( 'NONE', ( #2808 ), #32386, .T. ) ;
#7947 = DIRECTION ( 'NONE',  ( 1.000000000000000000, 2.866981220435666553E-17, 0.000000000000000000 ) ) ;
#7948 = PRODUCT_DEFINITION_SHAPE ( 'NONE', 'NONE',  #9035 ) ;
#7949 = DIRECTION ( 'NONE',  ( -3.071710424422018668E-17, 6.404604876783312462E-16, 1.000000000000000000 ) ) ;
#7950 = ADVANCED_FACE ( 'NONE', ( #28679 ), #11894, .T. ) ;
#7951 = CARTESIAN_POINT ( 'NONE',  ( -14.42683414290149813, -8.428067600363897682, 67.25975083869262505 ) ) ;
#7952 = AXIS2_PLACEMENT_3D ( 'NONE', #23817, #24547, #38818 ) ;
#7953 = CARTESIAN_POINT ( 'NONE',  ( -42.30718209070717961, -14.90920654474416907, 63.93529411764704662 ) ) ;
#7954 = DIRECTION ( 'NONE',  ( 0.3964226963016397320, 0.9180681052388968144, 0.000000000000000000 ) ) ;
#7955 = CARTESIAN_POINT ( 'NONE',  ( -24.61562913124599916, -12.86357381044341430, 66.55892682786348757 ) ) ;
#7956 = DIRECTION ( 'NONE',  ( 0.000000000000000000, 0.007114381193220324640, -0.9999746924698832418 ) ) ;
#7957 = VERTEX_POINT ( 'NONE', #32839 ) ;
#7958 = ORIENTED_EDGE ( 'NONE', *, *, #10371, .F. ) ;
#7959 = CARTESIAN_POINT ( 'NONE',  ( -14.87409385541304019, -6.859212275519751323, 50.50378509014259265 ) ) ;
#7960 = ORIENTED_EDGE ( 'NONE', *, *, #30922, .F. ) ;
#7961 = CARTESIAN_POINT ( 'NONE',  ( -11.49688049385021138, -18.62690763749001732, 64.76179218520604763 ) ) ;
#7962 = CARTESIAN_POINT ( 'NONE',  ( -21.86436131997776755, -11.54087357708903916, 53.69233794759168887 ) ) ;
#7963 = AXIS2_PLACEMENT_3D ( 'NONE', #40098, #43317, #20659 ) ;
#7964 = B_SPLINE_CURVE_WITH_KNOTS ( 'NONE', 1,
 ( #43056, #31490 ),
 .UNSPECIFIED., .F., .F.,
 ( 2, 2 ),
 ( 0.000000000000000000, 1.000000000000000000 ),
 .UNSPECIFIED. ) ;
#7965 = CARTESIAN_POINT ( 'NONE',  ( -13.70631952225474137, -20.74045397679160629, 65.28628931288089632 ) ) ;
#7966 = CARTESIAN_POINT ( 'NONE',  ( -17.77754172124238963, -7.367517167730140315, 60.12414849856542531 ) ) ;
#7967 = ORIENTED_EDGE ( 'NONE', *, *, #150, .F. ) ;
#7968 = B_SPLINE_CURVE_WITH_KNOTS ( 'NONE', 1,
 ( #38864, #46974 ),
 .UNSPECIFIED., .F., .F.,
 ( 2, 2 ),
 ( 0.000000000000000000, 1.000000000000000000 ),
 .UNSPECIFIED. ) ;
#7969 = AXIS2_PLACEMENT_3D ( 'NONE', #21647, #25106, #40126 ) ;
#7970 = CARTESIAN_POINT ( 'NONE',  ( -16.02724774380223849, -7.491242405164911133, 63.78515641179975404 ) ) ;
#7971 = DIRECTION ( 'NONE',  ( -0.6607190350374019250, -0.7506333037770469563, 0.000000000000000000 ) ) ;
#7972 = VERTEX_POINT ( 'NONE', #47877 ) ;
#7973 = CARTESIAN_POINT ( 'NONE',  ( -18.84284385759798752, -7.587656875400192291, 49.25157356644813689 ) ) ;
#7974 = AXIS2_PLACEMENT_3D ( 'NONE', #6368, #6847, #48206 ) ;
#7975 = CARTESIAN_POINT ( 'NONE',  ( -14.73375560093340120, -21.75656996136207866, 61.75105004614717785 ) ) ;
#7976 = VERTEX_POINT ( 'NONE', #31892 ) ;
#7977 = CARTESIAN_POINT ( 'NONE',  ( -8.424093855413067544, -8.109206544744111511, 50.49999999999999289 ) ) ;
#7978 = CARTESIAN_POINT ( 'NONE',  ( -15.11475081961187428, -8.199755259496424031, 57.07829799881444899 ) ) ;
#7979 = ADVANCED_FACE ( 'NONE', ( #20811 ), #10221, .T. ) ;
#7980 = CARTESIAN_POINT ( 'NONE',  ( -14.82422806554511929, -10.90997840001177721, 49.52966884056655772 ) ) ;
#7981 = VERTEX_POINT ( 'NONE', #17583 ) ;
#7982 = CARTESIAN_POINT ( 'NONE',  ( -10.92750425249182022, -11.16255029878774252, 64.26386639478288032 ) ) ;
#7983 = CARTESIAN_POINT ( 'NONE',  ( 18.57590614458695200, 0.6315104036983664182, 50.27646649643033783 ) ) ;
#7984 = CIRCLE ( 'NONE', #41002, 0.3999999999999975797 ) ;
#7985 = CARTESIAN_POINT ( 'NONE',  ( -16.15549277074025980, -7.924674425949475243, 63.68627727349057466 ) ) ;
#7986 = CARTESIAN_POINT ( 'NONE',  ( -24.12651600458584511, -12.62191667979047160, 73.25697658996381278 ) ) ;
#7987 = ORIENTED_EDGE ( 'NONE', *, *, #43381, .F. ) ;
#7989 = LINE ( 'NONE', #34050, #19382 ) ;
#7988 = B_SPLINE_CURVE_WITH_KNOTS ( 'NONE', 3,
 ( #1865, #36068, #47651, #32156, #10236, #21066, #6536, #13165, #28214, #42988 ),
 .UNSPECIFIED., .F., .F.,
 ( 4, 2, 2, 2, 4 ),
 ( 0.000000000000000000, 0.2500000000000000000, 0.5000000000000000000, 0.7500000000000000000, 1.000000000000000000 ),
 .UNSPECIFIED. ) ;
#7990 = CARTESIAN_POINT ( 'NONE',  ( -17.42409385541299471, -14.80920654474435771, 49.52966884056655772 ) ) ;
#7991 = CARTESIAN_POINT ( 'NONE',  ( -20.52841364755139963, -8.479414496750122154, 63.61121502499755564 ) ) ;
#7992 = CARTESIAN_POINT ( 'NONE',  ( -20.81696265954430558, -20.93198702957875668, 62.11471400680572685 ) ) ;
#7993 = CARTESIAN_POINT ( 'NONE',  ( -10.48723278405693016, -15.75052974003975770, 64.79155073336579562 ) ) ;
#7994 = CARTESIAN_POINT ( 'NONE',  ( -21.62409385650551741, -6.426201560718812544, 50.50509628382439331 ) ) ;
#7995 = CIRCLE ( 'NONE', #4812, 1.999999999999999778 ) ;
#7996 = ORIENTED_EDGE ( 'NONE', *, *, #32974, .F. ) ;
#7997 = LINE ( 'NONE', #37502, #12529 ) ;
#7998 = FACE_OUTER_BOUND ( 'NONE', #42012, .T. ) ;
#7999 = EDGE_LOOP ( 'NONE', ( #11041, #7366, #48156, #45765 ) ) ;
#8000 = CARTESIAN_POINT ( 'NONE',  ( -10.45256745270239307, -15.43993597667916795, 57.86792809192976961 ) ) ;
#8001 = CARTESIAN_POINT ( 'NONE',  ( -22.56581679224888504, -9.985589735435180359, 73.48720857917361116 ) ) ;
#8002 = CARTESIAN_POINT ( 'NONE',  ( -10.81170448216924740, -12.36318809540519048, 57.34329390664808557 ) ) ;
#8003 = ORIENTED_EDGE ( 'NONE', *, *, #22600, .F. ) ;
#8004 = CARTESIAN_POINT ( 'NONE',  ( -14.74510888451587753, -8.287885092648833663, 60.61436521918190579 ) ) ;
#8005 = EDGE_CURVE ( 'NONE', #48120, #46547, #29870, .T. ) ;
#8006 = DIRECTION ( 'NONE',  ( -0.3374354101627465297, -0.9413486835218387583, -1.423378189644413276E-08 ) ) ;
#8007 = AXIS2_PLACEMENT_3D ( 'NONE', #15121, #42219, #18834 ) ;
#8008 = CARTESIAN_POINT ( 'NONE',  ( -18.32857646159318676, -22.20418385865972155, 68.93019298464047040 ) ) ;
#8009 = EDGE_CURVE ( 'NONE', #4181, #48314, #47159, .T. ) ;
#8010 = EDGE_CURVE ( 'NONE', #32569, #21373, #47026, .T. ) ;
#8011 = ORIENTED_EDGE ( 'NONE', *, *, #16142, .T. ) ;
#8012 = CARTESIAN_POINT ( 'NONE',  ( -14.87409385650551741, -9.792211528768504536, 50.49490371617623197 ) ) ;
#8013 = VECTOR ( 'NONE', #12048, 1000.000000000000114 ) ;
#8014 = DIRECTION ( 'NONE',  ( 3.071710424422018668E-17, -6.404604876783312462E-16, -1.000000000000000000 ) ) ;
#8015 = CARTESIAN_POINT ( 'NONE',  ( -24.82475127085388422, -15.66597259679895693, 73.11808347143848152 ) ) ;
#8016 = CARTESIAN_POINT ( 'NONE',  ( -14.03189736672541166, -8.176154092714252641, 70.90674531289162985 ) ) ;
#8017 = CARTESIAN_POINT ( 'NONE',  ( -13.50459945683549279, -9.009416567501544293, 57.07853663195904659 ) ) ;
#8018 = ORIENTED_EDGE ( 'NONE', *, *, #37471, .F. ) ;
#8019 = ORIENTED_EDGE ( 'NONE', *, *, #47262, .T. ) ;
#8020 = CARTESIAN_POINT ( 'NONE',  ( -15.01784385650551457, -9.790100578890868377, 49.79778022625163203 ) ) ;
#8021 = CARTESIAN_POINT ( 'NONE',  ( -12.06140467229625912, -20.05244645202335008, 54.27966884056654351 ) ) ;
#8022 = AXIS2_PLACEMENT_3D ( 'NONE', #35899, #40569, #43806 ) ;
#8023 = CARTESIAN_POINT ( 'NONE',  ( -22.83095840648717711, -19.93459376977450859, 72.82895984417613988 ) ) ;
#8024 =( BOUNDED_SURFACE ( )  B_SPLINE_SURFACE ( 3, 1, ( 
 ( #25423, #36962 ),
 ( #25186, #48299 ),
 ( #14062, #29110 ),
 ( #26154, #40205 ),
 ( #29850, #21721 ),
 ( #14534, #40918 ),
 ( #40433, #37446 ) ),
 .UNSPECIFIED., .T., .F., .F. ) 
 B_SPLINE_SURFACE_WITH_KNOTS ( ( 4, 3, 4 ),
 ( 2, 2 ),
 ( 0.000000000000000000, 0.5000000000000000000, 1.000000000000000000 ),
 ( 0.000000000000000000, 1.000000000000000000 ),
 .UNSPECIFIED. ) 
 GEOMETRIC_REPRESENTATION_ITEM ( )  RATIONAL_B_SPLINE_SURFACE ( (
 ( 1.000000000000000000, 1.000000000000000000),
 ( 0.3333333333333335369, 0.3333333333333330373),
 ( 0.3333333333333335369, 0.3333333333333330373),
 ( 1.000000000000000000, 1.000000000000000000),
 ( 0.3333333333333333703, 0.3333333333333333703),
 ( 0.3333333333333333703, 0.3333333333333333703),
 ( 1.000000000000000000, 1.000000000000000000) ) ) 
 REPRESENTATION_ITEM ( '' )  SURFACE ( )  );
#8025 = CARTESIAN_POINT ( 'NONE',  ( -15.58034385650551634, -6.424090610841176385, 49.80797279389977916 ) ) ;
#8026 = B_SPLINE_CURVE_WITH_KNOTS ( 'NONE', 3,
 ( #24593, #44274, #21126, #5865 ),
 .UNSPECIFIED., .F., .F.,
 ( 4, 4 ),
 ( 0.7089964807430767513, 1.000000000000000000 ),
 .UNSPECIFIED. ) ;
#8027 = CARTESIAN_POINT ( 'NONE',  ( -23.04402284766838349, -19.06632961612601918, 59.16938527523783620 ) ) ;
#8028 = EDGE_CURVE ( 'NONE', #6937, #27994, #29165, .T. ) ;
#8029 = PLANE ( 'NONE',  #42715 ) ;
#8030 = AXIS2_PLACEMENT_3D ( 'NONE', #16545, #24918, #31585 ) ;
#8031 = DIRECTION ( 'NONE',  ( 1.000000000000000000, -4.164305804376849172E-17, 1.614929280266638808E-16 ) ) ;
#8032 = CARTESIAN_POINT ( 'NONE',  ( -21.06702863216100496, -20.84540773593990792, 65.86981821684420879 ) ) ;
#8033 = VERTEX_POINT ( 'NONE', #43714 ) ;
#8034 =( BOUNDED_CURVE ( )  B_SPLINE_CURVE ( 3, ( #10874, #18491, #8173, #42637 ),
 .UNSPECIFIED., .F., .F. ) 
 B_SPLINE_CURVE_WITH_KNOTS ( ( 4, 4 ),
 ( 0.5000000000000000000, 0.9074455897393562953 ),
 .UNSPECIFIED. ) 
 CURVE ( )  GEOMETRIC_REPRESENTATION_ITEM ( )  RATIONAL_B_SPLINE_CURVE ( ( 1.000000000000025091, 0.4567392136813530623, 0.3561768502900203859, 0.6983129098260543177 ) ) 
 REPRESENTATION_ITEM ( '' )  );
#8035 = DIRECTION ( 'NONE',  ( -3.413470714839332458E-33, 1.190614954331866791E-16, -1.000000000000000000 ) ) ;
#8036 = ORIENTED_EDGE ( 'NONE', *, *, #43236, .T. ) ;
#8037 = VECTOR ( 'NONE', #47665, 1000.000000000000000 ) ;
#8038 = CARTESIAN_POINT ( 'NONE',  ( -21.83505603848428933, -9.305730678460758298, 59.60682523891489382 ) ) ;
#8039 = CARTESIAN_POINT ( 'NONE',  ( -9.974042462495141592, -14.85071659844522429, 74.95925431899817681 ) ) ;
#8040 = CARTESIAN_POINT ( 'NONE',  ( -18.56294146299573100, -7.902357174719097266, 74.14064450187080979 ) ) ;
#8041 = CARTESIAN_POINT ( 'NONE',  ( -24.72409385541305582, -14.80920654474424225, 70.97647058823527288 ) ) ;
#8042 = VECTOR ( 'NONE', #10955, 1000.000000000000000 ) ;
#8043 = ORIENTED_EDGE ( 'NONE', *, *, #663, .T. ) ;
#8044 = CARTESIAN_POINT ( 'NONE',  ( -50.42609385541305755, -14.90920654474413887, 60.01764705882352047 ) ) ;
#8045 = DIRECTION ( 'NONE',  ( -1.000000000000000000, -1.669677910507523057E-21, -6.493791346278465266E-22 ) ) ;
#8046 = DIRECTION ( 'NONE',  ( -3.071710424422018668E-17, 6.404604876783312462E-16, 1.000000000000000000 ) ) ;
#8047 = ORIENTED_EDGE ( 'NONE', *, *, #19993, .F. ) ;
#8048 = CARTESIAN_POINT ( 'NONE',  ( -4.424093855413056886, -8.109206544744111511, 50.49999999999999289 ) ) ;
#8049 = CARTESIAN_POINT ( 'NONE',  ( -24.72409385541305582, -14.80920654474419962, 66.05294117647058272 ) ) ;
#8051 =( BOUNDED_CURVE ( )  B_SPLINE_CURVE ( 3, ( #20907, #2899, #35664, #17914 ),
 .UNSPECIFIED., .F., .F. ) 
 B_SPLINE_CURVE_WITH_KNOTS ( ( 4, 4 ),
 ( 0.4074455897393648440, 0.5000000000000000000 ),
 .UNSPECIFIED. ) 
 CURVE ( )  GEOMETRIC_REPRESENTATION_ITEM ( )  RATIONAL_B_SPLINE_CURVE ( ( 0.6983129098260953960, 0.7760317562607079722, 0.8765941196520117273, 1.000000000000012212 ) ) 
 REPRESENTATION_ITEM ( '' )  );
#8050 = CARTESIAN_POINT ( 'NONE',  ( -27.42409385541305511, -10.10920654474410618, 63.99999999999998579 ) ) ;
#8052 = FACE_BOUND ( 'NONE', #28784, .T. ) ;
#8053 = APPLICATION_PROTOCOL_DEFINITION ( 'draft international standard', 'automotive_design', 1998, #18033 ) ;
#8054 = ORIENTED_EDGE ( 'NONE', *, *, #4814, .T. ) ;
#8055 = CARTESIAN_POINT ( 'NONE',  ( -50.42409385541305511, -14.80920654474410725, 74.99999999999998579 ) ) ;
#8056 = LINE ( 'NONE', #38053, #36785 ) ;
#8057 = FACE_OUTER_BOUND ( 'NONE', #9022, .T. ) ;
#8058 = ORIENTED_EDGE ( 'NONE', *, *, #28708, .T. ) ;
#8059 = CARTESIAN_POINT ( 'NONE',  ( -13.75179125342063458, -11.87837916245159953, 49.52966884056655772 ) ) ;
#8060 = ORIENTED_EDGE ( 'NONE', *, *, #48452, .F. ) ;
#8061 = CARTESIAN_POINT ( 'NONE',  ( -22.42006521943993391, -9.190894407991624604, 53.76227901944321985 ) ) ;
#8062 = CARTESIAN_POINT ( 'NONE',  ( -22.88419684932020459, -10.42887832691348926, 63.37185995611467604 ) ) ;
#8063 = ORIENTED_EDGE ( 'NONE', *, *, #3961, .F. ) ;
#8064 = CARTESIAN_POINT ( 'NONE',  ( 18.57590614458706924, 0.6315104036983326674, 50.27646649643033783 ) ) ;
#8065 = VERTEX_POINT ( 'NONE', #28454 ) ;
#8066 = ADVANCED_FACE ( 'NONE', ( #9968 ), #9738, .T. ) ;
#8067 = VERTEX_POINT ( 'NONE', #6276 ) ;
#8068 = EDGE_LOOP ( 'NONE', ( #19728, #36979, #41897, #27954, #38695 ) ) ;
#8069 = DIRECTION ( 'NONE',  ( -4.267285103686820140E-17, 1.935130192142698484E-16, 1.000000000000000000 ) ) ;
#8070 = CARTESIAN_POINT ( 'NONE',  ( -20.31413516131974362, -8.378470924821744603, 67.06632013881642251 ) ) ;
#8071 = CARTESIAN_POINT ( 'NONE',  ( -15.74783386771837890, -7.961078896070159061, 70.62461975990308360 ) ) ;
#8072 = PLANE ( 'NONE',  #15313 ) ;
#8073 = CARTESIAN_POINT ( 'NONE',  ( -19.31784385541291016, -6.860780111191745689, 51.02154966934421765 ) ) ;
#8074 = CARTESIAN_POINT ( 'NONE',  ( -10.50811820331624524, -16.17810198025521728, 71.45310207454518547 ) ) ;
#8075 = ORIENTED_EDGE ( 'NONE', *, *, #20174, .T. ) ;
#8076 = ORIENTED_EDGE ( 'NONE', *, *, #11038, .T. ) ;
#8077 = ADVANCED_FACE ( 'NONE', ( #24526 ), #5280, .T. ) ;
#8078 = EDGE_CURVE ( 'NONE', #5029, #21537, #10312, .T. ) ;
#8079 = EDGE_CURVE ( 'NONE', #14112, #6378, #18060, .T. ) ;
#8080 = CARTESIAN_POINT ( 'NONE',  ( -24.84793640206982701, -14.18443463346696909, 69.83770693398628282 ) ) ;
#8081 = CARTESIAN_POINT ( 'NONE',  ( -14.07539642552819359, -8.605278304397881328, 74.19954655214911554 ) ) ;
#8082 = CARTESIAN_POINT ( 'NONE',  ( -23.66133370835450833, -18.88359203746988868, 69.40876704922922613 ) ) ;
#8083 = EDGE_CURVE ( 'NONE', #43727, #25852, #34113, .T. ) ;
#8084 = ORIENTED_EDGE ( 'NONE', *, *, #45828, .F. ) ;
#8085 = CARTESIAN_POINT ( 'NONE',  ( -15.88659385650551670, -9.302874398569244363, 51.68646062012417985 ) ) ;
#8086 = VERTEX_POINT ( 'NONE', #14349 ) ;
#8087 = CARTESIAN_POINT ( 'NONE',  ( -17.75227477277866939, -19.48420168222599713, 52.02966884056656482 ) ) ;
#8088 = EDGE_CURVE ( 'NONE', #34579, #25977, #14720, .T. ) ;
#8089 = CARTESIAN_POINT ( 'NONE',  ( -12.13424045023392139, -19.48172391048287011, 61.54111352175390692 ) ) ;
#8090 = CARTESIAN_POINT ( 'NONE',  ( -4.924093855413050669, -6.359206544744109735, 47.99999999999998579 ) ) ;
#8091 = ORIENTED_EDGE ( 'NONE', *, *, #48520, .F. ) ;
#8092 = CARTESIAN_POINT ( 'NONE',  ( -10.42609550623400416, -14.63933595658813935, 67.93088217856531230 ) ) ;
#8093 = CARTESIAN_POINT ( 'NONE',  ( -22.79669589439772537, -19.97039224088601372, 72.74426291965076530 ) ) ;
#8094 = VERTEX_POINT ( 'NONE', #40723 ) ;
#8095 = CARTESIAN_POINT ( 'NONE',  ( -10.61779597260244401, -12.95740878981562361, 71.50828843252445211 ) ) ;
#8096 = CARTESIAN_POINT ( 'NONE',  ( -24.12651600458584511, -12.62191667979047338, 73.25697658996379857 ) ) ;
#8097 = CARTESIAN_POINT ( 'NONE',  ( -19.33359430827714576, -8.018871227582772931, 63.73089477487069132 ) ) ;
#8098 = ORIENTED_EDGE ( 'NONE', *, *, #16939, .F. ) ;
#8099 = CARTESIAN_POINT ( 'NONE',  ( -16.02724774380223849, -7.491242405164911133, 63.78515641179975404 ) ) ;
#8100 = ORIENTED_EDGE ( 'NONE', *, *, #3638, .T. ) ;
#8101 = CARTESIAN_POINT ( 'NONE',  ( -10.18401476999287425, -13.05278034840643286, 71.32333300961973066 ) ) ;
#8102 = EDGE_LOOP ( 'NONE', ( #37352, #15853, #37088, #36769 ) ) ;
#8103 = CARTESIAN_POINT ( 'NONE',  ( -19.86520892150080897, -18.82374422416847537, 49.52966884056656482 ) ) ;
#8104 = CARTESIAN_POINT ( 'NONE',  ( -10.99582178678916833, -11.91441492378913480, 74.85840195586327184 ) ) ;
#8105 = CARTESIAN_POINT ( 'NONE',  ( -24.23114935566793804, -13.17655915171226866, 63.13264225663914431 ) ) ;
#8106 = ORIENTED_EDGE ( 'NONE', *, *, #6947, .F. ) ;
#8107 = LINE ( 'NONE', #27042, #18950 ) ;
#8108 = EDGE_CURVE ( 'NONE', #27480, #5623, #7997, .T. ) ;
#8109 = FACE_OUTER_BOUND ( 'NONE', #38678, .T. ) ;
#8110 = CARTESIAN_POINT ( 'NONE',  ( -11.43159037681183321, -11.19109104294698298, 57.43576446439195848 ) ) ;
#8111 = ORIENTED_EDGE ( 'NONE', *, *, #29597, .T. ) ;
#8112 = CARTESIAN_POINT ( 'NONE',  ( -12.26841837488882092, -9.996323195260892192, 56.97446934404248964 ) ) ;
#8113 = DIRECTION ( 'NONE',  ( -3.071710424422018668E-17, 6.404604876783312462E-16, 1.000000000000000000 ) ) ;
#8114 = EDGE_CURVE ( 'NONE', #40490, #241, #22766, .T. ) ;
#8115 = ORIENTED_EDGE ( 'NONE', *, *, #4929, .F. ) ;
#8116 = ORIENTED_EDGE ( 'NONE', *, *, #5616, .T. ) ;
#8117 = FACE_OUTER_BOUND ( 'NONE', #19854, .T. ) ;
#8118 = CARTESIAN_POINT ( 'NONE',  ( -10.51737753838112610, -13.38018574993044219, 71.09339731095114701 ) ) ;
#8119 = FACE_OUTER_BOUND ( 'NONE', #9412, .T. ) ;
#8120 =( BOUNDED_CURVE ( )  B_SPLINE_CURVE ( 3, ( #31402, #39028, #30693, #8772 ),
 .UNSPECIFIED., .F., .F. ) 
 B_SPLINE_CURVE_WITH_KNOTS ( ( 4, 4 ),
 ( 0.000000000000000000, 0.4074455897393606807 ),
 .UNSPECIFIED. ) 
 CURVE ( )  GEOMETRIC_REPRESENTATION_ITEM ( )  RATIONAL_B_SPLINE_CURVE ( ( 1.000000000000000000, 0.4567392136813414050, 0.3561768502900338196, 0.6983129098260772993 ) ) 
 REPRESENTATION_ITEM ( '' )  );
#8121 = CARTESIAN_POINT ( 'NONE',  ( -20.66784385650552380, -6.428312510596450480, 51.20221977374900035 ) ) ;
#8122 = CARTESIAN_POINT ( 'NONE',  ( -24.83498170362974022, -14.04605013716215822, 73.37917436033832530 ) ) ;
#8123 = CARTESIAN_POINT ( 'NONE',  ( -15.66732230932660741, -10.46443543628982553, 49.52966884056655772 ) ) ;
#8124 = CARTESIAN_POINT ( 'NONE',  ( -9.975269291463440879, -14.95070888436857715, 74.95812242214459786 ) ) ;
#8125 = ORIENTED_EDGE ( 'NONE', *, *, #34829, .F. ) ;
#8126 = DIRECTION ( 'NONE',  ( 0.4182840851231336421, -0.9083162577718748576, 8.112345261759808545E-09 ) ) ;
#8127 =( LENGTH_UNIT ( ) NAMED_UNIT ( * ) SI_UNIT ( .MILLI., .METRE. ) );
#8128 = AXIS2_PLACEMENT_3D ( 'NONE', #20556, #39735, #35551 ) ;
#8129 = ADVANCED_FACE ( 'NONE', ( #7260 ), #3047, .T. ) ;
#8130 = CARTESIAN_POINT ( 'NONE',  ( -24.53556902878502655, -12.58855298716505366, 69.94959881007889635 ) ) ;
#8131 = FACE_OUTER_BOUND ( 'NONE', #2099, .T. ) ;
#8132 = ADVANCED_FACE ( 'NONE', ( #33817 ), #3540, .F. ) ;
#8133 = ORIENTED_EDGE ( 'NONE', *, *, #2974, .T. ) ;
#8134 = EDGE_CURVE ( 'NONE', #32577, #27062, #31771, .T. ) ;
#8135 = ORIENTED_EDGE ( 'NONE', *, *, #21193, .T. ) ;
#8136 = DIRECTION ( 'NONE',  ( -0.8037372918934695409, 0.5949843406508663612, 7.322964617522835370E-08 ) ) ;
#8137 = CARTESIAN_POINT ( 'NONE',  ( -12.84615363328625648, -20.17103110633857455, 72.09181604382622766 ) ) ;
#8138 = CARTESIAN_POINT ( 'NONE',  ( -21.68042710870613732, -9.185287987594811909, 63.07665001108087921 ) ) ;
#8139 = DIRECTION ( 'NONE',  ( -7.105595949593054157E-06, -6.912614924914188927E-07, 0.9999999999745162738 ) ) ;
#8140 = ADVANCED_FACE ( 'NONE', ( #30153 ), #33571, .T. ) ;
#8141 = ORIENTED_EDGE ( 'NONE', *, *, #45192, .T. ) ;
#8142 = CARTESIAN_POINT ( 'NONE',  ( -20.84119746710918974, -20.97572115929791892, 62.11471400470772863 ) ) ;
#8143 = CARTESIAN_POINT ( 'NONE',  ( -23.10710312199593730, -6.455677289120571594, 54.49999999999995026 ) ) ;
#8144 = PRODUCT_RELATED_PRODUCT_CATEGORY ( 'part', '', ( #46082 ) ) ;
#8145 = EDGE_LOOP ( 'NONE', ( #5454, #26803, #45626, #26115, #3120 ) ) ;
#8146 = B_SPLINE_CURVE_WITH_KNOTS ( 'NONE', 3,
 ( #42718, #6253, #12898, #28421, #43446, #9715, #42947, #20300, #8981, #47382 ),
 .UNSPECIFIED., .F., .F.,
 ( 4, 2, 2, 2, 4 ),
 ( 0.000000000000000000, 0.2500000000000000000, 0.5000000000000000000, 0.7500000000000000000, 1.000000000000000000 ),
 .UNSPECIFIED. ) ;
#8147 = DIRECTION ( 'NONE',  ( -0.3996021513128670266, -0.9166886716143755054, -9.834836654444679756E-09 ) ) ;
#8148 = CARTESIAN_POINT ( 'NONE',  ( -13.91545454884148825, -8.237059506355153715, 74.45600559034086530 ) ) ;
#8149 = ORIENTED_EDGE ( 'NONE', *, *, #48262, .F. ) ;
#8150 = CARTESIAN_POINT ( 'NONE',  ( -24.72409385541305582, -14.80920654474415699, 62.02941176470587692 ) ) ;
#8151 = VERTEX_POINT ( 'NONE', #45410 ) ;
#8152 = DIRECTION ( 'NONE',  ( 0.7224352045700188629, 0.6914386272098739239, -9.340627245513718311E-09 ) ) ;
#8153 = DIRECTION ( 'NONE',  ( -0.9660698163281072892, -0.2582810677919976650, 5.363434502754641456E-08 ) ) ;
#8154 = ORIENTED_EDGE ( 'NONE', *, *, #18400, .T. ) ;
#8155 = CARTESIAN_POINT ( 'NONE',  ( -24.42850061278427987, -15.61005279108867860, 73.00303770028719441 ) ) ;
#8156 = FACE_OUTER_BOUND ( 'NONE', #22384, .T. ) ;
#8157 = AXIS2_PLACEMENT_3D ( 'NONE', #24683, #39688, #31333 ) ;
#8158 = CARTESIAN_POINT ( 'NONE',  ( -16.19909385650551670, -8.114302828567740988, 52.18300498402516041 ) ) ;
#8159 = CARTESIAN_POINT ( 'NONE',  ( -17.64597121246115563, -21.80612736696262033, 58.42169971083756508 ) ) ;
#8160 =( BOUNDED_SURFACE ( )  B_SPLINE_SURFACE ( 3, 1, ( 
 ( #4987, #20001 ),
 ( #6437, #25861 ),
 ( #18458, #36439 ),
 ( #2956, #32526 ),
 ( #22178, #25613 ),
 ( #29553, #2491 ),
 ( #21686, #10604 ) ),
 .UNSPECIFIED., .T., .F., .F. ) 
 B_SPLINE_SURFACE_WITH_KNOTS ( ( 4, 3, 4 ),
 ( 2, 2 ),
 ( 0.000000000000000000, 0.5000000000000000000, 1.000000000000000000 ),
 ( 0.000000000000000000, 1.000000000000000000 ),
 .UNSPECIFIED. ) 
 GEOMETRIC_REPRESENTATION_ITEM ( )  RATIONAL_B_SPLINE_SURFACE ( (
 ( 1.000000000000000000, 1.000000000000000000),
 ( 0.3333333333333335369, 0.3333333333333330373),
 ( 0.3333333333333335369, 0.3333333333333330373),
 ( 1.000000000000000000, 1.000000000000000000),
 ( 0.3333333333333333703, 0.3333333333333333703),
 ( 0.3333333333333333703, 0.3333333333333333703),
 ( 1.000000000000000000, 1.000000000000000000) ) ) 
 REPRESENTATION_ITEM ( '' )  SURFACE ( )  );
#8161 = EDGE_CURVE ( 'NONE', #8614, #38441, #11666, .T. ) ;
#8162 = CARTESIAN_POINT ( 'NONE',  ( -19.17437844398820346, -7.979623566120205957, 63.44561363416070776 ) ) ;
#8163 = CARTESIAN_POINT ( 'NONE',  ( -22.28468842640967651, -19.91619389767071269, 65.98949666203347419 ) ) ;
#8164 = ORIENTED_EDGE ( 'NONE', *, *, #27077, .T. ) ;
#8165 = DIRECTION ( 'NONE',  ( 0.1648596854219665508, 0.9863170302304251624, -7.074492695212681195E-08 ) ) ;
#8166 = LINE ( 'NONE', #7432, #34517 ) ;
#8167 = CARTESIAN_POINT ( 'NONE',  ( -21.34628024798174550, -12.22231469401973847, 49.52966884056655772 ) ) ;
#8168 = CARTESIAN_POINT ( 'NONE',  ( -18.56951349870198342, -7.903555673074887267, 70.56171098378509043 ) ) ;
#8169 = CARTESIAN_POINT ( 'NONE',  ( -22.78971111612053946, -9.640535285194584247, 73.64194477181111154 ) ) ;
#8170 = ORIENTED_EDGE ( 'NONE', *, *, #29630, .T. ) ;
#8171 = VERTEX_POINT ( 'NONE', #27172 ) ;
#8172 = CARTESIAN_POINT ( 'NONE',  ( -16.78411710364782650, -21.83009890335197767, 68.99560651669348488 ) ) ;
#8173 = CARTESIAN_POINT ( 'NONE',  ( -17.69371375962564841, -21.85776310150506774, 62.17535971309806087 ) ) ;
#8174 = VERTEX_POINT ( 'NONE', #35274 ) ;
#8175 = CARTESIAN_POINT ( 'NONE',  ( -24.03794055889475345, -17.10236460774399703, 72.88336037747278340 ) ) ;
#8176 = CARTESIAN_POINT ( 'NONE',  ( -16.34521610185216645, -22.18068367542918651, 61.85544494263961468 ) ) ;
#8177 = CARTESIAN_POINT ( 'NONE',  ( -21.48659385759799179, -7.222650657624104298, 49.61879703869476543 ) ) ;
#8178 = DIRECTION ( 'NONE',  ( 0.000000000000000000, 0.000000000000000000, 1.000000000000000000 ) ) ;
#8179 = CARTESIAN_POINT ( 'NONE',  ( -24.39996002416654264, -14.20937999902714743, 73.31198592523365676 ) ) ;
#8180 = CARTESIAN_POINT ( 'NONE',  ( -10.76351158211370240, -11.46999907741044034, 67.73209273364366823 ) ) ;
#8181 =( BOUNDED_CURVE ( )  B_SPLINE_CURVE ( 3, ( #48526, #14044, #7430, #10863 ),
 .UNSPECIFIED., .F., .F. ) 
 B_SPLINE_CURVE_WITH_KNOTS ( ( 4, 4 ),
 ( 0.9074455897393653991, 1.000000000000000000 ),
 .UNSPECIFIED. ) 
 CURVE ( )  GEOMETRIC_REPRESENTATION_ITEM ( )  RATIONAL_B_SPLINE_CURVE ( ( 0.6983129098260947298, 0.7760317562606996455, 0.8765941196520014023, 1.000000000000000000 ) ) 
 REPRESENTATION_ITEM ( '' )  );
#8182 = CARTESIAN_POINT ( 'NONE',  ( -16.34629159056375514, -21.77648264143983781, 61.76127952027446355 ) ) ;
#8183 = VERTEX_POINT ( 'NONE', #26936 ) ;
#8184 = PLANE ( 'NONE',  #43819 ) ;
#8185 = CARTESIAN_POINT ( 'NONE',  ( -14.46825175861997437, -8.408613495736075194, 67.26534847800355976 ) ) ;
#8186 = EDGE_CURVE ( 'NONE', #47879, #1165, #6849, .T. ) ;
#8187 = CARTESIAN_POINT ( 'NONE',  ( -19.58764298555839289, -21.52291637062162621, 69.23482530291350656 ) ) ;
#8188 = CARTESIAN_POINT ( 'NONE',  ( -17.63137588941029676, -7.812166007189589756, 63.55057029281473291 ) ) ;
#8189 = CARTESIAN_POINT ( 'NONE',  ( -12.71689659754714441, -19.99233245408618487, 71.99580697112106975 ) ) ;
#8190 = EDGE_CURVE ( 'NONE', #32458, #47056, #35029, .T. ) ;
#8191 = VERTEX_POINT ( 'NONE', #1549 ) ;
#8192 = ORIENTED_EDGE ( 'NONE', *, *, #20460, .F. ) ;
#8193 = CARTESIAN_POINT ( 'NONE',  ( -22.29909385650551812, -8.114302828567740988, 52.18300498402516041 ) ) ;
#8194 = ADVANCED_FACE ( 'NONE', ( #23740 ), #46624, .F. ) ;
#8195 = ORIENTED_EDGE ( 'NONE', *, *, #29857, .T. ) ;
#8196 = FACE_OUTER_BOUND ( 'NONE', #28768, .T. ) ;
#8197 = VECTOR ( 'NONE', #42374, 1000.000000000000000 ) ;
#8198 = CARTESIAN_POINT ( 'NONE',  ( -10.42302287260171312, -13.97751933429587012, 57.73352905910142852 ) ) ;
#8199 = EDGE_CURVE ( 'NONE', #2092, #11637, #45666, .T. ) ;
#8200 = CARTESIAN_POINT ( 'NONE',  ( -17.42409385541300892, -14.80920654474439679, 56.49999999999994316 ) ) ;
#8201 = ORIENTED_EDGE ( 'NONE', *, *, #44885, .F. ) ;
#8202 = CARTESIAN_POINT ( 'NONE',  ( -14.11063322135152909, -21.03236308526469855, 72.21135587486895702 ) ) ;
#8203 = CARTESIAN_POINT ( 'NONE',  ( -10.68602809008750576, -16.88409676349039046, 57.70232650191087487 ) ) ;
#8204 = EDGE_LOOP ( 'NONE', ( #2819, #45737 ) ) ;
#8205 = CARTESIAN_POINT ( 'NONE',  ( 10.57590614458695377, 0.6652513346184687482, 50.77657095919170871 ) ) ;
#8206 = EDGE_CURVE ( 'NONE', #44919, #29409, #33884, .T. ) ;
#8207 = DIRECTION ( 'NONE',  ( 0.2737502900231349456, 0.9618007999124593699, -5.400150802740512045E-08 ) ) ;
#8208 = EDGE_CURVE ( 'NONE', #1942, #1265, #47163, .T. ) ;
#8209 = EDGE_LOOP ( 'NONE', ( #16439, #43841 ) ) ;
#8210 = CARTESIAN_POINT ( 'NONE',  ( -50.42609385541305755, -14.90920654474423301, 69.97058823529410176 ) ) ;
#8211 = CARTESIAN_POINT ( 'NONE',  ( -22.50287964365704241, -20.25976079877567670, 65.90432929200700585 ) ) ;
#8212 = CARTESIAN_POINT ( 'NONE',  ( -17.15896312645611843, -7.363872641478732106, 70.68310009708541486 ) ) ;
#8213 = ADVANCED_FACE ( 'NONE', ( #23014 ), #4516, .T. ) ;
#8214 = ORIENTED_EDGE ( 'NONE', *, *, #22006, .F. ) ;
#8215 = CARTESIAN_POINT ( 'NONE',  ( -24.27033112822875438, -13.12649005559073068, 63.13264177271826583 ) ) ;
#8216 = EDGE_CURVE ( 'NONE', #1066, #28162, #45562, .T. ) ;
#8217 = CARTESIAN_POINT ( 'NONE',  ( -16.07865488608826254, -7.939723797651444315, 63.67011030349581091 ) ) ;
#8218 = CARTESIAN_POINT ( 'NONE',  ( -24.45125044792649049, -12.33277093510790579, 73.35570258362008644 ) ) ;
#8219 = ORIENTED_EDGE ( 'NONE', *, *, #27467, .F. ) ;
#8220 = CARTESIAN_POINT ( 'NONE',  ( -50.42609385541305755, -14.80920654474421205, 67.05882352941175384 ) ) ;
#8221 = CARTESIAN_POINT ( 'NONE',  ( -13.51885987070619954, -20.68321654889814099, 65.28629170358011891 ) ) ;
#8222 = CARTESIAN_POINT ( 'NONE',  ( -13.53325622885376944, -21.16256470055228789, 65.17124264509627096 ) ) ;
#8223 = DIRECTION ( 'NONE',  ( -5.731567514496413899E-31, -1.020425574103664789E-16, -1.000000000000000000 ) ) ;
#8224 = AXIS2_PLACEMENT_3D ( 'NONE', #21058, #46919, #20819 ) ;
#8225 =( BOUNDED_SURFACE ( )  B_SPLINE_SURFACE ( 3, 1, ( 
 ( #8933, #9896 ),
 ( #28371, #1780 ),
 ( #20245, #28607 ),
 ( #46358, #1529 ),
 ( #16778, #43634 ),
 ( #32057, #35730 ),
 ( #42903, #2255 ) ),
 .UNSPECIFIED., .T., .F., .F. ) 
 B_SPLINE_SURFACE_WITH_KNOTS ( ( 4, 3, 4 ),
 ( 2, 2 ),
 ( 0.000000000000000000, 0.5000000000000000000, 1.000000000000000000 ),
 ( 0.000000000000000000, 1.000000000000000000 ),
 .UNSPECIFIED. ) 
 GEOMETRIC_REPRESENTATION_ITEM ( )  RATIONAL_B_SPLINE_SURFACE ( (
 ( 1.000000000000000000, 1.000000000000000000),
 ( 0.3333333333333335369, 0.3333333333333330373),
 ( 0.3333333333333335369, 0.3333333333333330373),
 ( 1.000000000000000000, 1.000000000000000000),
 ( 0.3333333333333333703, 0.3333333333333333703),
 ( 0.3333333333333333703, 0.3333333333333333703),
 ( 1.000000000000000000, 1.000000000000000000) ) ) 
 REPRESENTATION_ITEM ( '' )  SURFACE ( )  );
#8226 = CARTESIAN_POINT ( 'NONE',  ( 18.57590614458695200, 1.636933384339416264, 51.78951792648778252 ) ) ;
#8227 = CARTESIAN_POINT ( 'NONE',  ( -18.81159385650551741, -6.922745924619793101, 51.69366785382590024 ) ) ;
#8228 = AXIS2_PLACEMENT_3D ( 'NONE', #15451, #8343, #37626 ) ;
#8229 = VERTEX_POINT ( 'NONE', #5250 ) ;
#8230 = FACE_OUTER_BOUND ( 'NONE', #37923, .T. ) ;
#8231 = CARTESIAN_POINT ( 'NONE',  ( -11.03586941931242826, -10.97581178645133093, 60.85698564304344416 ) ) ;
#8232 = VERTEX_POINT ( 'NONE', #584 ) ;
#8233 = FACE_OUTER_BOUND ( 'NONE', #41585, .T. ) ;
#8234 = DIRECTION ( 'NONE',  ( -2.866981220435666553E-17, 1.000000000000000000, 1.190614954331866791E-16 ) ) ;
#8235 = CARTESIAN_POINT ( 'NONE',  ( -7.924093855413059551, -6.359206544744109735, 47.99999999999998579 ) ) ;
#8236 = EDGE_LOOP ( 'NONE', ( #17613, #14548, #29950, #5178 ) ) ;
#8237 = PLANE ( 'NONE',  #5858 ) ;
#8238 = CARTESIAN_POINT ( 'NONE',  ( -16.93941734680483080, -7.775588144984237005, 74.24546186738449194 ) ) ;
#8239 = CARTESIAN_POINT ( 'NONE',  ( -10.08052675126636721, -16.06451543208143917, 68.09272439531302723 ) ) ;
#8240 = VERTEX_POINT ( 'NONE', #30642 ) ;
#8241 = CARTESIAN_POINT ( 'NONE',  ( -18.52802763510036499, -22.17709038376527175, 72.40794071233227669 ) ) ;
#8242 = CARTESIAN_POINT ( 'NONE',  ( -24.39137686751062617, -17.44764348928926623, 69.53622875020744232 ) ) ;
#8243 = CARTESIAN_POINT ( 'NONE',  ( -10.38847021856859421, -14.31440148336201545, 60.80332504197532728 ) ) ;
#8244 = FACE_OUTER_BOUND ( 'NONE', #15896, .T. ) ;
#8245 = CYLINDRICAL_SURFACE ( 'NONE', #13389, 0.4000000000000010214 ) ;
#8246 = ORIENTED_EDGE ( 'NONE', *, *, #28982, .T. ) ;
#8247 = EDGE_LOOP ( 'NONE', ( #22421, #5942 ) ) ;
#8248 = CARTESIAN_POINT ( 'NONE',  ( -22.29909385541304090, -8.105421454601382081, 49.25000573077640098 ) ) ;
#8249 = ADVANCED_FACE ( 'NONE', ( #830 ), #19795, .T. ) ;
#8250 = CARTESIAN_POINT ( 'NONE',  ( -16.89979169948162863, -10.14008855580012458, 52.02966884056656482 ) ) ;
#8251 = ADVANCED_FACE ( 'NONE', ( #41954, #20270, #27896 ), #12154, .T. ) ;
#8252 = CARTESIAN_POINT ( 'NONE',  ( -20.38078961538757028, -7.970959937923086436, 70.50746246719650401 ) ) ;
#8253 = CARTESIAN_POINT ( 'NONE',  ( -26.42409385541305511, -8.109206544744111511, 50.50000000000000000 ) ) ;
#8254 = AXIS2_PLACEMENT_3D ( 'NONE', #22582, #19367, #38071 ) ;
#8255 = CARTESIAN_POINT ( 'NONE',  ( -10.80190725398411011, -17.07816814126333327, 61.15743131804588728 ) ) ;
#8256 = CARTESIAN_POINT ( 'NONE',  ( -21.00642299473589247, -8.276168789376990631, 60.02780591114678543 ) ) ;
#8257 = CARTESIAN_POINT ( 'NONE',  ( -18.70000984002059852, -7.871953501822487098, 67.10891511697577982 ) ) ;
#8258 = CARTESIAN_POINT ( 'NONE',  ( 22.62590614458706639, 1.904620652374673151, 48.58033007082241994 ) ) ;
#8259 = ORIENTED_EDGE ( 'NONE', *, *, #45635, .T. ) ;
#8260 = PLANE ( 'NONE',  #40629 ) ;
#8261 = EDGE_CURVE ( 'NONE', #38822, #8715, #30881, .T. ) ;
#8262 = ORIENTED_EDGE ( 'NONE', *, *, #37841, .T. ) ;
#8263 = CARTESIAN_POINT ( 'NONE',  ( -19.14088062437382831, -4.707495580760234333, 53.49999999999995026 ) ) ;
#8264 = CARTESIAN_POINT ( 'NONE',  ( -9.974795159103587494, -14.91206505565066109, 74.99767674250446703 ) ) ;
#8265 = EDGE_CURVE ( 'NONE', #34680, #22085, #13006, .T. ) ;
#8267 = ADVANCED_FACE ( 'NONE', ( #8230 ), #23245, .T. ) ;
#8266 = FACE_OUTER_BOUND ( 'NONE', #45605, .T. ) ;
#8268 = CARTESIAN_POINT ( 'NONE',  ( -41.16232914953070576, -14.90920654474427565, 73.09411764705880898 ) ) ;
#8269 = EDGE_CURVE ( 'NONE', #17144, #10239, #25928, .T. ) ;
#8270 = ORIENTED_EDGE ( 'NONE', *, *, #34978, .F. ) ;
#8271 = CARTESIAN_POINT ( 'NONE',  ( -10.35661233123872371, -12.45241144375540365, 60.91358254413026430 ) ) ;
#8272 = CARTESIAN_POINT ( 'NONE',  ( -20.87473523085085247, -8.206369618537406652, 60.01842129422883687 ) ) ;
#8273 = VERTEX_POINT ( 'NONE', #39220 ) ;
#8274 = CARTESIAN_POINT ( 'NONE',  ( -18.44528782684011503, -21.78515541812411982, 72.29983070759432451 ) ) ;
#8275 = CARTESIAN_POINT ( 'NONE',  ( -17.72970361830877195, -22.25294841905989074, 58.50579124373946627 ) ) ;
#8276 = CARTESIAN_POINT ( 'NONE',  ( -10.88941126017583905, -11.23118345116917460, 64.27069259981260529 ) ) ;
#8277 = FACE_BOUND ( 'NONE', #31300, .T. ) ;
#8278 = CARTESIAN_POINT ( 'NONE',  ( -22.15958588924365102, -19.96439345820419220, 62.30727227379612287 ) ) ;
#8279 = CARTESIAN_POINT ( 'NONE',  ( -10.56627859465609376, -16.21290490039525167, 71.44750383612122846 ) ) ;
#8280 = LINE ( 'NONE', #640, #5372 ) ;
#8281 = CARTESIAN_POINT ( 'NONE',  ( -24.37542404773270022, -16.00605899042400537, 69.62487740803682357 ) ) ;
#8282 = VERTEX_POINT ( 'NONE', #24929 ) ;
#8283 = DIRECTION ( 'NONE',  ( -1.000000000000000000, -2.866981220435666553E-17, 0.000000000000000000 ) ) ;
#8284 = ORIENTED_EDGE ( 'NONE', *, *, #32978, .T. ) ;
#8285 = CARTESIAN_POINT ( 'NONE',  ( -12.20772364030515611, -10.14112086625394049, 64.32914330961887117 ) ) ;
#8286 = CARTESIAN_POINT ( 'NONE',  ( -12.36756753426621813, -9.896138138887707214, 57.37463480816234096 ) ) ;
#8287 = VERTEX_POINT ( 'NONE', #17030 ) ;
#8288 = AXIS2_PLACEMENT_3D ( 'NONE', #192, #29723, #30471 ) ;
#8289 = CARTESIAN_POINT ( 'NONE',  ( -12.75184123886795717, -9.006184337177792543, 70.98892004851447268 ) ) ;
#8290 = ORIENTED_EDGE ( 'NONE', *, *, #29668, .F. ) ;
#8291 = EDGE_CURVE ( 'NONE', #46544, #12446, #37070, .T. ) ;
#8292 = AXIS2_PLACEMENT_3D ( 'NONE', #10342, #43596, #28330 ) ;
#8293 = EDGE_LOOP ( 'NONE', ( #3779, #41037 ) ) ;
#8294 = ORIENTED_EDGE ( 'NONE', *, *, #10452, .F. ) ;
#8295 = LINE ( 'NONE', #8788, #47734 ) ;
#8296 = CARTESIAN_POINT ( 'NONE',  ( -19.44376929052122449, -7.638105555415076076, 60.07597592072836790 ) ) ;
#8297 = CARTESIAN_POINT ( 'NONE',  ( -17.39742543611924575, -7.759256981132186759, 67.32039592192056432 ) ) ;
#8298 =( BOUNDED_CURVE ( )  B_SPLINE_CURVE ( 3, ( #14311, #37208, #40925, #33768 ),
 .UNSPECIFIED., .F., .F. ) 
 B_SPLINE_CURVE_WITH_KNOTS ( ( 4, 4 ),
 ( 0.000000000000000000, 0.4074455897393644555 ),
 .UNSPECIFIED. ) 
 CURVE ( )  GEOMETRIC_REPRESENTATION_ITEM ( )  RATIONAL_B_SPLINE_CURVE ( ( 1.000000000000000000, 0.4567392136813305803, 0.3561768502900297673, 0.6983129098260976164 ) ) 
 REPRESENTATION_ITEM ( '' )  );
#8299 = LINE ( 'NONE', #11013, #35365 ) ;
#8300 = CARTESIAN_POINT ( 'NONE',  ( -10.43098718212803000, -15.70539730037032911, 61.32316937334011442 ) ) ;
#8301 = DIRECTION ( 'NONE',  ( 3.534154189880001717E-15, -4.519331686442879103E-31, -1.000000000000000000 ) ) ;
#8302 = EDGE_LOOP ( 'NONE', ( #1637, #16733 ) ) ;
#8303 = EDGE_LOOP ( 'NONE', ( #42000, #25665 ) ) ;
#8304 = LINE ( 'NONE', #16396, #1372 ) ;
#8305 = EDGE_CURVE ( 'NONE', #25305, #17691, #17284, .T. ) ;
#8306 = CARTESIAN_POINT ( 'NONE',  ( -9.990623107247818879, -14.31192343302863179, 64.57299167182827659 ) ) ;
#8307 = CARTESIAN_POINT ( 'NONE',  ( -21.04590028053454631, -21.31959600062944205, 62.21447769906016845 ) ) ;
#8308 = LINE ( 'NONE', #31191, #22907 ) ;
#8309 = ORIENTED_EDGE ( 'NONE', *, *, #3392, .F. ) ;
#8310 =( BOUNDED_CURVE ( )  B_SPLINE_CURVE ( 2, ( #41101, #18677, #12275, #37891, #717, #27056, #4650, #244, #38620 ),
 .UNSPECIFIED., .F., .F. ) 
 B_SPLINE_CURVE_WITH_KNOTS ( ( 3, 2, 2, 2, 3 ),
 ( 0.2916666666666666297, 0.3020833333333332593, 0.3124999999999999445, 0.3229166666666666297, 0.3333333333333332593 ),
 .UNSPECIFIED. ) 
 CURVE ( )  GEOMETRIC_REPRESENTATION_ITEM ( )  RATIONAL_B_SPLINE_CURVE ( ( 1.000000000000000444, 0.9238795325112862944, 1.000000000000000000, 0.9238795325112867385, 1.000000000000000000, 0.9238795325112867385, 1.000000000000000000, 0.9238795325112871826, 0.9999999999999995559 ) ) 
 REPRESENTATION_ITEM ( '' )  );
#8311 = CARTESIAN_POINT ( 'NONE',  ( -14.76159385650551847, -9.295667164867525756, 49.30633214617472504 ) ) ;
#8312 =( BOUNDED_CURVE ( )  B_SPLINE_CURVE ( 3, ( #23651, #34947, #39130, #990 ),
 .UNSPECIFIED., .F., .F. ) 
 B_SPLINE_CURVE_WITH_KNOTS ( ( 4, 4 ),
 ( 4.712388980384689674, 4.921828490624010399 ),
 .UNSPECIFIED. ) 
 CURVE ( )  GEOMETRIC_REPRESENTATION_ITEM ( )  RATIONAL_B_SPLINE_CURVE ( ( 1.000000000000000000, 0.9963479302455154896, 0.9963479302455154896, 1.000000000000000000 ) ) 
 REPRESENTATION_ITEM ( '' )  );
#8313 = ORIENTED_EDGE ( 'NONE', *, *, #18818, .T. ) ;
#8314 = CARTESIAN_POINT ( 'NONE',  ( -24.70578670907444163, -13.23458007007709547, 59.51267921514076420 ) ) ;
#8315 = CARTESIAN_POINT ( 'NONE',  ( -16.55933827844250672, -21.80960967909763681, 68.78740806194913660 ) ) ;
#8316 = CYLINDRICAL_SURFACE ( 'NONE', #27605, 0.1500000000000052125 ) ;
#8317 = ORIENTED_EDGE ( 'NONE', *, *, #32128, .F. ) ;
#8318 = DIRECTION ( 'NONE',  ( -1.000000000000000000, 0.000000000000000000, 0.000000000000000000 ) ) ;
#8319 =( BOUNDED_CURVE ( )  B_SPLINE_CURVE ( 3, ( #4627, #44012, #13447, #20855 ),
 .UNSPECIFIED., .F., .F. ) 
 B_SPLINE_CURVE_WITH_KNOTS ( ( 4, 4 ),
 ( 0.5000000000000000000, 0.9074455897393642889 ),
 .UNSPECIFIED. ) 
 CURVE ( )  GEOMETRIC_REPRESENTATION_ITEM ( )  RATIONAL_B_SPLINE_CURVE ( ( 1.000000000000025313, 0.4567392136813321901, 0.3561768502900123923, 0.6983129098260936196 ) ) 
 REPRESENTATION_ITEM ( '' )  );
#8320 = CIRCLE ( 'NONE', #46064, 0.3999999999999975797 ) ;
#8321 = CARTESIAN_POINT ( 'NONE',  ( -11.37476892658000160, -19.15884210479704208, 68.33034228280476441 ) ) ;
#8322 = EDGE_CURVE ( 'NONE', #3873, #43420, #42095, .T. ) ;
#8323 = EDGE_CURVE ( 'NONE', #33825, #31312, #24700, .T. ) ;
#8324 = CARTESIAN_POINT ( 'NONE',  ( -12.26841837488882092, -9.996323195260892192, 56.97446934404248964 ) ) ;
#8325 = ORIENTED_EDGE ( 'NONE', *, *, #42461, .F. ) ;
#8326 = CARTESIAN_POINT ( 'NONE',  ( -10.43905175586412426, -15.29054565531327370, 57.75719864210760335 ) ) ;
#8327 = CARTESIAN_POINT ( 'NONE',  ( -17.50157081909136991, -7.358860168393607459, 67.20694839074946003 ) ) ;
#8328 = FACE_OUTER_BOUND ( 'NONE', #10494, .T. ) ;
#8329 = ORIENTED_EDGE ( 'NONE', *, *, #23169, .F. ) ;
#8330 = CYLINDRICAL_SURFACE ( 'NONE', #5536, 2.000000000000001776 ) ;
#8331 = VERTEX_POINT ( 'NONE', #47815 ) ;
#8332 = CARTESIAN_POINT ( 'NONE',  ( -36.42409385541304800, -8.109206544743658540, 50.50000000000030553 ) ) ;
#8333 = ADVANCED_FACE ( 'NONE', ( #32078 ), #38634, .T. ) ;
#8334 = EDGE_CURVE ( 'NONE', #25294, #6432, #42391, .T. ) ;
#8335 = ORIENTED_EDGE ( 'NONE', *, *, #44079, .F. ) ;
#8336 = CARTESIAN_POINT ( 'NONE',  ( -16.29919166237813144, -22.17386956490665639, 62.01214078850637890 ) ) ;
#8337 = DIRECTION ( 'NONE',  ( 0.9687793358424821033, -0.2479245821708677133, 0.000000000000000000 ) ) ;
#8338 = ORIENTED_EDGE ( 'NONE', *, *, #29806, .F. ) ;
#8339 = CARTESIAN_POINT ( 'NONE',  ( -22.12520620670305860, -9.029593692166299590, 63.31436867790266376 ) ) ;
#8340 = CARTESIAN_POINT ( 'NONE',  ( -16.27008067537174796, -7.904986561263926959, 60.50028479261354875 ) ) ;
#8341 = DIRECTION ( 'NONE',  ( 9.009792911740839922E-08, -1.813722297350279449E-06, 0.9999999999983510968 ) ) ;
#8342 = ORIENTED_EDGE ( 'NONE', *, *, #4644, .T. ) ;
#8343 = DIRECTION ( 'NONE',  ( 0.9087012777736581670, -0.4174469879787381932, -4.853707507795077342E-09 ) ) ;
#8344 = CARTESIAN_POINT ( 'NONE',  ( -16.42409385759798823, -9.359200813967568422, 50.49621490985803263 ) ) ;
#8345 = EDGE_CURVE ( 'NONE', #7976, #19337, #8641, .T. ) ;
#8346 = ORIENTED_EDGE ( 'NONE', *, *, #37354, .T. ) ;
#8347 = EDGE_LOOP ( 'NONE', ( #19416, #30454, #46569, #25315 ) ) ;
#8348 = CARTESIAN_POINT ( 'NONE',  ( -23.30282546666849086, -18.60927426030231047, 69.59371984657600763 ) ) ;
#8349 = CARTESIAN_POINT ( 'NONE',  ( -10.70296955259081351, -11.59513340129999648, 71.27356289404251299 ) ) ;
#8350 = CARTESIAN_POINT ( 'NONE',  ( -15.28291064399146038, -21.52618758091310980, 68.57592918174772478 ) ) ;
#8351 = CARTESIAN_POINT ( 'NONE',  ( -21.06159385650551741, -9.295667164867525756, 49.30633214617472504 ) ) ;
#8352 = CARTESIAN_POINT ( 'NONE',  ( -24.45563843384471880, -14.25946414430215903, 73.53760260359439371 ) ) ;
#8353 = CARTESIAN_POINT ( 'NONE',  ( -11.35824946695446691, -11.21643166988602047, 60.82885780703593070 ) ) ;
#8354 = CARTESIAN_POINT ( 'NONE',  ( -18.58355647720519599, -7.449975798599677290, 74.04053169813657576 ) ) ;
#8355 = CARTESIAN_POINT ( 'NONE',  ( -10.34288728022239923, -21.73268535153714254, 53.49999999999995026 ) ) ;
#8356 = ORIENTED_EDGE ( 'NONE', *, *, #35666, .T. ) ;
#8357 = VERTEX_POINT ( 'NONE', #6466 ) ;
#8358 = DIRECTION ( 'NONE',  ( -3.071710424422018668E-17, 6.404604876783312462E-16, 1.000000000000000000 ) ) ;
#8359 = CARTESIAN_POINT ( 'NONE',  ( -14.41791765924166135, -21.19496194411871315, 58.31050579099508724 ) ) ;
#8360 = CARTESIAN_POINT ( 'NONE',  ( -10.91670087826603464, -17.52156819001323740, 68.39721947804264346 ) ) ;
#8361 = DIRECTION ( 'NONE',  ( 0.9325317756203296282, -0.3459670625490731677, -0.1033986416233826505 ) ) ;
#8362 = ORIENTED_EDGE ( 'NONE', *, *, #23521, .F. ) ;
#8363 = ORIENTED_EDGE ( 'NONE', *, *, #30565, .F. ) ;
#8364 = PLANE ( 'NONE',  #12308 ) ;
#8365 = CARTESIAN_POINT ( 'NONE',  ( -19.60046948880987117, -21.46228020301366257, 65.76486213989072382 ) ) ;
#8366 = DIRECTION ( 'NONE',  ( 1.000000000000000000, -4.164305804376849172E-17, 1.614929280266638808E-16 ) ) ;
#8367 = CARTESIAN_POINT ( 'NONE',  ( -11.58245751978128268, -10.85571050334743859, 57.50903504724044524 ) ) ;
#8368 = ORIENTED_EDGE ( 'NONE', *, *, #25971, .T. ) ;
#8369 = CARTESIAN_POINT ( 'NONE',  ( -12.88390949798720619, -15.97110509908812936, 52.02966884056656482 ) ) ;
#8370 = CARTESIAN_POINT ( 'NONE',  ( -24.41553149706675896, -15.71832598455623398, 69.81835354388927328 ) ) ;
#8371 = EDGE_CURVE ( 'NONE', #43656, #38294, #47921, .T. ) ;
#8372 = VERTEX_POINT ( 'NONE', #17756 ) ;
#8373 = CARTESIAN_POINT ( 'NONE',  ( -12.88826169612582717, -20.14091212239222983, 72.09188343144306543 ) ) ;
#8374 = CARTESIAN_POINT ( 'NONE',  ( -13.79242041809915875, -8.303469675591347965, 74.31299407998417905 ) ) ;
#8375 = ORIENTED_EDGE ( 'NONE', *, *, #47773, .T. ) ;
#8376 = CARTESIAN_POINT ( 'NONE',  ( -12.36019758273501701, -19.71856390219481980, 65.28163476484961336 ) ) ;
#8377 = CIRCLE ( 'NONE', #48440, 4.686499999999999666 ) ;
#8378 = VECTOR ( 'NONE', #5403, 1000.000000000000000 ) ;
#8379 = ORIENTED_EDGE ( 'NONE', *, *, #19746, .F. ) ;
#8380 = EDGE_CURVE ( 'NONE', #5475, #34362, #22241, .T. ) ;
#8381 = PLANE ( 'NONE',  #27528 ) ;
#8382 = CARTESIAN_POINT ( 'NONE',  ( -23.77312771997254615, -18.70709664074277612, 72.87872845841107505 ) ) ;
#8383 = ORIENTED_EDGE ( 'NONE', *, *, #13802, .T. ) ;
#8384 = CARTESIAN_POINT ( 'NONE',  ( -20.34937902005098920, -7.957549317960647350, 70.40100341510218129 ) ) ;
#8385 = CARTESIAN_POINT ( 'NONE',  ( -18.64625997845222116, -21.76055708611507100, 68.97081679896227513 ) ) ;
#8386 = EDGE_CURVE ( 'NONE', #14119, #39039, #38924, .T. ) ;
#8387 = CARTESIAN_POINT ( 'NONE',  ( -19.12409385650551741, -6.426201560718813433, 50.50509628382439331 ) ) ;
#8388 = CARTESIAN_POINT ( 'NONE',  ( -21.35088739213495757, -21.14050036012818268, 69.21596729481782972 ) ) ;
#8389 =( BOUNDED_SURFACE ( )  B_SPLINE_SURFACE ( 3, 1, ( 
 ( #37445, #2999 ),
 ( #22212, #44163 ),
 ( #40665, #44624 ),
 ( #14533, #29354 ),
 ( #32793, #47593 ),
 ( #10642, #18006 ),
 ( #6948, #6706 ) ),
 .UNSPECIFIED., .T., .F., .F. ) 
 B_SPLINE_SURFACE_WITH_KNOTS ( ( 4, 3, 4 ),
 ( 2, 2 ),
 ( 0.000000000000000000, 0.5000000000000000000, 1.000000000000000000 ),
 ( 0.000000000000000000, 1.000000000000000000 ),
 .UNSPECIFIED. ) 
 GEOMETRIC_REPRESENTATION_ITEM ( )  RATIONAL_B_SPLINE_SURFACE ( (
 ( 1.000000000000000000, 1.000000000000000000),
 ( 0.3333333333333335369, 0.3333333333333330373),
 ( 0.3333333333333335369, 0.3333333333333330373),
 ( 1.000000000000000000, 1.000000000000000000),
 ( 0.3333333333333333703, 0.3333333333333333703),
 ( 0.3333333333333333703, 0.3333333333333333703),
 ( 1.000000000000000000, 1.000000000000000000) ) ) 
 REPRESENTATION_ITEM ( '' )  SURFACE ( )  );
#8390 = EDGE_CURVE ( 'NONE', #40074, #17102, #4695, .T. ) ;
#8391 = CARTESIAN_POINT ( 'NONE',  ( -19.30978178441422699, -7.601027468210772575, 63.61744607541091767 ) ) ;
#8392 = CARTESIAN_POINT ( 'NONE',  ( -50.42609385541305755, -14.90920654474426499, 72.98823529411762934 ) ) ;
#8393 = ORIENTED_EDGE ( 'NONE', *, *, #48116, .T. ) ;
#8394 = CARTESIAN_POINT ( 'NONE',  ( -24.47371109942907808, -14.90716652360855576, 59.25772288469824645 ) ) ;
#8395 = DIRECTION ( 'NONE',  ( 0.000000000000000000, -0.000000000000000000, -1.000000000000000000 ) ) ;
#8396 = CARTESIAN_POINT ( 'NONE',  ( -13.62949042321701398, -8.926946430974666669, 56.96967755885751217 ) ) ;
#8397 = CARTESIAN_POINT ( 'NONE',  ( -18.44140615910215431, -21.73495079426802690, 69.04187996903171154 ) ) ;
#8398 = CARTESIAN_POINT ( 'NONE',  ( -12.36019758273501701, -19.71856390219481980, 65.28163476484961336 ) ) ;
#8399 = EDGE_LOOP ( 'NONE', ( #18707, #36073 ) ) ;
#8400 = ORIENTED_EDGE ( 'NONE', *, *, #42193, .T. ) ;
#8401 = FACE_OUTER_BOUND ( 'NONE', #41398, .T. ) ;
#8402 = CARTESIAN_POINT ( 'NONE',  ( -24.30032249061147098, -16.12038754366300353, 62.59328623469320974 ) ) ;
#8403 = EDGE_LOOP ( 'NONE', ( #16910, #27933 ) ) ;
#8404 = CARTESIAN_POINT ( 'NONE',  ( -41.41379973776600565, -14.90920654474425433, 71.08235294117645253 ) ) ;
#8405 = CARTESIAN_POINT ( 'NONE',  ( -15.82259855879412846, -7.533287975791289171, 67.25511890406325222 ) ) ;
#8406 = CARTESIAN_POINT ( 'NONE',  ( -20.64284385759799179, -7.587656875400192291, 49.25157356644813689 ) ) ;
#8407 = CARTESIAN_POINT ( 'NONE',  ( -22.11926001268504294, -9.024814352312150234, 63.30658345311071855 ) ) ;
#8408 = CARTESIAN_POINT ( 'NONE',  ( -18.14707656476823772, -21.82566862371319871, 62.08355883028285405 ) ) ;
#8409 = CARTESIAN_POINT ( 'NONE',  ( -15.84273041897837864, -7.988518076557024727, 70.72063026278281939 ) ) ;
#8410 = CARTESIAN_POINT ( 'NONE',  ( -16.32745258320347759, -21.77369344365219561, 61.77040269689842944 ) ) ;
#8411 = ORIENTED_EDGE ( 'NONE', *, *, #5615, .T. ) ;
#8412 = CARTESIAN_POINT ( 'NONE',  ( -13.44904343725875684, -12.32681728777199481, 49.52966884056655772 ) ) ;
#8413 = B_SPLINE_CURVE_WITH_KNOTS ( 'NONE', 3,
 ( #3432, #6890, #3679, #11074, #17950, #18437, #21667, #37144, #29536, #29791 ),
 .UNSPECIFIED., .F., .F.,
 ( 4, 2, 2, 2, 4 ),
 ( 0.000000000000000000, 0.2500000000000000000, 0.5000000000000000000, 0.7500000000000000000, 1.000000000000000000 ),
 .UNSPECIFIED. ) ;
#8414 = CARTESIAN_POINT ( 'NONE',  ( -19.74200936563729769, -21.46758226568296024, 68.94954551542706156 ) ) ;
#8415 = CARTESIAN_POINT ( 'NONE',  ( -50.42609385541305755, -14.80920654474416764, 63.03529411764704804 ) ) ;
#8416 = CARTESIAN_POINT ( 'NONE',  ( -20.70232472158584969, -8.624289250480600799, 59.84125250310036392 ) ) ;
#8417 = CARTESIAN_POINT ( 'NONE',  ( -15.96294338902451493, -7.962954265068761472, 67.42390783910214225 ) ) ;
#8418 = ORIENTED_EDGE ( 'NONE', *, *, #33650, .T. ) ;
#8419 = VECTOR ( 'NONE', #18, 999.9999999999998863 ) ;
#8420 = ORIENTED_EDGE ( 'NONE', *, *, #31788, .T. ) ;
#8421 = AXIS2_PLACEMENT_3D ( 'NONE', #29623, #6004, #21027 ) ;
#8422 = CARTESIAN_POINT ( 'NONE',  ( -22.18659385650551741, -9.302874398569244363, 51.68646062012417985 ) ) ;
#8423 = ORIENTED_EDGE ( 'NONE', *, *, #24903, .F. ) ;
#8424 = DIRECTION ( 'NONE',  ( 0.000000000000000000, 1.000000000000000000, 0.000000000000000000 ) ) ;
#8425 = CARTESIAN_POINT ( 'NONE',  ( -11.77169535943213319, -10.59578862612641714, 74.73885051658085388 ) ) ;
#8426 = CIRCLE ( 'NONE', #34383, 1.999999999999999556 ) ;
#8427 = EDGE_CURVE ( 'NONE', #18022, #4434, #44185, .T. ) ;
#8428 = ORIENTED_EDGE ( 'NONE', *, *, #41946, .T. ) ;
#8429 = DIRECTION ( 'NONE',  ( -0.3478314405900309048, -0.9375570856950864451, 0.000000000000000000 ) ) ;
#8430 = CARTESIAN_POINT ( 'NONE',  ( -16.06904454444675778, -7.890656075740461795, 63.67011029959335389 ) ) ;
#8431 = EDGE_LOOP ( 'NONE', ( #7135, #12321, #16287, #22248, #35584 ) ) ;
#8432 = CARTESIAN_POINT ( 'NONE',  ( -20.88147576600584543, -8.209942340109883219, 60.02620652709861560 ) ) ;
#8433 = CARTESIAN_POINT ( 'NONE',  ( -10.48085350821551742, -13.91959267249018950, 57.44825035245948186 ) ) ;
#8434 = ORIENTED_EDGE ( 'NONE', *, *, #1616, .T. ) ;
#8435 =( BOUNDED_CURVE ( )  B_SPLINE_CURVE ( 3, ( #47980, #14216, #29271, #8096 ),
 .UNSPECIFIED., .F., .F. ) 
 B_SPLINE_CURVE_WITH_KNOTS ( ( 4, 4 ),
 ( 0.4074455897393700066, 0.5000000000000000000 ),
 .UNSPECIFIED. ) 
 CURVE ( )  GEOMETRIC_REPRESENTATION_ITEM ( )  RATIONAL_B_SPLINE_CURVE ( ( 0.6983129098261058321, 0.7760317562607081943, 0.8765941196520058432, 0.9999999999999983347 ) ) 
 REPRESENTATION_ITEM ( '' )  );
#8436 = CARTESIAN_POINT ( 'NONE',  ( -11.30361347545239958, -11.41219030243732391, 64.14882039658046153 ) ) ;
#8437 = VERTEX_POINT ( 'NONE', #14526 ) ;
#8438 = CARTESIAN_POINT ( 'NONE',  ( -17.42409385541299471, -14.80920654474435771, 49.52966884056655772 ) ) ;
#8439 = CARTESIAN_POINT ( 'NONE',  ( -12.43150676794136089, -13.18545343111793855, 50.77966884056655772 ) ) ;
#8440 = VERTEX_POINT ( 'NONE', #3479 ) ;
#8441 = CARTESIAN_POINT ( 'NONE',  ( -12.77926086925118554, -20.11284637564935807, 71.80653681455748938 ) ) ;
#8442 = EDGE_CURVE ( 'NONE', #42114, #20623, #44617, .T. ) ;
#8443 = ADVANCED_FACE ( 'NONE', ( #6939 ), #16624, .T. ) ;
#8444 = CARTESIAN_POINT ( 'NONE',  ( -15.25055861359784259, -21.51969010973779817, 72.34575615124376213 ) ) ;
#8445 = CARTESIAN_POINT ( 'NONE',  ( -21.29994498387370427, -20.70774380606181708, 65.74020874375150925 ) ) ;
#8446 = CARTESIAN_POINT ( 'NONE',  ( -24.37947880424689018, -14.01905714813458914, 73.12271482014924118 ) ) ;
#8448 =( BOUNDED_CURVE ( )  B_SPLINE_CURVE ( 3, ( #6570, #35199, #12795, #9118 ),
 .UNSPECIFIED., .F., .F. ) 
 B_SPLINE_CURVE_WITH_KNOTS ( ( 4, 4 ),
 ( 0.5000000000000000000, 0.9074455897393685078 ),
 .UNSPECIFIED. ) 
 CURVE ( )  GEOMETRIC_REPRESENTATION_ITEM ( )  RATIONAL_B_SPLINE_CURVE ( ( 1.000000000000005995, 0.4567392136813286929, 0.3561768502900247713, 0.6983129098261008361 ) ) 
 REPRESENTATION_ITEM ( '' )  );
#8447 = CARTESIAN_POINT ( 'NONE',  ( -10.42334066387008029, -15.64104445138816146, 61.03789045260960222 ) ) ;
#8449 = AXIS2_PLACEMENT_3D ( 'NONE', #10822, #28815, #36188 ) ;
#8450 = AXIS2_PLACEMENT_3D ( 'NONE', #47730, #21636, #39859 ) ;
#8451 = LINE ( 'NONE', #31340, #5360 ) ;
#8452 = CARTESIAN_POINT ( 'NONE',  ( -45.92409385541306222, -14.20920654474410760, 70.50000000000000000 ) ) ;
#8453 = EDGE_CURVE ( 'NONE', #26883, #19332, #14772, .T. ) ;
#8454 = CARTESIAN_POINT ( 'NONE',  ( -13.49409790474204840, -20.66256726344224504, 61.53118467422925164 ) ) ;
#8455 = CARTESIAN_POINT ( 'NONE',  ( -17.29284385650551670, -7.406986770994972602, 48.81910596585309747 ) ) ;
#8456 = ORIENTED_EDGE ( 'NONE', *, *, #681, .F. ) ;
#8457 = CARTESIAN_POINT ( 'NONE',  ( -21.78913961794832588, -8.771810275399618106, 70.24637145832762997 ) ) ;
#8458 = CARTESIAN_POINT ( 'NONE',  ( -24.26085316502931377, -16.31268185143223093, 59.12332382745086079 ) ) ;
#8459 = ORIENTED_EDGE ( 'NONE', *, *, #40614, .T. ) ;
#8460 = CARTESIAN_POINT ( 'NONE',  ( -17.42409385541299471, -14.80920654474435594, 52.02966884056656482 ) ) ;
#8461 = CYLINDRICAL_SURFACE ( 'NONE', #43617, 0.1500000000000051847 ) ;
#8462 = AXIS2_PLACEMENT_3D ( 'NONE', #4270, #38219, #22998 ) ;
#8463 = CARTESIAN_POINT ( 'NONE',  ( -12.71430834099865415, -19.98797453911052457, 68.63657440637429374 ) ) ;
#8464 = CARTESIAN_POINT ( 'NONE',  ( -17.65006842549283306, -20.30456235612524196, 53.49999999999995026 ) ) ;
#8465 = EDGE_CURVE ( 'NONE', #15068, #40396, #44816, .T. ) ;
#8466 = EDGE_LOOP ( 'NONE', ( #5217, #27514, #17967, #24117, #36220 ) ) ;
#8467 = ADVANCED_FACE ( 'NONE', ( #37694 ), #28845, .T. ) ;
#8468 = CARTESIAN_POINT ( 'NONE',  ( -10.37852926856506386, -14.47236211977926246, 71.41962671695536358 ) ) ;
#8469 = CARTESIAN_POINT ( 'NONE',  ( -17.19980177718173309, -7.762775310937220397, 70.49035839668022163 ) ) ;
#8470 = CARTESIAN_POINT ( 'NONE',  ( -24.00447786525511518, -11.31618815658438315, 66.62203293136848004 ) ) ;
#8471 = ORIENTED_EDGE ( 'NONE', *, *, #34691, .F. ) ;
#8472 = CARTESIAN_POINT ( 'NONE',  ( -18.52866185626436746, -22.17699158182255559, 72.46323720911766486 ) ) ;
#8473 = FACE_OUTER_BOUND ( 'NONE', #45518, .T. ) ;
#8474 = CARTESIAN_POINT ( 'NONE',  ( -23.98503169607928953, -17.39005800936845603, 66.22885190747201989 ) ) ;
#8475 = B_SPLINE_CURVE_WITH_KNOTS ( 'NONE', 3,
 ( #4832, #42504, #1122, #16122, #43480, #24529, #13155, #32618, #43719, #2094 ),
 .UNSPECIFIED., .F., .F.,
 ( 4, 2, 2, 2, 4 ),
 ( 0.1272669073659042638, 0.2522669073487938673, 0.3772669073316834432, 0.5022669073145730190, 0.6272669072974625948 ),
 .UNSPECIFIED. ) ;
#8476 = CARTESIAN_POINT ( 'NONE',  ( -18.24390634433515856, -19.99480269976908176, 49.52966884056656482 ) ) ;
#8477 = CARTESIAN_POINT ( 'NONE',  ( -45.92409385541305511, -17.80920654474410370, 70.50000000000000000 ) ) ;
#8478 = VERTEX_POINT ( 'NONE', #44380 ) ;
#8479 = ORIENTED_EDGE ( 'NONE', *, *, #36552, .F. ) ;
#8480 = CARTESIAN_POINT ( 'NONE',  ( -22.46784385541304374, -9.357632978295830739, 49.97845033065684106 ) ) ;
#8481 = DIRECTION ( 'NONE',  ( -3.071710424422018668E-17, 6.404604876783312462E-16, 1.000000000000000000 ) ) ;
#8482 = CARTESIAN_POINT ( 'NONE',  ( -23.37982836330400005, -11.13088026761028182, 73.64727903829775357 ) ) ;
#8483 = LINE ( 'NONE', #30421, #11929 ) ;
#8484 = EDGE_CURVE ( 'NONE', #43615, #21832, #21824, .T. ) ;
#8485 = VECTOR ( 'NONE', #9331, 1000.000000000000114 ) ;
#8486 = CIRCLE ( 'NONE', #12415, 0.5560000000000009379 ) ;
#8487 = B_SPLINE_CURVE_WITH_KNOTS ( 'NONE', 1,
 ( #44300, #36869 ),
 .UNSPECIFIED., .F., .F.,
 ( 2, 2 ),
 ( 0.000000000000000000, 1.000000000000000000 ),
 .UNSPECIFIED. ) ;
#8488 = CARTESIAN_POINT ( 'NONE',  ( -17.42409385541299471, -14.80920654474435771, 49.52966884056655772 ) ) ;
#8489 = CARTESIAN_POINT ( 'NONE',  ( -20.48833051011514073, -8.513735643284267240, 66.97031093069610108 ) ) ;
#8490 = CARTESIAN_POINT ( 'NONE',  ( -20.32146343473794303, -8.373352561929221949, 73.86529255602565058 ) ) ;
#8491 = CIRCLE ( 'NONE', #42313, 0.5560000000000009379 ) ;
#8492 = CARTESIAN_POINT ( 'NONE',  ( -24.75383108144848165, -16.14659837148148824, 66.24980321609697853 ) ) ;
#8493 = ORIENTED_EDGE ( 'NONE', *, *, #9347, .T. ) ;
#8494 = CARTESIAN_POINT ( 'NONE',  ( -22.01092588021961660, -8.937695967300268052, 66.84805351483468883 ) ) ;
#8495 = ADVANCED_FACE ( 'NONE', ( #8401 ), #27107, .T. ) ;
#8496 = CARTESIAN_POINT ( 'NONE',  ( -17.42409385541299471, -14.80920654474435771, 49.52966884056655772 ) ) ;
#8497 = ORIENTED_EDGE ( 'NONE', *, *, #7644, .F. ) ;
#8498 = FACE_OUTER_BOUND ( 'NONE', #32042, .T. ) ;
#8499 = CARTESIAN_POINT ( 'NONE',  ( -13.64083825785024295, -8.860125017712917384, 56.97527577494557249 ) ) ;
#8500 = VERTEX_POINT ( 'NONE', #15770 ) ;
#8501 = CARTESIAN_POINT ( 'NONE',  ( -18.14803087600414955, -22.22395683015660239, 65.54543360577268629 ) ) ;
#8502 = CARTESIAN_POINT ( 'NONE',  ( -14.95535764022100977, -18.80681796222810576, 49.52966884056656482 ) ) ;
#8503 = CARTESIAN_POINT ( 'NONE',  ( -20.19053640067075506, -7.838066347919499854, 54.27966884056654351 ) ) ;
#8504 = CARTESIAN_POINT ( 'NONE',  ( -17.58219478024370730, -20.05682544264153933, 50.77966884056656482 ) ) ;
#8505 = EDGE_LOOP ( 'NONE', ( #18843, #24171, #21513, #20822, #44751 ) ) ;
#8506 = CARTESIAN_POINT ( 'NONE',  ( -21.68042710870613732, -9.185287987594811909, 63.07665001108087921 ) ) ;
#8507 = FACE_OUTER_BOUND ( 'NONE', #13457, .T. ) ;
#8508 = CARTESIAN_POINT ( 'NONE',  ( -23.81024772113315890, -18.64597811008791695, 72.94863512192290500 ) ) ;
#8509 = FACE_OUTER_BOUND ( 'NONE', #15654, .T. ) ;
#8510 = SHAPE_DEFINITION_REPRESENTATION ( #35058, #46513 ) ;
#8511 = ADVANCED_FACE ( 'NONE', ( #20203 ), #22954, .T. ) ;
#8512 = CARTESIAN_POINT ( 'NONE',  ( -11.44474483503512197, -18.44890233052262829, 57.99817723587980112 ) ) ;
#8513 = CARTESIAN_POINT ( 'NONE',  ( -18.34350352696802844, -21.80264126034385441, 65.55352047473381560 ) ) ;
#8514 = EDGE_CURVE ( 'NONE', #12740, #11221, #3592, .T. ) ;
#8515 = CARTESIAN_POINT ( 'NONE',  ( 18.46573386768564973, 3.114729847419841047, 50.78398819077492732 ) ) ;
#8516 = ORIENTED_EDGE ( 'NONE', *, *, #18582, .F. ) ;
#8517 = DIRECTION ( 'NONE',  ( 0.4599824152910792496, 0.8879280250239794947, 2.250728352126283681E-08 ) ) ;
#8518 = ADVANCED_FACE ( 'NONE', ( #26634 ), #40493, .T. ) ;
#8519 = ORIENTED_EDGE ( 'NONE', *, *, #39944, .T. ) ;
#8520 = VECTOR ( 'NONE', #36653, 1000.000000000000114 ) ;
#8521 = DIRECTION ( 'NONE',  ( -1.075201462585828720E-05, 1.608194665399622665E-06, 0.9999999999409039386 ) ) ;
#8522 = CARTESIAN_POINT ( 'NONE',  ( -13.25597978444290170, -9.183840967339035544, 67.45113130188182993 ) ) ;
#8523 = ORIENTED_EDGE ( 'NONE', *, *, #27126, .F. ) ;
#8524 = CARTESIAN_POINT ( 'NONE',  ( -14.86627107493491984, -7.811969877679347363, 56.96504568426624360 ) ) ;
#8525 = CIRCLE ( 'NONE', #9298, 1.999999999999994893 ) ;
#8526 = VECTOR ( 'NONE', #46495, 1000.000000000000000 ) ;
#8527 = FACE_BOUND ( 'NONE', #9626, .T. ) ;
#8528 = B_SPLINE_CURVE_WITH_KNOTS ( 'NONE', 3,
 ( #37847, #4857, #4138, #15416, #30484, #45498, #11756, #1142, #16147, #26778 ),
 .UNSPECIFIED., .F., .F.,
 ( 4, 2, 2, 2, 4 ),
 ( 0.000000000000000000, 0.2500000000000000000, 0.5000000000000000000, 0.7500000000000000000, 1.000000000000000000 ),
 .UNSPECIFIED. ) ;
#8529 = VERTEX_POINT ( 'NONE', #15517 ) ;
#8530 = VERTEX_POINT ( 'NONE', #11858 ) ;
#8531 = ORIENTED_EDGE ( 'NONE', *, *, #7106, .F. ) ;
#8532 = DIRECTION ( 'NONE',  ( 0.000000000000000000, 1.000000000000000000, -0.000000000000000000 ) ) ;
#8533 = LINE ( 'NONE', #34622, #21632 ) ;
#8534 = CARTESIAN_POINT ( 'NONE',  ( -17.44579964618406009, -7.359071133328546566, 67.18186073236977052 ) ) ;
#8535 = EDGE_CURVE ( 'NONE', #44852, #26302, #41895, .T. ) ;
#8536 = CARTESIAN_POINT ( 'NONE',  ( -10.27391136003569905, -12.71670657087258327, 64.31190181376453552 ) ) ;
#8537 = CARTESIAN_POINT ( 'NONE',  ( -12.52694624409642898, -20.42352324341258907, 72.00664875469250603 ) ) ;
#8538 = EDGE_CURVE ( 'NONE', #12573, #38501, #38175, .T. ) ;
#8539 = ORIENTED_EDGE ( 'NONE', *, *, #47721, .T. ) ;
#8540 = ORIENTED_EDGE ( 'NONE', *, *, #231, .F. ) ;
#8541 = CARTESIAN_POINT ( 'NONE',  ( -22.27409385650551243, -9.792211528768504536, 50.49490371617623197 ) ) ;
#8542 = EDGE_CURVE ( 'NONE', #19435, #1693, #31053, .T. ) ;
#8543 = EDGE_CURVE ( 'NONE', #30739, #11687, #33473, .T. ) ;
#8544 = LINE ( 'NONE', #35360, #9479 ) ;
#8545 = DIRECTION ( 'NONE',  ( 1.420801291081008049E-06, 1.008342286629444690E-05, -0.9999999999481530288 ) ) ;
#8546 = DIRECTION ( 'NONE',  ( -0.9687793358424819923, 0.2479245821708680464, 0.000000000000000000 ) ) ;
#8547 = EDGE_LOOP ( 'NONE', ( #14794, #1681, #31046, #40880, #48704 ) ) ;
#8548 = CARTESIAN_POINT ( 'NONE',  ( -21.54284385650551670, -8.811426318492348031, 52.18089403414751359 ) ) ;
#8549 = ORIENTED_EDGE ( 'NONE', *, *, #44949, .T. ) ;
#8550 = CARTESIAN_POINT ( 'NONE',  ( -21.54665965586444543, -9.090157682337041578, 70.13132566468406992 ) ) ;
#8551 = CARTESIAN_POINT ( 'NONE',  ( -15.37138615481495840, -21.50153415455971384, 68.86127572257412055 ) ) ;
#8552 = AXIS2_PLACEMENT_3D ( 'NONE', #32834, #37246, #3296 ) ;
#8553 = CARTESIAN_POINT ( 'NONE',  ( -10.40277079310570052, -15.44444055846370745, 57.71792809063055785 ) ) ;
#8554 = VECTOR ( 'NONE', #16024, 1000.000000000000000 ) ;
#8555 = B_SPLINE_CURVE_WITH_KNOTS ( 'NONE', 3,
 ( #11476, #44493, #26017, #41034, #44994, #14898, #29222, #44258, #11241, #7065 ),
 .UNSPECIFIED., .F., .F.,
 ( 4, 2, 2, 2, 4 ),
 ( 0.000000000000000000, 0.2500000000000000000, 0.5000000000000000000, 0.7500000000000000000, 1.000000000000000000 ),
 .UNSPECIFIED. ) ;
#8556 = ORIENTED_EDGE ( 'NONE', *, *, #46016, .T. ) ;
#8557 = DIRECTION ( 'NONE',  ( -3.071710424422018668E-17, 6.404604876783312462E-16, 1.000000000000000000 ) ) ;
#8558 = AXIS2_PLACEMENT_3D ( 'NONE', #31842, #32792, #36247 ) ;
#8559 = AXIS2_PLACEMENT_3D ( 'NONE', #41362, #3954, #30551 ) ;
#8560 = CARTESIAN_POINT ( 'NONE',  ( -22.05250757621314150, -8.971161105938598723, 63.33007234022110055 ) ) ;
#8561 = ADVANCED_FACE ( 'NONE', ( #16245 ), #34487, .T. ) ;
#8562 = CARTESIAN_POINT ( 'NONE',  ( -20.60192465206874246, -18.25372010660273148, 52.02966884056656482 ) ) ;
#8563 = ORIENTED_EDGE ( 'NONE', *, *, #17663, .F. ) ;
#8564 = AXIS2_PLACEMENT_3D ( 'NONE', #43464, #6016, #2801 ) ;
#8565 = CARTESIAN_POINT ( 'NONE',  ( -15.11195830621016256, -21.41632612911037370, 65.40596681519618016 ) ) ;
#8566 = B_SPLINE_CURVE_WITH_KNOTS ( 'NONE', 3,
 ( #21232, #40186, #13092, #6458, #32322, #1791, #6209, #43412, #24693, #20512 ),
 .UNSPECIFIED., .F., .F.,
 ( 4, 2, 2, 2, 4 ),
 ( 0.000000000000000000, 0.2500000000000000000, 0.5000000000000000000, 0.7500000000000000000, 1.000000000000000000 ),
 .UNSPECIFIED. ) ;
#8567 = FACE_OUTER_BOUND ( 'NONE', #16879, .T. ) ;
#8568 = CARTESIAN_POINT ( 'NONE',  ( -14.95535764022100977, -18.80681796222810576, 49.52966884056656482 ) ) ;
#8569 = VERTEX_POINT ( 'NONE', #27597 ) ;
#8570 = CARTESIAN_POINT ( 'NONE',  ( -10.44216256679811217, -13.77595636612621988, 61.06254307272654813 ) ) ;
#8571 = VERTEX_POINT ( 'NONE', #23916 ) ;
#8572 = CARTESIAN_POINT ( 'NONE',  ( -11.08846142298070880, -18.82290330472913098, 47.99999999999994316 ) ) ;
#8573 = CARTESIAN_POINT ( 'NONE',  ( -11.79792992861738909, -18.97409303405279957, 71.98685885147807539 ) ) ;
#8575 = EDGE_CURVE ( 'NONE', #39260, #37877, #15018, .T. ) ;
#8574 = ORIENTED_EDGE ( 'NONE', *, *, #23587, .F. ) ;
#8576 = FACE_OUTER_BOUND ( 'NONE', #11668, .T. ) ;
#8577 = CARTESIAN_POINT ( 'NONE',  ( -24.22593759466564123, -12.94379566627669753, 70.18731784193515466 ) ) ;
#8578 = CARTESIAN_POINT ( 'NONE',  ( -22.10120296142702045, -17.19398125327358073, 50.77966884056655772 ) ) ;
#8579 = ADVANCED_FACE ( 'NONE', ( #13525 ), #24645, .T. ) ;
#8580 = ORIENTED_EDGE ( 'NONE', *, *, #23244, .F. ) ;
#8581 = CARTESIAN_POINT ( 'NONE',  ( -11.12219343327886811, -17.98741664779230121, 71.72285496256920112 ) ) ;
#8582 =( BOUNDED_CURVE ( )  B_SPLINE_CURVE ( 3, ( #30578, #19234, #34236, #41891 ),
 .UNSPECIFIED., .F., .F. ) 
 B_SPLINE_CURVE_WITH_KNOTS ( ( 4, 4 ),
 ( 1.570796326794896780, 1.780235837034204183 ),
 .UNSPECIFIED. ) 
 CURVE ( )  GEOMETRIC_REPRESENTATION_ITEM ( )  RATIONAL_B_SPLINE_CURVE ( ( 1.000000000000000000, 0.9963479302455159337, 0.9963479302455159337, 1.000000000000000000 ) ) 
 REPRESENTATION_ITEM ( '' )  );
#8583 = FACE_OUTER_BOUND ( 'NONE', #2196, .T. ) ;
#8584 = FACE_OUTER_BOUND ( 'NONE', #38452, .T. ) ;
#8585 = CARTESIAN_POINT ( 'NONE',  ( -12.00450496360434727, -9.697323582995780455, 60.66643917381700390 ) ) ;
#8586 = EDGE_LOOP ( 'NONE', ( #35722, #24033, #36198, #46208, #26997 ) ) ;
#8587 = CARTESIAN_POINT ( 'NONE',  ( -10.63676228191995321, -11.73759119428953390, 74.65865931763289609 ) ) ;
#8588 = CARTESIAN_POINT ( 'NONE',  ( -24.72694767484942702, -16.28301260341204326, 62.70833288210281609 ) ) ;
#8589 = VERTEX_POINT ( 'NONE', #39645 ) ;
#8590 = ORIENTED_EDGE ( 'NONE', *, *, #7438, .F. ) ;
#8591 = CARTESIAN_POINT ( 'NONE',  ( -10.49233462046909793, -15.78425219969246562, 61.22892196979352519 ) ) ;
#8592 = CARTESIAN_POINT ( 'NONE',  ( -10.57990114081760957, -13.11695186304741334, 71.22300718686659593 ) ) ;
#8594 = CARTESIAN_POINT ( 'NONE',  ( -10.37739347266510670, -15.12138602804827414, 75.00598708744817600 ) ) ;
#8593 = VECTOR ( 'NONE', #35755, 1000.000000000000000 ) ;
#8595 = CARTESIAN_POINT ( 'NONE',  ( -22.41159385650551528, -6.922745924619793101, 51.69366785382590024 ) ) ;
#8596 = LINE ( 'NONE', #4907, #3810 ) ;
#8597 = PRODUCT_DEFINITION_FORMATION_WITH_SPECIFIED_SOURCE ( 'ANY', '', #33845, .NOT_KNOWN. ) ;
#8598 = CARTESIAN_POINT ( 'NONE',  ( -17.42409385541299471, -14.80920654474435594, 52.02966884056656482 ) ) ;
#8599 = CARTESIAN_POINT ( 'NONE',  ( -19.77436091090941517, -21.87886160397694368, 65.64981624214608757 ) ) ;
#8600 =( BOUNDED_CURVE ( )  B_SPLINE_CURVE ( 2, ( #4355, #42757, #20095, #19363, #1132, #9025, #45962, #24046, #34864 ),
 .UNSPECIFIED., .F., .F. ) 
 B_SPLINE_CURVE_WITH_KNOTS ( ( 3, 2, 2, 2, 3 ),
 ( 0.5833333333333332593, 0.5937499999999998890, 0.6041666666666665186, 0.6145833333333332593, 0.6249999999999998890 ),
 .UNSPECIFIED. ) 
 CURVE ( )  GEOMETRIC_REPRESENTATION_ITEM ( )  RATIONAL_B_SPLINE_CURVE ( ( 1.000000000000000888, 0.9238795325112859613, 1.000000000000000000, 0.9238795325112867385, 1.000000000000000000, 0.9238795325112867385, 1.000000000000000000, 0.9238795325112875156, 0.9999999999999992228 ) ) 
 REPRESENTATION_ITEM ( '' )  );
#8601 = VECTOR ( 'NONE', #30338, 1000.000000000000000 ) ;
#8602 = CIRCLE ( 'NONE', #48692, 0.5560000000000009379 ) ;
#8603 = ADVANCED_FACE ( 'NONE', ( #21183 ), #5916, .T. ) ;
#8604 = CARTESIAN_POINT ( 'NONE',  ( -23.70711844648210942, -18.01498993332871734, 59.09558460557502713 ) ) ;
#8605 = ORIENTED_EDGE ( 'NONE', *, *, #10303, .F. ) ;
#8606 = ORIENTED_EDGE ( 'NONE', *, *, #38145, .F. ) ;
#8607 = CARTESIAN_POINT ( 'NONE',  ( -12.35277332135121675, -20.26681466537264242, 68.45162004874669037 ) ) ;
#8608 = EDGE_CURVE ( 'NONE', #14812, #9213, #25827, .T. ) ;
#8609 = EDGE_CURVE ( 'NONE', #23558, #24381, #19384, .T. ) ;
#8610 = CARTESIAN_POINT ( 'NONE',  ( -13.65110163016468015, -21.23324793748626504, 68.57129851394472553 ) ) ;
#8611 = CIRCLE ( 'NONE', #21151, 1.500000000000008216 ) ;
#8612 = DIRECTION ( 'NONE',  ( 1.000000000000000000, 2.866981220435666553E-17, 0.000000000000000000 ) ) ;
#8613 = CARTESIAN_POINT ( 'NONE',  ( -14.88240180108872934, -21.38896689746768587, 65.19776689114348756 ) ) ;
#8614 = VERTEX_POINT ( 'NONE', #40138 ) ;
#8615 =( BOUNDED_SURFACE ( )  B_SPLINE_SURFACE ( 3, 1, ( 
 ( #37245, #37991 ),
 ( #33547, #48592 ),
 ( #14826, #29896 ),
 ( #11409, #14260 ),
 ( #48024, #40390 ),
 ( #29310, #40619 ),
 ( #9220, #46652 ) ),
 .UNSPECIFIED., .T., .F., .F. ) 
 B_SPLINE_SURFACE_WITH_KNOTS ( ( 4, 3, 4 ),
 ( 2, 2 ),
 ( 0.000000000000000000, 0.5000000000000000000, 1.000000000000000000 ),
 ( 0.000000000000000000, 1.000000000000000000 ),
 .UNSPECIFIED. ) 
 GEOMETRIC_REPRESENTATION_ITEM ( )  RATIONAL_B_SPLINE_SURFACE ( (
 ( 1.000000000000000000, 1.000000000000000000),
 ( 0.3333333333333335369, 0.3333333333333330373),
 ( 0.3333333333333335369, 0.3333333333333330373),
 ( 1.000000000000000000, 1.000000000000000000),
 ( 0.3333333333333333703, 0.3333333333333333703),
 ( 0.3333333333333333703, 0.3333333333333333703),
 ( 1.000000000000000000, 1.000000000000000000) ) ) 
 REPRESENTATION_ITEM ( '' )  SURFACE ( )  );
#8616 = ADVANCED_FACE ( 'NONE', ( #39887 ), #16735, .T. ) ;
#8617 = EDGE_CURVE ( 'NONE', #15782, #43774, #1521, .T. ) ;
#8618 = VERTEX_POINT ( 'NONE', #43600 ) ;
#8619 = DIRECTION ( 'NONE',  ( 0.9979768094191902028, 0.06357898915123888495, 3.501668460141639105E-17 ) ) ;
#8620 = CARTESIAN_POINT ( 'NONE',  ( -23.42915847708036381, -11.11517115755410146, 73.64721174900437006 ) ) ;
#8621 = CARTESIAN_POINT ( 'NONE',  ( -15.61430862894485649, -21.57127090070544639, 72.11863486128041245 ) ) ;
#8622 = CARTESIAN_POINT ( 'NONE',  ( -23.34481640033245853, -18.63641755246779752, 69.59371984262205046 ) ) ;
#8623 = ORIENTED_EDGE ( 'NONE', *, *, #40310, .T. ) ;
#8624 = CARTESIAN_POINT ( 'NONE',  ( -20.82033344162761423, -20.98728273936873734, 62.11471416939660628 ) ) ;
#8625 = CARTESIAN_POINT ( 'NONE',  ( -12.74138925215518015, -14.62063335304397427, 49.52966884056655772 ) ) ;
#8626 = EDGE_CURVE ( 'NONE', #11402, #28884, #32501, .T. ) ;
#8627 = ORIENTED_EDGE ( 'NONE', *, *, #35831, .F. ) ;
#8628 = CARTESIAN_POINT ( 'NONE',  ( -22.04114742393716142, -9.481025248639417313, 59.73643293354757589 ) ) ;
#8629 = CARTESIAN_POINT ( 'NONE',  ( -22.14599171854093740, -19.97736010173111509, 65.72038334521670322 ) ) ;
#8630 = ORIENTED_EDGE ( 'NONE', *, *, #26631, .F. ) ;
#8631 = PLANE ( 'NONE',  #37741 ) ;
#8632 = VECTOR ( 'NONE', #20706, 1000.000000000000000 ) ;
#8633 = ORIENTED_EDGE ( 'NONE', *, *, #6938, .F. ) ;
#8634 = CARTESIAN_POINT ( 'NONE',  ( -14.07539661982785262, -8.605278201040592378, 74.34954655214895070 ) ) ;
#8635 = DIRECTION ( 'NONE',  ( 1.224646799147353207E-16, 1.000000000000000000, -1.912410701131276611E-32 ) ) ;
#8636 = VERTEX_POINT ( 'NONE', #20461 ) ;
#8637 = CARTESIAN_POINT ( 'NONE',  ( -24.23636321612255173, -17.82529083293033167, 62.58865660992282898 ) ) ;
#8638 = EDGE_CURVE ( 'NONE', #13744, #29820, #10095, .T. ) ;
#8639 = CARTESIAN_POINT ( 'NONE',  ( -15.83034385541288991, -6.857644439847648599, 49.98602051094142951 ) ) ;
#8640 = CARTESIAN_POINT ( 'NONE',  ( -17.66159385650551528, -9.295667164867525756, 49.30633214617472504 ) ) ;
#8641 = CIRCLE ( 'NONE', #19636, 1.999999999999999334 ) ;
#8642 = DIRECTION ( 'NONE',  ( -0.9687793358424819923, 0.2479245821708680464, 0.000000000000000000 ) ) ;
#8643 = CARTESIAN_POINT ( 'NONE',  ( -15.10203878652056630, -21.46900354431040725, 61.52111843893123933 ) ) ;
#8644 = VERTEX_POINT ( 'NONE', #1974 ) ;
#8645 = CARTESIAN_POINT ( 'NONE',  ( -19.08084885026315902, -21.61197540051820454, 58.71434541541806595 ) ) ;
#8646 = CARTESIAN_POINT ( 'NONE',  ( -11.42962537269896117, -10.38539323336976494, 74.62380298385740218 ) ) ;
#8647 = FACE_OUTER_BOUND ( 'NONE', #31555, .T. ) ;
#8648 = CARTESIAN_POINT ( 'NONE',  ( -20.50090549915545424, -8.024104330060138679, 66.95820990016825647 ) ) ;
#8649 = LINE ( 'NONE', #38913, #37249 ) ;
#8650 = VERTEX_POINT ( 'NONE', #31777 ) ;
#8651 = EDGE_LOOP ( 'NONE', ( #36103, #29902 ) ) ;
#8652 = APPLICATION_CONTEXT ( 'automotive_design' ) ;
#8653 = CARTESIAN_POINT ( 'NONE',  ( -21.33694788700791278, -9.004934622526002741, 73.60128753634342047 ) ) ;
#8654 = CYLINDRICAL_SURFACE ( 'NONE', #6135, 0.1500000000000034084 ) ;
#8655 = VERTEX_POINT ( 'NONE', #13277 ) ;
#8656 = CARTESIAN_POINT ( 'NONE',  ( -22.18998830427771196, -20.00468049915955859, 65.71893796558269685 ) ) ;
#8657 = CARTESIAN_POINT ( 'NONE',  ( -24.04530722081856453, -17.24086825362277509, 66.15177283638185202 ) ) ;
#8658 = CARTESIAN_POINT ( 'NONE',  ( -22.33034385759799179, -6.857644439848013640, 49.98602051094139398 ) ) ;
#8659 = CARTESIAN_POINT ( 'NONE',  ( -17.35131678204048455, -7.807977840370839751, 70.67962813217452833 ) ) ;
#8660 = CARTESIAN_POINT ( 'NONE',  ( -14.61306878872958137, -8.340592061241681066, 67.67463703838096478 ) ) ;
#8661 = CARTESIAN_POINT ( 'NONE',  ( -26.42409385541305511, -15.80920654474410725, 47.99999999999997868 ) ) ;
#8662 = DIRECTION ( 'NONE',  ( -3.071710424422018668E-17, 6.404604876783312462E-16, 1.000000000000000000 ) ) ;
#8663 = EDGE_LOOP ( 'NONE', ( #18675, #13790, #34368, #16394, #12354 ) ) ;
#8664 = DIRECTION ( 'NONE',  ( 1.000000000000000000, 0.000000000000000000, 0.000000000000000000 ) ) ;
#8665 = EDGE_CURVE ( 'NONE', #1976, #9242, #1823, .T. ) ;
#8666 = CARTESIAN_POINT ( 'NONE',  ( -19.21561283247386598, -21.62782285876819088, 58.52507411012581429 ) ) ;
#8667 = VECTOR ( 'NONE', #7666, 1000.000000000000114 ) ;
#8668 = VECTOR ( 'NONE', #37663, 1000.000000000000114 ) ;
#8669 = CARTESIAN_POINT ( 'NONE',  ( -10.23610968374255314, -12.85046669463587143, 67.85336945107273721 ) ) ;
#8670 = CARTESIAN_POINT ( 'NONE',  ( -14.13242279744181573, -8.574497162196568212, 74.21426705364891063 ) ) ;
#8671 = AXIS2_PLACEMENT_3D ( 'NONE', #32630, #36776, #28694 ) ;
#8672 = ORIENTED_EDGE ( 'NONE', *, *, #217, .F. ) ;
#8673 = ORIENTED_EDGE ( 'NONE', *, *, #15396, .F. ) ;
#8674 = EDGE_CURVE ( 'NONE', #2631, #28641, #13042, .T. ) ;
#8675 = CARTESIAN_POINT ( 'NONE',  ( -22.74909385650551386, -8.104110260919577868, 48.81699501597546487 ) ) ;
#8676 = EDGE_CURVE ( 'NONE', #18372, #34964, #35463, .T. ) ;
#8677 = ORIENTED_EDGE ( 'NONE', *, *, #2717, .T. ) ;
#8678 = CARTESIAN_POINT ( 'NONE',  ( -11.56806251476610115, -18.73522173559940995, 65.03234934376791898 ) ) ;
#8679 = EDGE_CURVE ( 'NONE', #32808, #5810, #48004, .T. ) ;
#8680 = CARTESIAN_POINT ( 'NONE',  ( -16.39888349198502127, -21.73372412438269308, 62.05568132716130236 ) ) ;
#8681 = AXIS2_PLACEMENT_3D ( 'NONE', #42582, #30280, #15711 ) ;
#8682 = EDGE_CURVE ( 'NONE', #48460, #15180, #44092, .T. ) ;
#8683 = ORIENTED_EDGE ( 'NONE', *, *, #26599, .T. ) ;
#8684 = CARTESIAN_POINT ( 'NONE',  ( -10.79572390357762046, -11.40795830647630282, 67.80360014157953685 ) ) ;
#8685 = CARTESIAN_POINT ( 'NONE',  ( -10.40860991809309155, -15.50898095412354571, 57.85320721669017985 ) ) ;
#8686 = EDGE_CURVE ( 'NONE', #29406, #33012, #26992, .T. ) ;
#8687 = CLOSED_SHELL ( 'NONE', ( #32829, #20110, #31688, #6131, #45936, #24247, #286, #5 ) ) ;
#8688 = ORIENTED_EDGE ( 'NONE', *, *, #45753, .T. ) ;
#8689 = CARTESIAN_POINT ( 'NONE',  ( -23.90062161048602363, -17.60374255572093816, 59.00378367634043997 ) ) ;
#8690 =( BOUNDED_CURVE ( )  B_SPLINE_CURVE ( 3, ( #45505, #14935, #26786, #3896 ),
 .UNSPECIFIED., .F., .F. ) 
 B_SPLINE_CURVE_WITH_KNOTS ( ( 4, 4 ),
 ( 0.4074455897393590154, 0.5000000000000000000 ),
 .UNSPECIFIED. ) 
 CURVE ( )  GEOMETRIC_REPRESENTATION_ITEM ( )  RATIONAL_B_SPLINE_CURVE ( ( 0.6983129098260651979, 0.7760317562606895425, 0.8765941196520058432, 1.000000000000024647 ) ) 
 REPRESENTATION_ITEM ( '' )  );
#8691 = CARTESIAN_POINT ( 'NONE',  ( -23.04367355717579358, -10.55211556811382678, 59.90203429191419104 ) ) ;
#8692 = ORIENTED_EDGE ( 'NONE', *, *, #553, .T. ) ;
#8693 = CARTESIAN_POINT ( 'NONE',  ( -19.83852420082105894, -21.85790785478787868, 69.12137763959520953 ) ) ;
#8694 = CARTESIAN_POINT ( 'NONE',  ( -17.39742496553465756, -7.759256980052345654, 67.02039592192092243 ) ) ;
#8695 = ORIENTED_EDGE ( 'NONE', *, *, #11564, .T. ) ;
#8696 = DIRECTION ( 'NONE',  ( 2.775557561562888984E-15, 0.000000000000000000, -1.000000000000000000 ) ) ;
#8697 = DIRECTION ( 'NONE',  ( 0.7506333037770491767, -0.6607190350373993715, 0.000000000000000000 ) ) ;
#8698 = CARTESIAN_POINT ( 'NONE',  ( -17.23693881351924517, -7.361390637904862366, 70.65182322704724527 ) ) ;
#8699 = ORIENTED_EDGE ( 'NONE', *, *, #23779, .F. ) ;
#8700 = DIRECTION ( 'NONE',  ( -3.071710424422018668E-17, 6.404604876783312462E-16, 1.000000000000000000 ) ) ;
#8701 = CARTESIAN_POINT ( 'NONE',  ( -15.53265176333180619, -21.60105060138385014, 72.33103357390284316 ) ) ;
#8702 = VECTOR ( 'NONE', #25346, 1000.000000000000000 ) ;
#8703 = DIRECTION ( 'NONE',  ( 1.000000000000000000, 1.669677910507523057E-21, 6.493791346278465266E-22 ) ) ;
#8704 = DIRECTION ( 'NONE',  ( 0.000000000000000000, 1.000000000000000000, -3.469446951953614189E-15 ) ) ;
#8705 = CARTESIAN_POINT ( 'NONE',  ( -50.42409385541304800, -15.80920654474410725, 56.99999999999999289 ) ) ;
#8706 = VECTOR ( 'NONE', #17664, 999.9999999999998863 ) ;
#8707 = CARTESIAN_POINT ( 'NONE',  ( -20.23440041452680660, -8.343390979720714640, 70.25660101728180962 ) ) ;
#8708 = DIRECTION ( 'NONE',  ( -1.061592179903616477E-06, -3.103086884670442514E-06, 0.9999999999946218576 ) ) ;
#8709 = CARTESIAN_POINT ( 'NONE',  ( -17.81896166628845180, -7.766655581923772367, 63.64237022204054028 ) ) ;
#8710 = CARTESIAN_POINT ( 'NONE',  ( -10.45863924090583552, -14.11462608630872317, 61.21821294130609914 ) ) ;
#8711 = CARTESIAN_POINT ( 'NONE',  ( -14.48034385650551847, -6.424090610841176385, 49.80797279389978627 ) ) ;
#8712 = EDGE_LOOP ( 'NONE', ( #42634, #29654, #16805, #9133, #24631 ) ) ;
#8713 = CARTESIAN_POINT ( 'NONE',  ( -12.77013062424865630, -8.927826924028673616, 47.99999999999994316 ) ) ;
#8714 = CYLINDRICAL_SURFACE ( 'NONE', #22630, 0.5000000000000004441 ) ;
#8715 = VERTEX_POINT ( 'NONE', #17939 ) ;
#8716 = CARTESIAN_POINT ( 'NONE',  ( -20.02409385759798965, -9.359200813967568422, 50.49621490985803263 ) ) ;
#8717 = CARTESIAN_POINT ( 'NONE',  ( -15.00426899868425856, -21.85539911116967104, 65.28313592555664968 ) ) ;
#8718 = CIRCLE ( 'NONE', #27572, 6.899999999999997691 ) ;
#8719 = CARTESIAN_POINT ( 'NONE',  ( -10.60920434360279074, -17.81927616673939596, 71.76056483618631887 ) ) ;
#8720 = CARTESIAN_POINT ( 'NONE',  ( -50.42609385541305755, -14.80920654474424225, 70.07647058823528141 ) ) ;
#8721 = CARTESIAN_POINT ( 'NONE',  ( -14.67456124858633615, -21.24707893775024203, 58.18234469924885133 ) ) ;
#8722 = EDGE_CURVE ( 'NONE', #35691, #26935, #15256, .T. ) ;
#8723 = ORIENTED_EDGE ( 'NONE', *, *, #45646, .F. ) ;
#8724 = CARTESIAN_POINT ( 'NONE',  ( -23.76058118794394503, -11.83148257926706393, 63.02388499825810442 ) ) ;
#8725 = DIRECTION ( 'NONE',  ( -0.3037135924646501839, 0.9527633776296273727, 2.170275161112374231E-08 ) ) ;
#8726 = CARTESIAN_POINT ( 'NONE',  ( -23.99668814781213300, -11.30145868231390338, 66.61488666845116313 ) ) ;
#8727 = EDGE_CURVE ( 'NONE', #2574, #48564, #20374, .T. ) ;
#8728 = ORIENTED_EDGE ( 'NONE', *, *, #1361, .F. ) ;
#8729 = AXIS2_PLACEMENT_3D ( 'NONE', #17007, #13080, #5955 ) ;
#8730 = FACE_OUTER_BOUND ( 'NONE', #5215, .T. ) ;
#8731 = CARTESIAN_POINT ( 'NONE',  ( -24.39160045767772544, -17.44704251381193316, 69.59152525453608007 ) ) ;
#8732 = CARTESIAN_POINT ( 'NONE',  ( -41.53953503188365204, -14.80920654474424225, 70.07647058823528141 ) ) ;
#8733 = CARTESIAN_POINT ( 'NONE',  ( -17.42409385541299471, -14.80920654474435594, 52.02966884056656482 ) ) ;
#8734 = CARTESIAN_POINT ( 'NONE',  ( -21.01123855637963089, -20.87838213191899683, 65.58453944497207999 ) ) ;
#8735 = VERTEX_POINT ( 'NONE', #30038 ) ;
#8736 = ORIENTED_EDGE ( 'NONE', *, *, #25231, .F. ) ;
#8737 = CARTESIAN_POINT ( 'NONE',  ( -22.74909385541304019, -8.112991634885936776, 51.74999426922421719 ) ) ;
#8738 = VECTOR ( 'NONE', #17603, 1000.000000000000114 ) ;
#8739 = CARTESIAN_POINT ( 'NONE',  ( -19.88526343185200673, -21.36290080982552553, 72.42701748270100381 ) ) ;
#8740 = ADVANCED_FACE ( 'NONE', ( #32732 ), #37317, .T. ) ;
#8741 = VECTOR ( 'NONE', #16373, 999.9999999999998863 ) ;
#8742 = CARTESIAN_POINT ( 'NONE',  ( -22.01964724813734620, -15.72799447708766607, 52.02966884056656482 ) ) ;
#8743 = ADVANCED_FACE ( 'NONE', ( #21894 ), #26091, .T. ) ;
#8744 =( BOUNDED_SURFACE ( )  B_SPLINE_SURFACE ( 3, 1, ( 
 ( #37216, #15057 ),
 ( #30600, #45624 ),
 ( #26404, #3500 ),
 ( #37459, #19492 ),
 ( #41415, #30115 ),
 ( #26902, #34507 ),
 ( #3751, #18766 ) ),
 .UNSPECIFIED., .T., .F., .F. ) 
 B_SPLINE_SURFACE_WITH_KNOTS ( ( 4, 3, 4 ),
 ( 2, 2 ),
 ( 0.000000000000000000, 0.5000000000000000000, 1.000000000000000000 ),
 ( 0.000000000000000000, 1.000000000000000000 ),
 .UNSPECIFIED. ) 
 GEOMETRIC_REPRESENTATION_ITEM ( )  RATIONAL_B_SPLINE_SURFACE ( (
 ( 1.000000000000000000, 1.000000000000000000),
 ( 0.3333333333333335369, 0.3333333333333330373),
 ( 0.3333333333333335369, 0.3333333333333330373),
 ( 1.000000000000000000, 1.000000000000000000),
 ( 0.3333333333333333703, 0.3333333333333333703),
 ( 0.3333333333333333703, 0.3333333333333333703),
 ( 1.000000000000000000, 1.000000000000000000) ) ) 
 REPRESENTATION_ITEM ( '' )  SURFACE ( )  );
#8745 = VECTOR ( 'NONE', #42043, 1000.000000000000000 ) ;
#8746 = PRODUCT ( 'Base Cast Iron Chassis Plate', 'Base Cast Iron Chassis Plate', '', ( #38049 ) ) ;
#8747 = ADVANCED_FACE ( 'NONE', ( #14709 ), #41100, .F. ) ;
#8748 = DIRECTION ( 'NONE',  ( -3.071710424422018668E-17, 6.404604876783312462E-16, 1.000000000000000000 ) ) ;
#8749 = FACE_OUTER_BOUND ( 'NONE', #4212, .T. ) ;
#8750 = CIRCLE ( 'NONE', #29975, 4.686499999999998778 ) ;
#8751 = CARTESIAN_POINT ( 'NONE',  ( -24.26499789074519597, -17.75976756996305639, 62.65856417960095825 ) ) ;
#8752 = ADVANCED_FACE ( 'NONE', ( #47756 ), #13993, .T. ) ;
#8753 = ORIENTED_EDGE ( 'NONE', *, *, #13321, .T. ) ;
#8754 =( BOUNDED_CURVE ( )  B_SPLINE_CURVE ( 3, ( #1466, #46555, #20443, #21354 ),
 .UNSPECIFIED., .F., .F. ) 
 B_SPLINE_CURVE_WITH_KNOTS ( ( 4, 4 ),
 ( 0.4074455897393638448, 0.5000000000000000000 ),
 .UNSPECIFIED. ) 
 CURVE ( )  GEOMETRIC_REPRESENTATION_ITEM ( )  RATIONAL_B_SPLINE_CURVE ( ( 0.6983129098261096068, 0.7760317562607167430, 0.8765941196520149470, 1.000000000000006883 ) ) 
 REPRESENTATION_ITEM ( '' )  );
#8755 = CARTESIAN_POINT ( 'NONE',  ( -12.84719963800786502, -9.512789006345032661, 74.31923006385322594 ) ) ;
#8756 = EDGE_LOOP ( 'NONE', ( #33372, #40660, #13366, #18822, #45939 ) ) ;
#8757 = CARTESIAN_POINT ( 'NONE',  ( -10.72530867274958233, -17.00760959713300480, 57.97288447305808745 ) ) ;
#8758 = CYLINDRICAL_SURFACE ( 'NONE', #12411, 5.249999999999998224 ) ;
#8759 = ORIENTED_EDGE ( 'NONE', *, *, #26530, .T. ) ;
#8760 = CARTESIAN_POINT ( 'NONE',  ( -13.25841313310420766, -9.121485346447943954, 64.20946499508677618 ) ) ;
#8761 = B_SPLINE_CURVE_WITH_KNOTS ( 'NONE', 3,
 ( #40455, #14325, #47850, #14558, #29380, #3508, #10195, #10437, #14806, #40945 ),
 .UNSPECIFIED., .F., .F.,
 ( 4, 2, 2, 2, 4 ),
 ( 0.6272669072878209739, 0.7522669073073412482, 0.8772669073268615225, 1.002266907346381686, 1.127266907365902071 ),
 .UNSPECIFIED. ) ;
#8762 = CARTESIAN_POINT ( 'NONE',  ( -19.57409385759799036, -6.859212275519751323, 50.50378509014259265 ) ) ;
#8763 = CARTESIAN_POINT ( 'NONE',  ( -20.03377823521572765, -8.313858397182363191, 70.44203619096923319 ) ) ;
#8764 = CARTESIAN_POINT ( 'NONE',  ( -20.88906156096523148, -8.213963083740734916, 59.94786934217235341 ) ) ;
#8765 = ORIENTED_EDGE ( 'NONE', *, *, #5531, .F. ) ;
#8766 = CARTESIAN_POINT ( 'NONE',  ( -21.89130958583942288, -9.354787850460871468, 63.20625856529903075 ) ) ;
#8767 = CARTESIAN_POINT ( 'NONE',  ( -24.44055745662519641, -14.11932379769929113, 73.13743607903229815 ) ) ;
#8768 = FACE_OUTER_BOUND ( 'NONE', #45115, .T. ) ;
#8769 = CARTESIAN_POINT ( 'NONE',  ( -18.39951368268757648, -22.19516171751901368, 69.00010101991060196 ) ) ;
#8770 = DIRECTION ( 'NONE',  ( 1.000000000000000000, 0.000000000000000000, 0.000000000000000000 ) ) ;
#8771 = VECTOR ( 'NONE', #42344, 1000.000000000000000 ) ;
#8772 = CARTESIAN_POINT ( 'NONE',  ( -20.66696756681432490, -21.06910030335248152, 58.64475164910062688 ) ) ;
#8773 = CARTESIAN_POINT ( 'NONE',  ( -23.46260529264823447, -11.17067950781535579, 73.36193301757424479 ) ) ;
#8774 = DIRECTION ( 'NONE',  ( 0.7150252244155715919, -0.6990986543038554268, 7.133781456731073326E-17 ) ) ;
#8775 = EDGE_LOOP ( 'NONE', ( #26304, #9937, #24320, #18513 ) ) ;
#8776 = FACE_OUTER_BOUND ( 'NONE', #7932, .T. ) ;
#8777 = ORIENTED_EDGE ( 'NONE', *, *, #31906, .T. ) ;
#8778 = LINE ( 'NONE', #5077, #25079 ) ;
#8779 = CARTESIAN_POINT ( 'NONE',  ( -13.26878139971602621, -9.173971005569262260, 67.56869938284187072 ) ) ;
#8780 = EDGE_CURVE ( 'NONE', #6936, #47492, #4649, .T. ) ;
#8781 = EDGE_LOOP ( 'NONE', ( #5908, #43495 ) ) ;
#8782 = AXIS2_PLACEMENT_3D ( 'NONE', #2959, #26118, #44354 ) ;
#8783 = DIRECTION ( 'NONE',  ( -0.7506333037770542838, 0.6607190350373937093, 0.000000000000000000 ) ) ;
#8784 = FACE_BOUND ( 'NONE', #28335, .T. ) ;
#8785 = ORIENTED_EDGE ( 'NONE', *, *, #36642, .T. ) ;
#8786 = ORIENTED_EDGE ( 'NONE', *, *, #39724, .F. ) ;
#8787 = ORIENTED_EDGE ( 'NONE', *, *, #23943, .T. ) ;
#8788 = CARTESIAN_POINT ( 'NONE',  ( -10.99582178678916833, -11.91441492378913658, 74.85840195586327184 ) ) ;
#8789 = VECTOR ( 'NONE', #7713, 1000.000000000000227 ) ;
#8790 = CARTESIAN_POINT ( 'NONE',  ( -21.84909385541302029, -8.112991634885936776, 51.74999426922424561 ) ) ;
#8791 = DIRECTION ( 'NONE',  ( -2.866981220435666553E-17, 1.000000000000000000, 1.190614954331866791E-16 ) ) ;
#8792 = CARTESIAN_POINT ( 'NONE',  ( -14.58386025153609467, -8.409552409253036487, 67.44902071755305428 ) ) ;
#8793 = CARTESIAN_POINT ( 'NONE',  ( -21.12516169987187098, -20.80993955427394582, 69.06922321213187388 ) ) ;
#8794 = CARTESIAN_POINT ( 'NONE',  ( -13.43328788299345966, -9.058103587765096165, 60.73950223935946013 ) ) ;
#8795 = VERTEX_POINT ( 'NONE', #34185 ) ;
#8796 = VERTEX_POINT ( 'NONE', #45543 ) ;
#8797 = CARTESIAN_POINT ( 'NONE',  ( -22.04909385650551457, -8.104110260919577868, 48.81699501597546487 ) ) ;
#8798 = ADVANCED_FACE ( 'NONE', ( #3929 ), #7874, .T. ) ;
#8799 = B_SPLINE_CURVE_WITH_KNOTS ( 'NONE', 3,
 ( #44166, #43671, #44626, #44387, #25424, #10416, #25653, #10884, #3001, #2285 ),
 .UNSPECIFIED., .F., .F.,
 ( 4, 2, 2, 2, 4 ),
 ( 0.6272669072877721241, 0.7522669073073040558, 0.8772669073268360984, 1.002266907346368141, 1.127266907365900073 ),
 .UNSPECIFIED. ) ;
#8800 = PLANE ( 'NONE',  #46466 ) ;
#8801 = CARTESIAN_POINT ( 'NONE',  ( -21.62013776805207854, -9.204234041992926052, 70.32059703345998969 ) ) ;
#8802 = ORIENTED_EDGE ( 'NONE', *, *, #22750, .T. ) ;
#8803 = CARTESIAN_POINT ( 'NONE',  ( -22.55534385650551599, -7.417179338643134834, 52.18511593390279302 ) ) ;
#8804 = EDGE_LOOP ( 'NONE', ( #48377, #7087, #34679, #24510, #4994 ) ) ;
#8805 = ADVANCED_FACE ( 'NONE', ( #30768 ), #16191, .T. ) ;
#8806 = VECTOR ( 'NONE', #25554, 1000.000000000000000 ) ;
#8807 = CARTESIAN_POINT ( 'NONE',  ( -23.02753331400065662, -10.61361262881353085, 59.60203474230917919 ) ) ;
#8808 = AXIS2_PLACEMENT_3D ( 'NONE', #27187, #30894, #16322 ) ;
#8809 = CARTESIAN_POINT ( 'NONE',  ( -17.26260884657101258, -7.811009669971855196, 67.09327729553568531 ) ) ;
#8810 = EDGE_CURVE ( 'NONE', #43519, #9620, #15955, .T. ) ;
#8811 = VERTEX_POINT ( 'NONE', #34425 ) ;
#8812 = CARTESIAN_POINT ( 'NONE',  ( -13.27770617114843965, -9.107455183738579763, 64.05946529205222362 ) ) ;
#8813 = CARTESIAN_POINT ( 'NONE',  ( -22.39254715322108780, -9.803279359720651343, 73.36672461330924477 ) ) ;
#8814 = CARTESIAN_POINT ( 'NONE',  ( -10.81230840161673790, -17.25685697075765646, 64.64211442681141762 ) ) ;
#8815 = CARTESIAN_POINT ( 'NONE',  ( -23.12302657392458016, -18.95946740514217765, 62.35406880581413702 ) ) ;
#8816 = ORIENTED_EDGE ( 'NONE', *, *, #5380, .T. ) ;
#8817 = CIRCLE ( 'NONE', #36309, 4.686499999999998778 ) ;
#8818 = DIRECTION ( 'NONE',  ( -0.5351595679979685993, -0.8447509909909710624, 0.000000000000000000 ) ) ;
#8819 = ADVANCED_FACE ( 'NONE', ( #1184 ), #43264, .F. ) ;
#8820 = DIRECTION ( 'NONE',  ( 0.5562740912439652075, 0.8309988781043535777, 7.851267780903551505E-08 ) ) ;
#8821 = CARTESIAN_POINT ( 'NONE',  ( -13.92409385541305511, -10.60920654474410618, 81.99999999999998579 ) ) ;
#8822 = ORIENTED_EDGE ( 'NONE', *, *, #27799, .T. ) ;
#8823 = CARTESIAN_POINT ( 'NONE',  ( -10.42930205768512941, -13.90492575851057211, 61.33310083575204885 ) ) ;
#8824 = EDGE_CURVE ( 'NONE', #46544, #12446, #18770, .T. ) ;
#8825 = ORIENTED_EDGE ( 'NONE', *, *, #48452, .T. ) ;
#8826 = CARTESIAN_POINT ( 'NONE',  ( -21.73098984888145679, -8.730191469543168381, 70.31627926275058371 ) ) ;
#8827 = CARTESIAN_POINT ( 'NONE',  ( -14.79922921121938195, -7.836842249070715916, 57.03495322699122738 ) ) ;
#8828 = EDGE_LOOP ( 'NONE', ( #13933, #28951, #33081, #35298 ) ) ;
#8829 = EDGE_CURVE ( 'NONE', #19901, #38378, #28800, .T. ) ;
#8830 = CARTESIAN_POINT ( 'NONE',  ( -14.90085577400961014, -10.20532018813695707, 49.52966884056655772 ) ) ;
#8831 = CARTESIAN_POINT ( 'NONE',  ( -21.79520202288280117, -20.27875078180004920, 58.95369995708556843 ) ) ;
#8832 = CARTESIAN_POINT ( 'NONE',  ( -24.24046477733709182, -13.21445941831622761, 63.11647676942984475 ) ) ;
#8833 = CARTESIAN_POINT ( 'NONE',  ( -17.42409385541299471, -14.80920654474435771, 49.52966884056655772 ) ) ;
#8834 = ORIENTED_EDGE ( 'NONE', *, *, #10716, .T. ) ;
#8835 = CARTESIAN_POINT ( 'NONE',  ( -24.14992870231961319, -18.01341063617936911, 59.11883102335588802 ) ) ;
#8836 = CARTESIAN_POINT ( 'NONE',  ( -20.64758834049123593, -8.594144569355316676, 63.38291771811893938 ) ) ;
#8837 = CARTESIAN_POINT ( 'NONE',  ( -23.12535539932854078, -10.01343808792704237, 66.65686846082743955 ) ) ;
#8838 = ORIENTED_EDGE ( 'NONE', *, *, #35557, .T. ) ;
#8839 = DIRECTION ( 'NONE',  ( 0.000000000000000000, -0.9999954153791273948, -0.003028072113819838245 ) ) ;
#8840 = CARTESIAN_POINT ( 'NONE',  ( -24.73606664458329263, -16.23668146098944831, 62.79317443719546787 ) ) ;
#8841 = ORIENTED_EDGE ( 'NONE', *, *, #27206, .T. ) ;
#8842 = ORIENTED_EDGE ( 'NONE', *, *, #7063, .T. ) ;
#8843 = CIRCLE ( 'NONE', #4902, 0.3999999999999978018 ) ;
#8844 = CARTESIAN_POINT ( 'NONE',  ( -22.78465872505329770, -10.30744173788789908, 66.54182281442142255 ) ) ;
#8845 = CARTESIAN_POINT ( 'NONE',  ( -13.44410990971816666, -8.986443949771105721, 64.32435409333248799 ) ) ;
#8846 = CARTESIAN_POINT ( 'NONE',  ( -10.42732927771101359, -14.54885032245585386, 71.43855692335705498 ) ) ;
#8847 = CARTESIAN_POINT ( 'NONE',  ( -12.72364782008763484, -9.064348897850818432, 49.69364828684970803 ) ) ;
#8848 = CARTESIAN_POINT ( 'NONE',  ( -15.47038452772150663, -21.58309165278561537, 72.04575460769355288 ) ) ;
#8849 = CARTESIAN_POINT ( 'NONE',  ( -22.51726247777427758, -19.68384842258191725, 72.94400547081133368 ) ) ;
#8850 = CARTESIAN_POINT ( 'NONE',  ( -41.79100562011894482, -14.80920654474422271, 68.06470588235292496 ) ) ;
#8851 = CARTESIAN_POINT ( 'NONE',  ( -24.40658499505740053, -15.78250870199476807, 69.83307488408829045 ) ) ;
#8852 = EDGE_LOOP ( 'NONE', ( #26050, #10541, #35046, #33401, #10688 ) ) ;
#8853 = ORIENTED_EDGE ( 'NONE', *, *, #11726, .F. ) ;
#8854 = CARTESIAN_POINT ( 'NONE',  ( -13.27161037900033058, -18.02158587759403829, 50.77966884056655772 ) ) ;
#8855 = CARTESIAN_POINT ( 'NONE',  ( 0.000000000000000000, 0.000000000000000000, 0.000000000000000000 ) ) ;
#8856 = CARTESIAN_POINT ( 'NONE',  ( -23.64864541627648009, -11.60591314845866684, 66.70597954916981109 ) ) ;
#8857 = CARTESIAN_POINT ( 'NONE',  ( -22.48114071483173149, -19.64927648862363796, 72.94400547034429394 ) ) ;
#8858 = CARTESIAN_POINT ( 'NONE',  ( -18.83585931754296183, -7.494105970839488151, 70.48572750873847781 ) ) ;
#8859 = VERTEX_POINT ( 'NONE', #37632 ) ;
#8860 = ADVANCED_FACE ( 'NONE', ( #959, #8117 ), #30526, .F. ) ;
#8861 = DIRECTION ( 'NONE',  ( 1.000000000000000000, 1.665334536937734564E-16, 1.927470528863183637E-16 ) ) ;
#8862 = CARTESIAN_POINT ( 'NONE',  ( -18.08884787034790875, -9.601462109806339740, 52.02966884056656482 ) ) ;
#8863 = DIRECTION ( 'NONE',  ( 0.7621627669932626858, -0.6473854467078885566, 3.680865982637999709E-08 ) ) ;
#8864 = CARTESIAN_POINT ( 'NONE',  ( -11.10069974846098262, -18.74849293576752984, 61.46984965132461554 ) ) ;
#8865 = VERTEX_POINT ( 'NONE', #26572 ) ;
#8866 = DIRECTION ( 'NONE',  ( 0.09332174201254196666, 0.9956360040033428449, 0.000000000000000000 ) ) ;
#8867 = VERTEX_POINT ( 'NONE', #8348 ) ;
#8868 = DIRECTION ( 'NONE',  ( 1.352396030810764649E-06, 5.694414615768204918E-07, 0.9999999999989234167 ) ) ;
#8869 =( BOUNDED_CURVE ( )  B_SPLINE_CURVE ( 3, ( #5244, #26931, #20261, #31101 ),
 .UNSPECIFIED., .F., .F. ) 
 B_SPLINE_CURVE_WITH_KNOTS ( ( 4, 4 ),
 ( 4.712388980384691450, 4.921828490624010399 ),
 .UNSPECIFIED. ) 
 CURVE ( )  GEOMETRIC_REPRESENTATION_ITEM ( )  RATIONAL_B_SPLINE_CURVE ( ( 1.000000000000000000, 0.9963479302455156006, 0.9963479302455156006, 1.000000000000000000 ) ) 
 REPRESENTATION_ITEM ( '' )  );
#8870 = DIRECTION ( 'NONE',  ( -3.071710424422018668E-17, 6.404604876783312462E-16, 1.000000000000000000 ) ) ;
#8871 = ORIENTED_EDGE ( 'NONE', *, *, #1506, .T. ) ;
#8872 = CARTESIAN_POINT ( 'NONE',  ( -10.48085350821551742, -13.91959267249018950, 57.44825035245948186 ) ) ;
#8873 = EDGE_CURVE ( 'NONE', #35369, #1693, #37590, .T. ) ;
#8874 = ORIENTED_EDGE ( 'NONE', *, *, #15055, .T. ) ;
#8875 = CARTESIAN_POINT ( 'NONE',  ( -17.32409385759798681, -9.359200813967568422, 50.49621490985803263 ) ) ;
#8876 = CARTESIAN_POINT ( 'NONE',  ( -21.61813247623101830, -8.651786778886961571, 73.71633474065167491 ) ) ;
#8877 = ORIENTED_EDGE ( 'NONE', *, *, #20906, .T. ) ;
#8878 = FACE_OUTER_BOUND ( 'NONE', #36345, .T. ) ;
#8879 = ADVANCED_FACE ( 'NONE', ( #4903 ), #16892, .T. ) ;
#8880 = EDGE_CURVE ( 'NONE', #20471, #18227, #3141, .T. ) ;
#8881 = CARTESIAN_POINT ( 'NONE',  ( -18.51768661843271602, -21.77690966467453393, 68.70025907080108141 ) ) ;
#8882 = CARTESIAN_POINT ( 'NONE',  ( -15.80534385650551599, -8.801233750844183135, 48.81488406609782515 ) ) ;
#8883 = FACE_OUTER_BOUND ( 'NONE', #8852, .T. ) ;
#8884 = CARTESIAN_POINT ( 'NONE',  ( -14.79922921121938195, -7.836842249070715916, 57.03495322699122738 ) ) ;
#8885 = DIRECTION ( 'NONE',  ( -2.403795749289375575E-06, -2.069898561751298366E-06, -0.9999999999949685803 ) ) ;
#8886 = EDGE_LOOP ( 'NONE', ( #12482, #10563, #46876, #38395, #38706 ) ) ;
#8888 = DIRECTION ( 'NONE',  ( 1.000000000000000000, 0.000000000000000000, 8.260587980841940012E-17 ) ) ;
#8887 =( BOUNDED_CURVE ( )  B_SPLINE_CURVE ( 3, ( #44337, #10589, #14722, #37148 ),
 .UNSPECIFIED., .F., .F. ) 
 B_SPLINE_CURVE_WITH_KNOTS ( ( 4, 4 ),
 ( 0.4074455897393665649, 0.5000000000000000000 ),
 .UNSPECIFIED. ) 
 CURVE ( )  GEOMETRIC_REPRESENTATION_ITEM ( )  RATIONAL_B_SPLINE_CURVE ( ( 0.6983129098260959511, 0.7760317562607057518, 0.8765941196520083967, 1.000000000000007772 ) ) 
 REPRESENTATION_ITEM ( '' )  );
#8889 = CARTESIAN_POINT ( 'NONE',  ( -10.47368616940683772, -17.49164935309025282, 64.67093470525151133 ) ) ;
#8890 = B_SPLINE_CURVE_WITH_KNOTS ( 'NONE', 3,
 ( #33151, #21612, #17422, #32454, #40798, #7083, #6350, #21380, #18380, #43784 ),
 .UNSPECIFIED., .F., .F.,
 ( 4, 2, 2, 2, 4 ),
 ( 0.6272669072877604668, 0.7522669073072733026, 0.8772669073267862494, 1.002266907346299085, 1.127266907365811921 ),
 .UNSPECIFIED. ) ;
#8891 = CARTESIAN_POINT ( 'NONE',  ( -15.49284385541290376, -8.630756214087227818, 51.74842643355271576 ) ) ;
#8892 = DIRECTION ( 'NONE',  ( 0.000000000000000000, 0.000000000000000000, 1.000000000000000000 ) ) ;
#8893 = CARTESIAN_POINT ( 'NONE',  ( -24.76302562995550716, -16.09181782173303077, 66.20291600427756862 ) ) ;
#8894 = EDGE_LOOP ( 'NONE', ( #28083, #40268, #32080, #16621, #37192 ) ) ;
#8895 = VERTEX_POINT ( 'NONE', #17156 ) ;
#8896 = CARTESIAN_POINT ( 'NONE',  ( -24.47598042472018776, -12.40625281542414449, 73.43499722901042048 ) ) ;
#8897 = DIRECTION ( 'NONE',  ( -0.7171836970970659753, 0.6968841687240312499, -4.479616660400631173E-09 ) ) ;
#8898 = EDGE_LOOP ( 'NONE', ( #25578, #34378 ) ) ;
#8899 = CARTESIAN_POINT ( 'NONE',  ( -15.68463861365884249, -7.564349260043091938, 67.25351876580783994 ) ) ;
#8900 = CARTESIAN_POINT ( 'NONE',  ( -50.42409385541304800, -25.10920654474410441, 63.99999999999998579 ) ) ;
#8901 = CARTESIAN_POINT ( 'NONE',  ( -23.02926993209503337, -10.53310206560860074, 59.90203402044859615 ) ) ;
#8902 = CARTESIAN_POINT ( 'NONE',  ( -13.01353307917097268, -8.804980454159759162, 64.09441913135431435 ) ) ;
#8903 = CARTESIAN_POINT ( 'NONE',  ( -24.28619334359350290, -16.42731978468327014, 59.13804568661029037 ) ) ;
#8904 = PLANE ( 'NONE',  #19204 ) ;
#8905 =( BOUNDED_CURVE ( )  B_SPLINE_CURVE ( 3, ( #36814, #3099, #18107, #44485 ),
 .UNSPECIFIED., .F., .F. ) 
 B_SPLINE_CURVE_WITH_KNOTS ( ( 4, 4 ),
 ( 0.9074455897393663983, 1.000000000000000000 ),
 .UNSPECIFIED. ) 
 CURVE ( )  GEOMETRIC_REPRESENTATION_ITEM ( )  RATIONAL_B_SPLINE_CURVE ( ( 0.6983129098261118273, 0.7760317562607144115, 0.8765941196520105061, 1.000000000000000000 ) ) 
 REPRESENTATION_ITEM ( '' )  );
#8906 = ORIENTED_EDGE ( 'NONE', *, *, #34780, .F. ) ;
#8907 = CARTESIAN_POINT ( 'NONE',  ( -16.50613596612109646, -22.20251566029174128, 65.48210330380625521 ) ) ;
#8908 = EDGE_CURVE ( 'NONE', #25681, #35257, #27064, .T. ) ;
#8909 = CARTESIAN_POINT ( 'NONE',  ( -20.83485798093626329, -8.694536558548913163, 59.95198372774736129 ) ) ;
#8910 = CARTESIAN_POINT ( 'NONE',  ( -22.51432625447135649, -9.926136081597567440, 70.01178455096938080 ) ) ;
#8911 = CYLINDRICAL_SURFACE ( 'NONE', #29537, 5.249999999999998224 ) ;
#8912 = CARTESIAN_POINT ( 'NONE',  ( -21.49815937814055999, -9.116931945208399668, 70.43132539264750847 ) ) ;
#8913 = ORIENTED_EDGE ( 'NONE', *, *, #40227, .T. ) ;
#8914 = ORIENTED_EDGE ( 'NONE', *, *, #27126, .T. ) ;
#8915 = CARTESIAN_POINT ( 'NONE',  ( -22.69284385650552238, -7.406986770994973490, 48.81910596585309747 ) ) ;
#8916 = VERTEX_POINT ( 'NONE', #31474 ) ;
#8917 = EDGE_CURVE ( 'NONE', #14347, #21243, #32024, .T. ) ;
#8918 = CARTESIAN_POINT ( 'NONE',  ( -12.01449246772864576, -9.686654477736338364, 60.73730818761442407 ) ) ;
#8919 = EDGE_CURVE ( 'NONE', #6766, #26691, #38745, .T. ) ;
#8920 = CARTESIAN_POINT ( 'NONE',  ( -11.00038316533314919, -18.58284169098544680, 57.98431467230947334 ) ) ;
#8921 = B_SPLINE_CURVE_WITH_KNOTS ( 'NONE', 1,
 ( #28399, #32559 ),
 .UNSPECIFIED., .F., .F.,
 ( 2, 2 ),
 ( 0.000000000000000000, 1.000000000000000000 ),
 .UNSPECIFIED. ) ;
#8922 = ORIENTED_EDGE ( 'NONE', *, *, #31100, .T. ) ;
#8923 = CARTESIAN_POINT ( 'NONE',  ( -10.43244324318236593, -14.46516609096106265, 67.85800133269570722 ) ) ;
#8924 = CARTESIAN_POINT ( 'NONE',  ( -43.06159385541306506, -14.80920654474410902, 57.89999999999999147 ) ) ;
#8925 = CIRCLE ( 'NONE', #12840, 4.686499999999997890 ) ;
#8926 = ORIENTED_EDGE ( 'NONE', *, *, #19348, .F. ) ;
#8927 = CARTESIAN_POINT ( 'NONE',  ( -10.64059482219176722, -17.88964966403732859, 71.70571712204632320 ) ) ;
#8928 = CARTESIAN_POINT ( 'NONE',  ( -19.44371787714632305, -21.98101111209947334, 58.63852002154196441 ) ) ;
#8929 = VERTEX_POINT ( 'NONE', #20401 ) ;
#8930 = CARTESIAN_POINT ( 'NONE',  ( -11.30361205576526196, -11.41219277671509147, 64.44882039656690154 ) ) ;
#8931 = CARTESIAN_POINT ( 'NONE',  ( -17.39742496553465401, -7.759256980052345654, 67.02039592192090822 ) ) ;
#8932 = ORIENTED_EDGE ( 'NONE', *, *, #45634, .T. ) ;
#8933 = CARTESIAN_POINT ( 'NONE',  ( -16.00544582274271477, -7.903112417841744453, 63.95538887075813506 ) ) ;
#8934 = CARTESIAN_POINT ( 'NONE',  ( -22.21960400195047569, -20.51063794322999101, 58.87104585263988099 ) ) ;
#8935 = CYLINDRICAL_SURFACE ( 'NONE', #24240, 1.249999999999998668 ) ;
#8936 = ORIENTED_EDGE ( 'NONE', *, *, #6120, .F. ) ;
#8937 = CARTESIAN_POINT ( 'NONE',  ( -24.27074747244433794, -17.74661109614212506, 62.63394374183828006 ) ) ;
#8938 = EDGE_CURVE ( 'NONE', #29708, #10558, #21123, .T. ) ;
#8939 = EDGE_CURVE ( 'NONE', #28685, #47879, #43980, .T. ) ;
#8940 = DIRECTION ( 'NONE',  ( 2.866981220435666553E-17, -1.000000000000000000, -1.190614954331866791E-16 ) ) ;
#8941 = CARTESIAN_POINT ( 'NONE',  ( -20.06975372951847447, -8.274133229585533655, 73.73568642813194174 ) ) ;
#8942 = CARTESIAN_POINT ( 'NONE',  ( -14.60783717270099835, -21.70648693424663378, 58.35113322083577003 ) ) ;
#8943 = CARTESIAN_POINT ( 'NONE',  ( -24.47354813883760016, -12.39902559715248032, 73.42720875634239519 ) ) ;
#8944 = DIRECTION ( 'NONE',  ( 3.549360974554993999E-17, -6.371834667797928663E-18, -1.000000000000000000 ) ) ;
#8945 = ORIENTED_EDGE ( 'NONE', *, *, #6911, .T. ) ;
#8946 = CARTESIAN_POINT ( 'NONE',  ( -24.43362379028604536, -14.05489247495133753, 73.12271507725591846 ) ) ;
#8947 = CARTESIAN_POINT ( 'NONE',  ( -23.46741973463711872, -19.16603908095663655, 62.53902270128352825 ) ) ;
#8948 = CARTESIAN_POINT ( 'NONE',  ( -14.60689809042302834, -8.346551666329650843, 64.08978840692947188 ) ) ;
#8949 = EDGE_CURVE ( 'NONE', #29810, #16043, #12178, .T. ) ;
#8950 = ADVANCED_FACE ( 'NONE', ( #5140 ), #9805, .T. ) ;
#8951 = CARTESIAN_POINT ( 'NONE',  ( -18.22409385759798894, -9.359200813967568422, 50.49621490985803263 ) ) ;
#8952 = CARTESIAN_POINT ( 'NONE',  ( -17.40534385650551741, -8.801233750844183135, 48.81488406609782515 ) ) ;
#8954 = EDGE_CURVE ( 'NONE', #39770, #41197, #4995, .T. ) ;
#8953 = VERTEX_POINT ( 'NONE', #39098 ) ;
#8955 = DIRECTION ( 'NONE',  ( -0.9979768094191907579, -0.06357898915123130767, 0.000000000000000000 ) ) ;
#8956 = DIRECTION ( 'NONE',  ( -0.7364384864160969935, 0.6765045127160409510, 1.031360481960658298E-08 ) ) ;
#8957 = ORIENTED_EDGE ( 'NONE', *, *, #29794, .T. ) ;
#8958 = DIRECTION ( 'NONE',  ( -0.000000000000000000, 0.000000000000000000, 1.000000000000000000 ) ) ;
#8959 = CARTESIAN_POINT ( 'NONE',  ( -10.60259942276942802, -17.80446876823743096, 71.69001273946355468 ) ) ;
#8960 = EDGE_CURVE ( 'NONE', #41932, #891, #17616, .T. ) ;
#8961 = DIRECTION ( 'NONE',  ( 2.866981220435666553E-17, -1.000000000000000000, -1.190614954331866791E-16 ) ) ;
#8962 = CARTESIAN_POINT ( 'NONE',  ( 18.57590614458706924, 3.114729847420145248, 50.78398819077499127 ) ) ;
#8963 = ORIENTED_EDGE ( 'NONE', *, *, #15879, .F. ) ;
#8964 = DIRECTION ( 'NONE',  ( 1.224646799147353207E-16, 1.000000000000000000, -1.912410701131276611E-32 ) ) ;
#8965 = CARTESIAN_POINT ( 'NONE',  ( -12.32158608955787393, -9.943909642237139579, 60.57390139315987909 ) ) ;
#8966 = EDGE_CURVE ( 'NONE', #12002, #36239, #6280, .T. ) ;
#8967 = EDGE_LOOP ( 'NONE', ( #17379, #39570, #12815, #22227, #26340 ) ) ;
#8968 = CARTESIAN_POINT ( 'NONE',  ( -12.69763806180496601, -20.04058448603118592, 68.62185382311069759 ) ) ;
#8969 = CARTESIAN_POINT ( 'NONE',  ( -24.23802539630901265, -11.79523892523793371, 59.66890987421792403 ) ) ;
#8970 = CARTESIAN_POINT ( 'NONE',  ( -10.40062145488671241, -15.42068369279106221, 57.56792819272491357 ) ) ;
#8971 = DIRECTION ( 'NONE',  ( -9.588436366354112311E-09, -2.115493567789935748E-07, -0.9999999999999775735 ) ) ;
#8972 = CARTESIAN_POINT ( 'NONE',  ( -9.424093855413055110, -25.10920654474410441, 54.99999999999997868 ) ) ;
#8973 = ORIENTED_EDGE ( 'NONE', *, *, #23115, .T. ) ;
#8974 = ORIENTED_EDGE ( 'NONE', *, *, #2600, .T. ) ;
#8975 = CARTESIAN_POINT ( 'NONE',  ( -21.00534385541304161, -7.595227055684746986, 51.75156210489594599 ) ) ;
#8976 = CARTESIAN_POINT ( 'NONE',  ( -22.99332866974948075, -9.860676417004754057, 70.18991268411126327 ) ) ;
#8977 = B_SPLINE_CURVE_WITH_KNOTS ( 'NONE', 1,
 ( #11305, #26317 ),
 .UNSPECIFIED., .F., .F.,
 ( 2, 2 ),
 ( 0.000000000000000000, 1.000000000000000000 ),
 .UNSPECIFIED. ) ;
#8978 = CARTESIAN_POINT ( 'NONE',  ( -19.01758550583589269, -21.68056959198661815, 58.82507637440430415 ) ) ;
#8979 = B_SPLINE_CURVE_WITH_KNOTS ( 'NONE', 3,
 ( #39107, #39836, #2164, #13227, #6104, #12772, #5390, #20413, #9580, #47481 ),
 .UNSPECIFIED., .F., .F.,
 ( 4, 2, 2, 2, 4 ),
 ( 0.6272669072877348206, 0.7522669073072507651, 0.8772669073267668205, 1.002266907346282876, 1.127266907365798820 ),
 .UNSPECIFIED. ) ;
#8980 = SPHERICAL_SURFACE ( 'NONE', #45766, 4.000000000000000000 ) ;
#8981 = CARTESIAN_POINT ( 'NONE',  ( -13.94388580779785691, -20.88290965541650479, 68.75625091190090643 ) ) ;
#8982 = ORIENTED_EDGE ( 'NONE', *, *, #39547, .F. ) ;
#8983 = CARTESIAN_POINT ( 'NONE',  ( -10.36617775085144899, -14.83726598580069300, 68.01367321887373407 ) ) ;
#8984 = CARTESIAN_POINT ( 'NONE',  ( -18.26345899425187369, -22.21252533677388286, 65.45876839498835409 ) ) ;
#8985 = EDGE_CURVE ( 'NONE', #454, #26524, #26211, .T. ) ;
#8986 = ORIENTED_EDGE ( 'NONE', *, *, #11769, .F. ) ;
#8987 = CARTESIAN_POINT ( 'NONE',  ( -21.25293954998800672, -20.66975872501122424, 72.54063127481728657 ) ) ;
#8988 = CARTESIAN_POINT ( 'NONE',  ( -12.94846085306722294, -9.425284032318575811, 74.54752936559843590 ) ) ;
#8989 = VECTOR ( 'NONE', #7883, 1000.000000000000227 ) ;
#8990 = EDGE_LOOP ( 'NONE', ( #41040, #43919 ) ) ;
#8991 = CARTESIAN_POINT ( 'NONE',  ( -13.29845767883066543, -21.01266560759323809, 61.63150935275904629 ) ) ;
#8992 = CARTESIAN_POINT ( 'NONE',  ( -10.42338558849718311, -15.67229764252504332, 57.56792711140763430 ) ) ;
#8993 = VERTEX_POINT ( 'NONE', #124 ) ;
#8994 = CARTESIAN_POINT ( 'NONE',  ( -12.14425528403576493, -10.13739698163135117, 64.02914326607979945 ) ) ;
#8995 = EDGE_CURVE ( 'NONE', #31288, #9885, #47129, .T. ) ;
#8996 = AXIS2_PLACEMENT_3D ( 'NONE', #16436, #43036, #9315 ) ;
#8997 = B_SPLINE_CURVE_WITH_KNOTS ( 'NONE', 3,
 ( #6442, #28602, #13313, #9660, #17730, #10382, #20969, #9413, #24675, #24437 ),
 .UNSPECIFIED., .F., .F.,
 ( 4, 2, 2, 2, 4 ),
 ( 0.1272669073658574679, 0.2522669073463327249, 0.3772669073268078987, 0.5022669073072831836, 0.6272669072877583574 ),
 .UNSPECIFIED. ) ;
#8998 = FACE_OUTER_BOUND ( 'NONE', #27506, .T. ) ;
#8999 = CARTESIAN_POINT ( 'NONE',  ( -15.15660932275500272, -21.48492473237050859, 65.39124617759186719 ) ) ;
#9000 = CARTESIAN_POINT ( 'NONE',  ( -24.30269918248666272, -16.11583968492636032, 66.25252109504093312 ) ) ;
#9001 = ORIENTED_EDGE ( 'NONE', *, *, #1094, .F. ) ;
#9002 = CARTESIAN_POINT ( 'NONE',  ( -15.66732230932660741, -10.46443543628982376, 52.02966884056656482 ) ) ;
#9003 = DIRECTION ( 'NONE',  ( 1.000000000000000000, -4.164305804376849788E-17, 1.614929280266638808E-16 ) ) ;
#9004 = CARTESIAN_POINT ( 'NONE',  ( -21.31115985637654120, -8.927249709250720144, 73.88656608925673197 ) ) ;
#9005 = FACE_BOUND ( 'NONE', #29615, .T. ) ;
#9006 = EDGE_CURVE ( 'NONE', #29810, #47031, #12921, .T. ) ;
#9007 = CARTESIAN_POINT ( 'NONE',  ( -10.37462438995674319, -14.89569194323783208, 74.79778901495059529 ) ) ;
#9008 = CARTESIAN_POINT ( 'NONE',  ( -17.60317953294568127, -7.758478677834707682, 67.43528183898541783 ) ) ;
#9009 = EDGE_CURVE ( 'NONE', #23509, #35946, #15107, .T. ) ;
#9010 = DIRECTION ( 'NONE',  ( 1.000000000000000000, -0.000000000000000000, -0.000000000000000000 ) ) ;
#9011 = ORIENTED_EDGE ( 'NONE', *, *, #10917, .T. ) ;
#9012 = CARTESIAN_POINT ( 'NONE',  ( -23.64494593247637866, -11.48417377041487164, 62.95218242698565092 ) ) ;
#9013 = ADVANCED_FACE ( 'NONE', ( #15346 ), #41467, .T. ) ;
#9014 = ORIENTED_EDGE ( 'NONE', *, *, #9521, .F. ) ;
#9015 = CARTESIAN_POINT ( 'NONE',  ( -11.71918404020638427, -18.95175453447547653, 71.70158022526054253 ) ) ;
#9016 = DIRECTION ( 'NONE',  ( -3.071710424422018668E-17, 6.404604876783312462E-16, 1.000000000000000000 ) ) ;
#9017 = ORIENTED_EDGE ( 'NONE', *, *, #44678, .T. ) ;
#9018 = FACE_OUTER_BOUND ( 'NONE', #26145, .T. ) ;
#9019 = CARTESIAN_POINT ( 'NONE',  ( -11.93195840498443516, -10.38844327383712773, 70.98365212470247343 ) ) ;
#9020 = B_SPLINE_CURVE_WITH_KNOTS ( 'NONE', 3,
 ( #19521, #15562, #4752, #30867, #45881, #12136, #38468, #15079, #24192, #39199 ),
 .UNSPECIFIED., .F., .F.,
 ( 4, 2, 2, 2, 4 ),
 ( 0.000000000000000000, 0.2500000000000000000, 0.5000000000000000000, 0.7500000000000000000, 1.000000000000000000 ),
 .UNSPECIFIED. ) ;
#9021 = EDGE_LOOP ( 'NONE', ( #151, #22973, #34146, #22347 ) ) ;
#9022 = EDGE_LOOP ( 'NONE', ( #24793, #22610, #3319, #14506, #35297 ) ) ;
#9023 = ORIENTED_EDGE ( 'NONE', *, *, #22516, .T. ) ;
#9024 = DIRECTION ( 'NONE',  ( -0.9118114225829225816, -0.4106092176842893182, -5.589476761700638731E-08 ) ) ;
#9026 = EDGE_CURVE ( 'NONE', #41394, #33214, #7097, .T. ) ;
#9025 = CARTESIAN_POINT ( 'NONE',  ( -16.14284385759799179, -7.587656875400192291, 49.25157356644813689 ) ) ;
#9027 =( BOUNDED_CURVE ( )  B_SPLINE_CURVE ( 3, ( #30337, #33747, #22200, #37187 ),
 .UNSPECIFIED., .F., .F. ) 
 B_SPLINE_CURVE_WITH_KNOTS ( ( 4, 4 ),
 ( 0.4074455897393669535, 0.5000000000000000000 ),
 .UNSPECIFIED. ) 
 CURVE ( )  GEOMETRIC_REPRESENTATION_ITEM ( )  RATIONAL_B_SPLINE_CURVE ( ( 0.6983129098260987266, 0.7760317562607002007, 0.8765941196519997369, 0.9999999999999954481 ) ) 
 REPRESENTATION_ITEM ( '' )  );
#9028 = CARTESIAN_POINT ( 'NONE',  ( -21.22430400244884297, -8.930495821374908161, 73.67416693519540161 ) ) ;
#9029 = CARTESIAN_POINT ( 'NONE',  ( -10.60833884242739522, -12.99528357717770355, 64.15347367985145866 ) ) ;
#9030 = CARTESIAN_POINT ( 'NONE',  ( -13.65433549462749596, -7.199988887673270277, 54.38277594638588397 ) ) ;
#9031 = EDGE_LOOP ( 'NONE', ( #17353, #1870 ) ) ;
#9032 = ORIENTED_EDGE ( 'NONE', *, *, #336, .T. ) ;
#9033 = VECTOR ( 'NONE', #36575, 1000.000000000000114 ) ;
#9034 = CARTESIAN_POINT ( 'NONE',  ( -21.20534385650551812, -8.801233750844183135, 48.81488406609782515 ) ) ;
#9035 = PRODUCT_DEFINITION ( 'UNKNOWN', '', #7003, #32670 ) ;
#9036 = VECTOR ( 'NONE', #39639, 1000.000000000000000 ) ;
#9037 = CARTESIAN_POINT ( 'NONE',  ( -21.51679988820674438, -20.55329806219026523, 72.40957539702174017 ) ) ;
#9038 = CARTESIAN_POINT ( 'NONE',  ( -20.68814852852636221, -21.05812772122902388, 58.94475156075989730 ) ) ;
#9039 = DIRECTION ( 'NONE',  ( 6.651268170491444817E-06, 3.577353459756793540E-06, 0.9999999999714814791 ) ) ;
#9040 = CARTESIAN_POINT ( 'NONE',  ( -23.11784385650551954, -9.790100578890868377, 49.79778022625162492 ) ) ;
#9041 =( BOUNDED_CURVE ( )  B_SPLINE_CURVE ( 3, ( #11325, #33452, #37394, #26337 ),
 .UNSPECIFIED., .F., .F. ) 
 B_SPLINE_CURVE_WITH_KNOTS ( ( 4, 4 ),
 ( 0.4074455897393630677, 0.5000000000000000000 ),
 .UNSPECIFIED. ) 
 CURVE ( )  GEOMETRIC_REPRESENTATION_ITEM ( )  RATIONAL_B_SPLINE_CURVE ( ( 0.6983129098260806300, 0.7760317562606832142, 0.8765941196519884127, 0.9999999999999931166 ) ) 
 REPRESENTATION_ITEM ( '' )  );
#9042 = ORIENTED_EDGE ( 'NONE', *, *, #15248, .F. ) ;
#9043 = CARTESIAN_POINT ( 'NONE',  ( -14.73375560093340120, -21.75656996136207866, 61.75105004614717785 ) ) ;
#9044 = CARTESIAN_POINT ( 'NONE',  ( -41.91674091423659121, -14.80920654474410547, 67.05882352941175384 ) ) ;
#9045 = CARTESIAN_POINT ( 'NONE',  ( -24.46050813376110611, -17.25744323842079098, 73.04482527373910727 ) ) ;
#9046 = EDGE_CURVE ( 'NONE', #48213, #42290, #40095, .T. ) ;
#9047 = EDGE_LOOP ( 'NONE', ( #46287, #34318, #45469, #4124, #1210 ) ) ;
#9048 = CARTESIAN_POINT ( 'NONE',  ( -11.59752430615055729, -18.69167855836258596, 68.32762835703452708 ) ) ;
#9049 = CARTESIAN_POINT ( 'NONE',  ( -10.37394849890712401, -14.76283852923608464, 71.61310637325181006 ) ) ;
#9050 = LINE ( 'NONE', #24066, #20157 ) ;
#9051 = CARTESIAN_POINT ( 'NONE',  ( -19.10873388551254948, -7.551407109436953924, 67.08727174327995613 ) ) ;
#9052 = ORIENTED_EDGE ( 'NONE', *, *, #25102, .T. ) ;
#9053 = CARTESIAN_POINT ( 'NONE',  ( -24.46506320217640962, -17.24406362331221132, 72.99840605271779737 ) ) ;
#9054 = CARTESIAN_POINT ( 'NONE',  ( -22.88305309436651669, -19.19300359198548378, 58.95580955766958198 ) ) ;
#9055 = CARTESIAN_POINT ( 'NONE',  ( -10.33431723597471930, -12.52035407725662886, 60.98348989824278732 ) ) ;
#9056 = ORIENTED_EDGE ( 'NONE', *, *, #18929, .F. ) ;
#9057 = CARTESIAN_POINT ( 'NONE',  ( -17.15134030326023051, -7.364115279526828317, 70.67531275522621570 ) ) ;
#9058 = ORIENTED_EDGE ( 'NONE', *, *, #36915, .T. ) ;
#9059 = AXIS2_PLACEMENT_3D ( 'NONE', #26644, #26390, #41405 ) ;
#9060 = CARTESIAN_POINT ( 'NONE',  ( -33.52409385541305653, -8.109206544744111511, 51.54999999999998295 ) ) ;
#9061 = DIRECTION ( 'NONE',  ( -1.000000000000000000, -2.866981220435666553E-17, -0.000000000000000000 ) ) ;
#9062 = ORIENTED_EDGE ( 'NONE', *, *, #26391, .F. ) ;
#9063 = CARTESIAN_POINT ( 'NONE',  ( -22.20754945420574700, -20.52070228389602136, 58.96431674811245927 ) ) ;
#9064 = AXIS2_PLACEMENT_3D ( 'NONE', #28241, #6315, #17124 ) ;
#9065 = FACE_OUTER_BOUND ( 'NONE', #1608, .T. ) ;
#9066 = ADVANCED_FACE ( 'NONE', ( #37262 ), #29656, .T. ) ;
#9067 = CARTESIAN_POINT ( 'NONE',  ( -48.42409385541304800, -25.10920654474410441, 81.99999999999998579 ) ) ;
#9068 = ORIENTED_EDGE ( 'NONE', *, *, #8538, .T. ) ;
#9069 = CARTESIAN_POINT ( 'NONE',  ( -13.42213083866590040, -20.61341924012868887, 58.34090257147585135 ) ) ;
#9070 = UNCERTAINTY_MEASURE_WITH_UNIT (LENGTH_MEASURE( 1.000000000000000082E-05 ), #22723, 'distance_accuracy_value', 'NONE');
#9071 = EDGE_CURVE ( 'NONE', #4198, #48039, #29937, .T. ) ;
#9072 = CARTESIAN_POINT ( 'NONE',  ( -20.81921488491704864, -21.44071703825394692, 58.75979854551385984 ) ) ;
#9073 = B_SPLINE_CURVE_WITH_KNOTS ( 'NONE', 3,
 ( #40358, #21420, #24863, #29281, #6631, #17462, #2684, #25821, #10082, #44315 ),
 .UNSPECIFIED., .F., .F.,
 ( 4, 2, 2, 2, 4 ),
 ( 0.000000000000000000, 0.2500000000000000000, 0.5000000000000000000, 0.7500000000000000000, 1.000000000000000000 ),
 .UNSPECIFIED. ) ;
#9074 = CARTESIAN_POINT ( 'NONE',  ( -46.38423044223897307, -13.72754205882879042, 70.87000000000000455 ) ) ;
#9075 = ORIENTED_EDGE ( 'NONE', *, *, #43117, .T. ) ;
#9076 = CARTESIAN_POINT ( 'NONE',  ( -10.62601537294527176, -11.76145610990993617, 74.65816588861473235 ) ) ;
#9077 = EDGE_CURVE ( 'NONE', #27516, #10658, #6491, .T. ) ;
#9078 = DIRECTION ( 'NONE',  ( -0.9893874368562772803, 0.1453014101478918851, -1.482692748682289258E-17 ) ) ;
#9079 = ORIENTED_EDGE ( 'NONE', *, *, #1762, .T. ) ;
#9080 = ORIENTED_EDGE ( 'NONE', *, *, #22857, .F. ) ;
#9081 = CARTESIAN_POINT ( 'NONE',  ( -46.47622156840087371, -14.20920654474410760, 70.43449436244988249 ) ) ;
#9082 = PLANE ( 'NONE',  #11551 ) ;
#9083 = DIRECTION ( 'NONE',  ( -0.9687793358424823253, 0.2479245821708663811, 0.000000000000000000 ) ) ;
#9084 = CARTESIAN_POINT ( 'NONE',  ( -18.02409385650551599, -6.426201560718813433, 50.50509628382439331 ) ) ;
#9085 = FACE_OUTER_BOUND ( 'NONE', #35536, .T. ) ;
#9086 = EDGE_CURVE ( 'NONE', #17474, #997, #21740, .T. ) ;
#9087 = FACE_OUTER_BOUND ( 'NONE', #4120, .T. ) ;
#9088 = CARTESIAN_POINT ( 'NONE',  ( -24.28125388808335927, -13.17092994507341430, 62.83823998052931614 ) ) ;
#9089 = EDGE_CURVE ( 'NONE', #13644, #42456, #16997, .T. ) ;
#9090 = DIRECTION ( 'NONE',  ( 0.000000000000000000, 0.000000000000000000, 1.000000000000000000 ) ) ;
#9091 = ORIENTED_EDGE ( 'NONE', *, *, #33760, .T. ) ;
#9092 = ORIENTED_EDGE ( 'NONE', *, *, #15458, .T. ) ;
#9093 = CARTESIAN_POINT ( 'NONE',  ( -10.99668346656864060, -11.04197136062318307, 60.72239829427679325 ) ) ;
#9094 = CARTESIAN_POINT ( 'NONE',  ( -22.52409385541004383, -9.359200813967481380, 50.49621490983041383 ) ) ;
#9095 = DIRECTION ( 'NONE',  ( 1.235321093103353499E-06, 4.801898924785047334E-07, 0.9999999999991215915 ) ) ;
#9096 = CARTESIAN_POINT ( 'NONE',  ( -11.09043784728536863, -11.82832424043013475, 71.37395526268804247 ) ) ;
#9097 = VECTOR ( 'NONE', #7148, 1000.000000000000000 ) ;
#9098 = VERTEX_POINT ( 'NONE', #20037 ) ;
#9099 = CARTESIAN_POINT ( 'NONE',  ( -22.96375064570672819, -10.44813988596692589, 63.08658113699938497 ) ) ;
#9100 = CARTESIAN_POINT ( 'NONE',  ( -19.83890857264518104, -18.82566669410956806, 49.52966884056656482 ) ) ;
#9101 = CARTESIAN_POINT ( 'NONE',  ( -15.55814167568544448, -21.55598949654579144, 72.33110090557599392 ) ) ;
#9102 = CARTESIAN_POINT ( 'NONE',  ( -13.52409385541304410, -9.359200813967568422, 50.49621490985803263 ) ) ;
#9103 = EDGE_CURVE ( 'NONE', #8372, #11939, #43472, .T. ) ;
#9104 = ORIENTED_EDGE ( 'NONE', *, *, #20383, .F. ) ;
#9105 = CARTESIAN_POINT ( 'NONE',  ( -24.84806299871600643, -14.18603056061780343, 69.69629353939886585 ) ) ;
#9106 = FACE_OUTER_BOUND ( 'NONE', #22524, .T. ) ;
#9107 = ORIENTED_EDGE ( 'NONE', *, *, #2590, .F. ) ;
#9108 = CARTESIAN_POINT ( 'NONE',  ( -24.42331094633779998, -14.99212722102677198, 59.43227208747884305 ) ) ;
#9109 = CARTESIAN_POINT ( 'NONE',  ( -12.94457089969240648, -20.18822822247345883, 71.99756910775208496 ) ) ;
#9110 = CARTESIAN_POINT ( 'NONE',  ( -23.77562434277295367, -17.86939608417919345, 59.01850491586762359 ) ) ;
#9111 = ORIENTED_EDGE ( 'NONE', *, *, #1768, .F. ) ;
#9112 = ADVANCED_FACE ( 'NONE', ( #1808 ), #258, .T. ) ;
#9113 = CARTESIAN_POINT ( 'NONE',  ( -12.96596342764269316, -9.347744029417796696, 71.14925352873375175 ) ) ;
#9114 = VERTEX_POINT ( 'NONE', #842 ) ;
#9115 = CARTESIAN_POINT ( 'NONE',  ( -22.67171275331017810, -14.65110561991362381, 52.02966884056656482 ) ) ;
#9116 = CARTESIAN_POINT ( 'NONE',  ( -10.42420801082433712, -14.84918507598050219, 71.51885965942804546 ) ) ;
#9117 = ORIENTED_EDGE ( 'NONE', *, *, #35700, .F. ) ;
#9118 = CARTESIAN_POINT ( 'NONE',  ( -14.97188219925329378, -8.199429090594037461, 57.14999999999993463 ) ) ;
#9119 = CARTESIAN_POINT ( 'NONE',  ( -17.32409385650551314, -6.426201560718813433, 50.50509628382439331 ) ) ;
#9120 = ORIENTED_EDGE ( 'NONE', *, *, #39823, .T. ) ;
#9121 = CARTESIAN_POINT ( 'NONE',  ( -24.46479344033866710, -14.44719916248949154, 66.33292729247949637 ) ) ;
#9122 = CARTESIAN_POINT ( 'NONE',  ( -14.91112529534803066, -8.221969756899694559, 57.13527940342243028 ) ) ;
#9123 = DIRECTION ( 'NONE',  ( -0.6478992145799704616, 0.7617260713318516618, -1.927832152310573586E-08 ) ) ;
#9124 = VERTEX_POINT ( 'NONE', #45904 ) ;
#9125 = CARTESIAN_POINT ( 'NONE',  ( -19.04501905262167227, -19.80271247795941392, 50.77966884056656482 ) ) ;
#9126 = LINE ( 'NONE', #19962, #10948 ) ;
#9127 = CIRCLE ( 'NONE', #11470, 1.049999999999998934 ) ;
#9128 = CARTESIAN_POINT ( 'NONE',  ( -22.33041777183100507, -20.41561037748852669, 62.34943743628787161 ) ) ;
#9129 = ADVANCED_FACE ( 'NONE', ( #45674 ), #1562, .T. ) ;
#9130 = CARTESIAN_POINT ( 'NONE',  ( -48.42409385541304800, -27.10920654474410796, 81.99999999999998579 ) ) ;
#9131 = CARTESIAN_POINT ( 'NONE',  ( -20.81696448553514855, -20.93198605141084201, 62.41471400679856885 ) ) ;
#9132 = ORIENTED_EDGE ( 'NONE', *, *, #9605, .T. ) ;
#9133 = ORIENTED_EDGE ( 'NONE', *, *, #8010, .T. ) ;
#9134 = EDGE_CURVE ( 'NONE', #16415, #48249, #39232, .T. ) ;
#9135 = CARTESIAN_POINT ( 'NONE',  ( -24.17166340479750630, -16.86472320484777043, 72.88335999016837263 ) ) ;
#9136 = DIRECTION ( 'NONE',  ( -1.770046493635803029E-07, 8.183081527205841035E-08, 0.9999999999999809042 ) ) ;
#9137 = ORIENTED_EDGE ( 'NONE', *, *, #9324, .T. ) ;
#9138 = FACE_OUTER_BOUND ( 'NONE', #619, .T. ) ;
#9139 = CARTESIAN_POINT ( 'NONE',  ( -19.74436319619195501, -10.72363366794506234, 52.02966884056656482 ) ) ;
#9140 = CARTESIAN_POINT ( 'NONE',  ( -18.33659385759798965, -8.995762431863214559, 51.38120296130585274 ) ) ;
#9141 = DIRECTION ( 'NONE',  ( 0.000000000000000000, 1.000000000000000000, -5.551115123125785858E-15 ) ) ;
#9142 = CARTESIAN_POINT ( 'NONE',  ( -10.79685900591816683, -12.39371430582574796, 61.09853628380557922 ) ) ;
#9143 = ORIENTED_EDGE ( 'NONE', *, *, #19917, .T. ) ;
#9144 = B_SPLINE_CURVE_WITH_KNOTS ( 'NONE', 3,
 ( #32211, #28989, #43543, #36123, #9807, #2406, #13709, #14181, #28751, #43781 ),
 .UNSPECIFIED., .F., .F.,
 ( 4, 2, 2, 2, 4 ),
 ( 0.1272669073657799188, 0.2522669073462755485, 0.3772669073267712614, 0.5022669073072668633, 0.6272669072877625762 ),
 .UNSPECIFIED. ) ;
#9145 = CARTESIAN_POINT ( 'NONE',  ( -24.00901317767523935, -17.32824147414624960, 69.42811846502259243 ) ) ;
#9146 = CARTESIAN_POINT ( 'NONE',  ( -20.82057464141327330, -8.686965885571435564, 59.91295551501632133 ) ) ;
#9147 = FACE_OUTER_BOUND ( 'NONE', #45776, .T. ) ;
#9148 = EDGE_CURVE ( 'NONE', #20159, #13083, #12164, .T. ) ;
#9150 = VERTEX_POINT ( 'NONE', #28640 ) ;
#9149 = EDGE_CURVE ( 'NONE', #31450, #6597, #1146, .T. ) ;
#9151 = ORIENTED_EDGE ( 'NONE', *, *, #5756, .F. ) ;
#9152 = EDGE_LOOP ( 'NONE', ( #18782, #10145, #7566, #32624 ) ) ;
#9153 = EDGE_CURVE ( 'NONE', #25767, #946, #11198, .T. ) ;
#9154 = EDGE_CURVE ( 'NONE', #14388, #42196, #39718, .T. ) ;
#9155 = FACE_OUTER_BOUND ( 'NONE', #11562, .T. ) ;
#9156 = CARTESIAN_POINT ( 'NONE',  ( -21.74910605648477713, -9.305107492218610332, 63.20656180270096769 ) ) ;
#9157 =( BOUNDED_CURVE ( )  B_SPLINE_CURVE ( 3, ( #43959, #25230, #40254, #13395 ),
 .UNSPECIFIED., .F., .F. ) 
 B_SPLINE_CURVE_WITH_KNOTS ( ( 4, 4 ),
 ( 1.570796326794896780, 1.780235837034217727 ),
 .UNSPECIFIED. ) 
 CURVE ( )  GEOMETRIC_REPRESENTATION_ITEM ( )  RATIONAL_B_SPLINE_CURVE ( ( 1.000000000000000000, 0.9963479302455154896, 0.9963479302455154896, 1.000000000000000000 ) ) 
 REPRESENTATION_ITEM ( '' )  );
#9158 = B_SPLINE_CURVE_WITH_KNOTS ( 'NONE', 3,
 ( #19399, #37611, #44539, #10791, #19157, #26303, #34164, #34401, #7608, #697 ),
 .UNSPECIFIED., .F., .F.,
 ( 4, 2, 2, 2, 4 ),
 ( 0.000000000000000000, 0.2500000000000000000, 0.5000000000000000000, 0.7500000000000000000, 1.000000000000000000 ),
 .UNSPECIFIED. ) ;
#9159 = VERTEX_POINT ( 'NONE', #28873 ) ;
#9160 = DIRECTION ( 'NONE',  ( 0.000000000000000000, 1.000000000000000000, -0.000000000000000000 ) ) ;
#9161 = AXIS2_PLACEMENT_3D ( 'NONE', #17398, #31701, #9061 ) ;
#9162 = AXIS2_PLACEMENT_3D ( 'NONE', #17903, #33167, #47967 ) ;
#9163 = CARTESIAN_POINT ( 'NONE',  ( -14.92409385541306044, -14.80920654474411080, 82.49999999999998579 ) ) ;
#9164 = ORIENTED_EDGE ( 'NONE', *, *, #12671, .T. ) ;
#9165 = CARTESIAN_POINT ( 'NONE',  ( -20.13271805750754950, -8.299978134201072777, 70.53628287813307907 ) ) ;
#9166 = PLANE ( 'NONE',  #40671 ) ;
#9167 = ORIENTED_EDGE ( 'NONE', *, *, #48459, .F. ) ;
#9168 = CARTESIAN_POINT ( 'NONE',  ( -10.79232760089606735, -12.56855635920591219, 57.40145450620173051 ) ) ;
#9169 = ORIENTED_EDGE ( 'NONE', *, *, #7171, .F. ) ;
#9170 =( BOUNDED_CURVE ( )  B_SPLINE_CURVE ( 3, ( #2878, #9810, #6101, #24822 ),
 .UNSPECIFIED., .F., .F. ) 
 B_SPLINE_CURVE_WITH_KNOTS ( ( 4, 4 ),
 ( 0.9074455897393666204, 1.000000000000000000 ),
 .UNSPECIFIED. ) 
 CURVE ( )  GEOMETRIC_REPRESENTATION_ITEM ( )  RATIONAL_B_SPLINE_CURVE ( ( 0.6983129098261039447, 0.7760317562607076392, 0.8765941196520062872, 1.000000000000000000 ) ) 
 REPRESENTATION_ITEM ( '' )  );
#9171 = CARTESIAN_POINT ( 'NONE',  ( -12.01648241349452917, -10.28590705807702932, 67.49896869922172016 ) ) ;
#9172 = ORIENTED_EDGE ( 'NONE', *, *, #4814, .F. ) ;
#9173 = DIRECTION ( 'NONE',  ( -3.071710424422018668E-17, 6.404604876783312462E-16, 1.000000000000000000 ) ) ;
#9174 = CARTESIAN_POINT ( 'NONE',  ( -16.84865286310842336, -21.83598151670433296, 68.98088545748413480 ) ) ;
#9175 = CARTESIAN_POINT ( 'NONE',  ( -24.72409385541305582, -14.90920654474425255, 71.98235294117645822 ) ) ;
#9176 = VERTEX_POINT ( 'NONE', #44168 ) ;
#9177 = CARTESIAN_POINT ( 'NONE',  ( -13.60238606012557483, -8.884930320952351579, 56.96967755506135234 ) ) ;
#9178 = EDGE_CURVE ( 'NONE', #31757, #23869, #28404, .T. ) ;
#9179 = LINE ( 'NONE', #34341, #7726 ) ;
#9180 = CARTESIAN_POINT ( 'NONE',  ( -21.89264518680100835, -20.26253109894388160, 58.77915004610762395 ) ) ;
#9181 = CARTESIAN_POINT ( 'NONE',  ( -15.49415775405465645, -8.028509947901662613, 74.37985659017797957 ) ) ;
#9182 = CYLINDRICAL_SURFACE ( 'NONE', #8030, 0.1499999999999962752 ) ;
#9183 = CARTESIAN_POINT ( 'NONE',  ( -10.40425584863931263, -17.30445325246355992, 61.33460017742925174 ) ) ;
#9184 = ORIENTED_EDGE ( 'NONE', *, *, #33343, .T. ) ;
#9185 =( BOUNDED_SURFACE ( )  B_SPLINE_SURFACE ( 3, 1, ( 
 ( #34529, #27873 ),
 ( #11901, #46608 ),
 ( #46111, #810 ),
 ( #35012, #12370 ),
 ( #12615, #31330 ),
 ( #15815, #23228 ),
 ( #9174, #30624 ) ),
 .UNSPECIFIED., .T., .F., .F. ) 
 B_SPLINE_SURFACE_WITH_KNOTS ( ( 4, 3, 4 ),
 ( 2, 2 ),
 ( 0.000000000000000000, 0.5000000000000000000, 1.000000000000000000 ),
 ( 0.000000000000000000, 1.000000000000000000 ),
 .UNSPECIFIED. ) 
 GEOMETRIC_REPRESENTATION_ITEM ( )  RATIONAL_B_SPLINE_SURFACE ( (
 ( 1.000000000000000000, 1.000000000000000000),
 ( 0.3333333333333335369, 0.3333333333333330373),
 ( 0.3333333333333335369, 0.3333333333333330373),
 ( 1.000000000000000000, 1.000000000000000000),
 ( 0.3333333333333333703, 0.3333333333333333703),
 ( 0.3333333333333333703, 0.3333333333333333703),
 ( 1.000000000000000000, 1.000000000000000000) ) ) 
 REPRESENTATION_ITEM ( '' )  SURFACE ( )  );
#9186 = LINE ( 'NONE', #20746, #32107 ) ;
#9187 = CARTESIAN_POINT ( 'NONE',  ( -24.86367705086121660, -14.41520995907644753, 66.38281513983412196 ) ) ;
#9188 = CARTESIAN_POINT ( 'NONE',  ( -9.974456273375457371, -14.72748566909688073, 71.51278126739182994 ) ) ;
#9189 = CARTESIAN_POINT ( 'NONE',  ( -14.11401878847811986, -20.97727922448205007, 72.22607667752819793 ) ) ;
#9190 = CARTESIAN_POINT ( 'NONE',  ( -15.26784385650551989, -6.428312510596451368, 51.20221977374900035 ) ) ;
#9191 = VERTEX_POINT ( 'NONE', #36008 ) ;
#9192 = ADVANCED_FACE ( 'NONE', ( #9926 ), #21943, .T. ) ;
#9193 = CARTESIAN_POINT ( 'NONE',  ( -22.67064388239395711, -10.17514023627220965, 66.76855582679374379 ) ) ;
#9194 = FACE_OUTER_BOUND ( 'NONE', #329, .T. ) ;
#9195 = VERTEX_POINT ( 'NONE', #17043 ) ;
#9196 = DIRECTION ( 'NONE',  ( 0.9325317756203292952, -0.3459670625490730012, 0.1033986416233858563 ) ) ;
#9197 = CARTESIAN_POINT ( 'NONE',  ( -23.62594491300536959, -11.45603751788689095, 66.70742424642772050 ) ) ;
#9198 = CARTESIAN_POINT ( 'NONE',  ( -11.62870111763649028, -18.82374159213384601, 68.21689662501481166 ) ) ;
#9199 = CARTESIAN_POINT ( 'NONE',  ( -22.71059208588729561, -10.14448404190931186, 70.02650598627910483 ) ) ;
#9200 = CARTESIAN_POINT ( 'NONE',  ( -14.60783614669699304, -21.70648650955843806, 58.35113213314874514 ) ) ;
#9201 = ORIENTED_EDGE ( 'NONE', *, *, #27020, .F. ) ;
#9202 = CARTESIAN_POINT ( 'NONE',  ( -22.47245519635065492, -19.73066437834766873, 72.65872596779033188 ) ) ;
#9203 = VECTOR ( 'NONE', #44875, 1000.000000000000114 ) ;
#9204 = DIRECTION ( 'NONE',  ( -3.071710424422018668E-17, 6.404604876783312462E-16, 1.000000000000000000 ) ) ;
#9205 = CARTESIAN_POINT ( 'NONE',  ( -24.03011946566357437, -11.36467352769893324, 66.54497619818440057 ) ) ;
#9206 = B_SPLINE_CURVE_WITH_KNOTS ( 'NONE', 3,
 ( #43823, #5900, #24379, #9841, #32712, #47738, #39867, #35918, #6139, #21164 ),
 .UNSPECIFIED., .F., .F.,
 ( 4, 2, 2, 2, 4 ),
 ( 0.1272669073658336814, 0.2522669073487979752, 0.3772669073317622690, 0.5022669073147265628, 0.6272669072976908566 ),
 .UNSPECIFIED. ) ;
#9207 = ORIENTED_EDGE ( 'NONE', *, *, #10810, .F. ) ;
#9208 = CARTESIAN_POINT ( 'NONE',  ( -17.15293984484763712, -7.364064364366409876, 70.53389935397558475 ) ) ;
#9209 = CARTESIAN_POINT ( 'NONE',  ( -13.23553521163189828, -8.648101578109386622, 60.63288603205860738 ) ) ;
#9210 = CARTESIAN_POINT ( 'NONE',  ( -21.84079810191280657, -9.314188493807273872, 63.49153755726582915 ) ) ;
#9211 = CARTESIAN_POINT ( 'NONE',  ( -23.27284462870851911, -18.74605969774991010, 66.10917289053097079 ) ) ;
#9212 = CARTESIAN_POINT ( 'NONE',  ( -20.49775566701509177, -11.27142682889164327, 49.52966884056655772 ) ) ;
#9213 = VERTEX_POINT ( 'NONE', #21726 ) ;
#9214 = ORIENTED_EDGE ( 'NONE', *, *, #38728, .T. ) ;
#9215 = CARTESIAN_POINT ( 'NONE',  ( -20.44284385541303806, -7.587656875400192291, 49.25157356644813689 ) ) ;
#9216 = ADVANCED_FACE ( 'NONE', ( #47828 ), #2763, .T. ) ;
#9217 = EDGE_CURVE ( 'NONE', #16722, #30190, #24013, .T. ) ;
#9218 = CARTESIAN_POINT ( 'NONE',  ( -20.31413516131974717, -8.378470924821744603, 67.06632013881642251 ) ) ;
#9219 = DIRECTION ( 'NONE',  ( -0.8603395911234869020, -0.5097212845717464802, 0.000000000000000000 ) ) ;
#9220 = CARTESIAN_POINT ( 'NONE',  ( -11.79630000206883977, -19.05592701419838519, 71.97213747039440079 ) ) ;
#9221 = EDGE_CURVE ( 'NONE', #30692, #29219, #32315, .T. ) ;
#9222 = ADVANCED_FACE ( 'NONE', ( #24477 ), #35765, .T. ) ;
#9223 = LINE ( 'NONE', #16824, #932 ) ;
#9224 = CARTESIAN_POINT ( 'NONE',  ( -12.23301264461619553, -10.03852782535897958, 60.84446034103241630 ) ) ;
#9225 = CARTESIAN_POINT ( 'NONE',  ( -19.94917705995926482, -8.226604131702123013, 74.00624557436877637 ) ) ;
#9226 = CARTESIAN_POINT ( 'NONE',  ( -24.46479343890040425, -14.44719913075708995, 66.48292729247951627 ) ) ;
#9227 = ORIENTED_EDGE ( 'NONE', *, *, #35121, .F. ) ;
#9228 = CARTESIAN_POINT ( 'NONE',  ( -21.95395705827280963, -8.894478678276469097, 66.91795930326043162 ) ) ;
#9229 = LINE ( 'NONE', #23772, #1548 ) ;
#9230 = AXIS2_PLACEMENT_3D ( 'NONE', #9981, #47418, #47170 ) ;
#9231 = AXIS2_PLACEMENT_3D ( 'NONE', #17001, #12607, #35005 ) ;
#9232 = ORIENTED_EDGE ( 'NONE', *, *, #7226, .T. ) ;
#9233 = CARTESIAN_POINT ( 'NONE',  ( -12.36794899618824317, -19.72224014812425708, 61.69678633597965955 ) ) ;
#9234 = CARTESIAN_POINT ( 'NONE',  ( -12.26902364965855519, -19.54473725125994221, 57.92682373989410394 ) ) ;
#9235 = ORIENTED_EDGE ( 'NONE', *, *, #33556, .F. ) ;
#9236 = CARTESIAN_POINT ( 'NONE',  ( -12.38445583493520630, -13.33796604008351494, 50.77966884056655772 ) ) ;
#9237 = EDGE_CURVE ( 'NONE', #10986, #36933, #13429, .T. ) ;
#9238 = CYLINDRICAL_SURFACE ( 'NONE', #40713, 0.1500000000000084044 ) ;
#9239 = AXIS2_PLACEMENT_3D ( 'NONE', #4433, #15493, #12550 ) ;
#9240 = DIRECTION ( 'NONE',  ( -3.071710424422018668E-17, 6.404604876783312462E-16, 1.000000000000000000 ) ) ;
#9241 = CARTESIAN_POINT ( 'NONE',  ( -11.06285897508056593, -17.73077265676491265, 71.85252885412863577 ) ) ;
#9242 = VERTEX_POINT ( 'NONE', #3254 ) ;
#9243 = FACE_OUTER_BOUND ( 'NONE', #27968, .T. ) ;
#9244 = DIRECTION ( 'NONE',  ( 0.000000000000000000, 0.000000000000000000, 1.000000000000000000 ) ) ;
#9245 = DIRECTION ( 'NONE',  ( 1.078708504465006897E-05, 7.367657514171588156E-06, 0.9999999999146782503 ) ) ;
#9246 = FACE_BOUND ( 'NONE', #28492, .T. ) ;
#9247 = CARTESIAN_POINT ( 'NONE',  ( -19.69746735473979271, -8.127384799358436496, 73.87663944647505332 ) ) ;
#9248 = LINE ( 'NONE', #5564, #31834 ) ;
#9249 = CARTESIAN_POINT ( 'NONE',  ( -16.02567528876233993, -7.491550372963335924, 63.92656979170173059 ) ) ;
#9250 = VERTEX_POINT ( 'NONE', #48303 ) ;
#9251 = CARTESIAN_POINT ( 'NONE',  ( -45.92409385541306222, -13.51240245935757578, 70.50000000000000000 ) ) ;
#9252 = LINE ( 'NONE', #19855, #31327 ) ;
#9253 = CARTESIAN_POINT ( 'NONE',  ( -20.89331258220900978, -11.64059849529350643, 49.52966884056655772 ) ) ;
#9254 = EDGE_LOOP ( 'NONE', ( #35476, #7456, #18874, #32927 ) ) ;
#9255 = CARTESIAN_POINT ( 'NONE',  ( -20.03744868119640898, -21.78660147720172802, 69.04827188316701836 ) ) ;
#9256 = EDGE_LOOP ( 'NONE', ( #25208, #21883 ) ) ;
#9257 = VERTEX_POINT ( 'NONE', #29600 ) ;
#9258 = ORIENTED_EDGE ( 'NONE', *, *, #48395, .T. ) ;
#9259 = CARTESIAN_POINT ( 'NONE',  ( -33.42409385541304800, -7.059211358595575803, 50.50317947571981847 ) ) ;
#9260 = CARTESIAN_POINT ( 'NONE',  ( -23.19494370299929287, -18.77118727246694263, 65.82389430425217824 ) ) ;
#9261 = DIRECTION ( 'NONE',  ( 0.9687793358424821033, -0.2479245821708680464, 0.000000000000000000 ) ) ;
#9262 = CARTESIAN_POINT ( 'NONE',  ( -24.71482052093760373, -13.27635576790630090, 59.54080713533480917 ) ) ;
#9263 = CARTESIAN_POINT ( 'NONE',  ( -23.46218685299048801, -18.44850610243709710, 73.06368207112421942 ) ) ;
#9264 = VECTOR ( 'NONE', #3378, 1000.000000000000000 ) ;
#9265 = AXIS2_PLACEMENT_3D ( 'NONE', #31041, #42120, #34957 ) ;
#9266 = ORIENTED_EDGE ( 'NONE', *, *, #46458, .F. ) ;
#9267 = ORIENTED_EDGE ( 'NONE', *, *, #20686, .F. ) ;
#9268 = CARTESIAN_POINT ( 'NONE',  ( -22.89284385650552522, -7.406986770994973490, 48.81910596585309747 ) ) ;
#9269 = EDGE_CURVE ( 'NONE', #33912, #47972, #37030, .T. ) ;
#9270 = CARTESIAN_POINT ( 'NONE',  ( -11.35824856342118139, -11.21643317443627375, 60.97885780702566194 ) ) ;
#9271 = CARTESIAN_POINT ( 'NONE',  ( -14.90981300391231024, -21.39562377109201208, 61.63600440604547970 ) ) ;
#9272 = VECTOR ( 'NONE', #44429, 1000.000000000000000 ) ;
#9273 = CARTESIAN_POINT ( 'NONE',  ( -23.27033594065426314, -18.65917932524403966, 65.89677377228576916 ) ) ;
#9274 = CARTESIAN_POINT ( 'NONE',  ( -13.63659385650551847, -6.915538690918075382, 49.31353937987644542 ) ) ;
#9275 = VECTOR ( 'NONE', #16306, 1000.000000000000000 ) ;
#9277 = ORIENTED_EDGE ( 'NONE', *, *, #45851, .T. ) ;
#9276 = EDGE_CURVE ( 'NONE', #501, #13279, #7454, .T. ) ;
#9278 = CARTESIAN_POINT ( 'NONE',  ( -23.09439617342594886, -10.70187492079748282, 59.71276609431315308 ) ) ;
#9279 = PLANE ( 'NONE',  #7224 ) ;
#9280 = EDGE_CURVE ( 'NONE', #5788, #26302, #35153, .T. ) ;
#9281 = CARTESIAN_POINT ( 'NONE',  ( -24.44689184067228638, -14.18710713894228270, 69.93803194250308763 ) ) ;
#9282 = EDGE_CURVE ( 'NONE', #4206, #12395, #47961, .T. ) ;
#9283 = VERTEX_POINT ( 'NONE', #48072 ) ;
#9284 = CARTESIAN_POINT ( 'NONE',  ( -21.00534385541298121, -7.595227055684706130, 51.75156210489605257 ) ) ;
#9285 = CARTESIAN_POINT ( 'NONE',  ( -41.17556444364835500, -14.80920654474426534, 72.98823529411762934 ) ) ;
#9286 = B_SPLINE_CURVE_WITH_KNOTS ( 'NONE', 1,
 ( #17072, #5786 ),
 .UNSPECIFIED., .F., .F.,
 ( 2, 2 ),
 ( 0.000000000000000000, 1.000000000000000000 ),
 .UNSPECIFIED. ) ;
#9287 = CARTESIAN_POINT ( 'NONE',  ( -10.98710762053434387, -12.05856205565705785, 74.63128435701548824 ) ) ;
#9288 = CARTESIAN_POINT ( 'NONE',  ( -24.47380067112417734, -14.88812224869491807, 59.24859996059156231 ) ) ;
#9289 = ADVANCED_FACE ( 'NONE', ( #11373 ), #22217, .T. ) ;
#9290 = ORIENTED_EDGE ( 'NONE', *, *, #32043, .T. ) ;
#9291 = VECTOR ( 'NONE', #35317, 1000.000000000000000 ) ;
#9292 = FACE_OUTER_BOUND ( 'NONE', #29945, .T. ) ;
#9293 = AXIS2_PLACEMENT_3D ( 'NONE', #15776, #30348, #30832 ) ;
#9294 = CARTESIAN_POINT ( 'NONE',  ( -17.73278501768472992, -7.757988417614677168, 67.16472282884072342 ) ) ;
#9295 = CARTESIAN_POINT ( 'NONE',  ( -17.98078221672114552, -21.78831896835910698, 65.41702429779255112 ) ) ;
#9296 = ORIENTED_EDGE ( 'NONE', *, *, #35401, .T. ) ;
#9297 = CARTESIAN_POINT ( 'NONE',  ( -26.92409385541305511, -6.359206544744109735, 47.99999999999997868 ) ) ;
#9298 = AXIS2_PLACEMENT_3D ( 'NONE', #1541, #42682, #19786 ) ;
#9299 = AXIS2_PLACEMENT_3D ( 'NONE', #37062, #18589, #47922 ) ;
#9300 = ORIENTED_EDGE ( 'NONE', *, *, #3332, .F. ) ;
#9301 = CARTESIAN_POINT ( 'NONE',  ( -23.46260370332431577, -11.17067683354235719, 73.66193301755811262 ) ) ;
#9302 = FACE_OUTER_BOUND ( 'NONE', #15295, .T. ) ;
#9303 = ORIENTED_EDGE ( 'NONE', *, *, #1565, .F. ) ;
#9304 = CARTESIAN_POINT ( 'NONE',  ( -17.42409385541299471, -14.80920654474435771, 49.52966884056655772 ) ) ;
#9305 = CARTESIAN_POINT ( 'NONE',  ( -21.85024167232948855, -20.23279819819498115, 58.78059551072086464 ) ) ;
#9306 = FACE_OUTER_BOUND ( 'NONE', #25238, .T. ) ;
#9307 = LINE ( 'NONE', #5369, #47128 ) ;
#9308 = VERTEX_POINT ( 'NONE', #44630 ) ;
#9309 = CARTESIAN_POINT ( 'NONE',  ( -10.60635910294346651, -17.81289749453643978, 71.82364097624930821 ) ) ;
#9310 = VECTOR ( 'NONE', #14166, 1000.000000000000000 ) ;
#9311 = CARTESIAN_POINT ( 'NONE',  ( -20.88128654865952427, -21.40856141908871635, 58.68829242887799325 ) ) ;
#9312 =( BOUNDED_SURFACE ( )  B_SPLINE_SURFACE ( 3, 1, ( 
 ( #6629, #47742 ),
 ( #28058, #25104 ),
 ( #10332, #13512 ),
 ( #6145, #21645 ),
 ( #21167, #36633 ),
 ( #13030, #25343 ),
 ( #2915, #2449 ) ),
 .UNSPECIFIED., .T., .F., .F. ) 
 B_SPLINE_SURFACE_WITH_KNOTS ( ( 4, 3, 4 ),
 ( 2, 2 ),
 ( 0.000000000000000000, 0.5000000000000000000, 1.000000000000000000 ),
 ( 0.000000000000000000, 1.000000000000000000 ),
 .UNSPECIFIED. ) 
 GEOMETRIC_REPRESENTATION_ITEM ( )  RATIONAL_B_SPLINE_SURFACE ( (
 ( 1.000000000000000000, 1.000000000000000000),
 ( 0.3333333333333335369, 0.3333333333333330373),
 ( 0.3333333333333335369, 0.3333333333333330373),
 ( 1.000000000000000000, 1.000000000000000000),
 ( 0.3333333333333333703, 0.3333333333333333703),
 ( 0.3333333333333333703, 0.3333333333333333703),
 ( 1.000000000000000000, 1.000000000000000000) ) ) 
 REPRESENTATION_ITEM ( '' )  SURFACE ( )  );
#9313 = CARTESIAN_POINT ( 'NONE',  ( -23.45312108354205094, -19.18567332746851406, 62.55395650355025339 ) ) ;
#9314 = ORIENTED_EDGE ( 'NONE', *, *, #15185, .T. ) ;
#9315 = DIRECTION ( 'NONE',  ( 0.7700094066334510767, 0.6380325334150294125, 0.000000000000000000 ) ) ;
#9316 = CARTESIAN_POINT ( 'NONE',  ( -15.48424252676649182, -21.53505049348036948, 72.34575460973682937 ) ) ;
#9317 = VERTEX_POINT ( 'NONE', #33506 ) ;
#9318 = VERTEX_POINT ( 'NONE', #6953 ) ;
#9319 = CARTESIAN_POINT ( 'NONE',  ( -24.08907123645992243, -11.48026457312919391, 63.13713595337925000 ) ) ;
#9320 = CARTESIAN_POINT ( 'NONE',  ( -18.92409385541303024, -9.359200813967568422, 50.49621490985794026 ) ) ;
#9321 = DIRECTION ( 'NONE',  ( 1.000000000000000000, 0.000000000000000000, 0.000000000000000000 ) ) ;
#9322 = CARTESIAN_POINT ( 'NONE',  ( -17.57409385650551314, -9.792211528768504536, 50.49490371617623197 ) ) ;
#9323 = DIRECTION ( 'NONE',  ( 0.000000000000000000, 0.000000000000000000, 1.000000000000000000 ) ) ;
#9324 = EDGE_CURVE ( 'NONE', #14637, #16885, #27542, .T. ) ;
#9325 = CARTESIAN_POINT ( 'NONE',  ( -12.29706043583926345, -19.57525793408492731, 58.22682366956317424 ) ) ;
#9326 = CARTESIAN_POINT ( 'NONE',  ( -18.62171053289692324, -7.456047208065794685, 74.03402725549381103 ) ) ;
#9327 =( BOUNDED_CURVE ( )  B_SPLINE_CURVE ( 3, ( #17424, #31964, #43551, #24100 ),
 .UNSPECIFIED., .F., .F. ) 
 B_SPLINE_CURVE_WITH_KNOTS ( ( 4, 4 ),
 ( 0.5000000000000000000, 0.9074455897393693959 ),
 .UNSPECIFIED. ) 
 CURVE ( )  GEOMETRIC_REPRESENTATION_ITEM ( )  RATIONAL_B_SPLINE_CURVE ( ( 1.000000000000019318, 0.4567392136813193115, 0.3561768502900120592, 0.6983129098261183776 ) ) 
 REPRESENTATION_ITEM ( '' )  );
#9328 = CARTESIAN_POINT ( 'NONE',  ( -17.42409385541299471, -14.80920654474435771, 49.52966884056655772 ) ) ;
#9329 = EDGE_LOOP ( 'NONE', ( #1618, #24797 ) ) ;
#9330 = ORIENTED_EDGE ( 'NONE', *, *, #13611, .F. ) ;
#9331 = DIRECTION ( 'NONE',  ( 0.6408936281290996684, 0.7676297007174210929, 4.260501105223829223E-08 ) ) ;
#9332 = DIRECTION ( 'NONE',  ( 0.000000000000000000, 0.000000000000000000, 1.000000000000000000 ) ) ;
#9333 = CARTESIAN_POINT ( 'NONE',  ( -21.01124108229941001, -20.87838065962769463, 65.88453944495783787 ) ) ;
#9334 = CIRCLE ( 'NONE', #24270, 2.000000000000001332 ) ;
#9335 = CARTESIAN_POINT ( 'NONE',  ( -19.67760665824181388, -21.48965406232008490, 65.75014118398131302 ) ) ;
#9336 = CARTESIAN_POINT ( 'NONE',  ( -19.98813040044048606, -21.37641421727040125, 72.40478737316021807 ) ) ;
#9337 = DIRECTION ( 'NONE',  ( 0.9687793358424821033, -0.2479245821708677133, 0.000000000000000000 ) ) ;
#9338 = AXIS2_PLACEMENT_3D ( 'NONE', #18065, #9974, #17096 ) ;
#9339 = CIRCLE ( 'NONE', #15603, 0.4000000000000010214 ) ;
#9340 = EDGE_LOOP ( 'NONE', ( #3849, #22207, #12049, #29417, #46761 ) ) ;
#9341 = LINE ( 'NONE', #9824, #8378 ) ;
#9342 = CARTESIAN_POINT ( 'NONE',  ( -10.21398995055970893, -12.93320293812463007, 67.87685812613038649 ) ) ;
#9343 = EDGE_CURVE ( 'NONE', #29232, #38441, #37449, .T. ) ;
#9344 = FACE_OUTER_BOUND ( 'NONE', #4526, .T. ) ;
#9345 = CARTESIAN_POINT ( 'NONE',  ( -13.58034385541284195, -9.360768649639799932, 51.01397948905916735 ) ) ;
#9346 = CIRCLE ( 'NONE', #41567, 2.000000000000000444 ) ;
#9347 = EDGE_CURVE ( 'NONE', #32374, #40830, #22713, .T. ) ;
#9348 = ORIENTED_EDGE ( 'NONE', *, *, #13591, .T. ) ;
#9349 = CARTESIAN_POINT ( 'NONE',  ( -23.59167294107103530, -11.49507482056193197, 70.08137858863322833 ) ) ;
#9350 = EDGE_CURVE ( 'NONE', #47438, #24678, #26393, .T. ) ;
#9351 = CARTESIAN_POINT ( 'NONE',  ( -24.80769047312930553, -15.80232199467591947, 69.71802767292497549 ) ) ;
#9352 = CARTESIAN_POINT ( 'NONE',  ( -18.90996118681096405, -7.968724231816139536, 67.20071784163268092 ) ) ;
#9353 = CARTESIAN_POINT ( 'NONE',  ( -22.66918927228052283, -20.09991590937644901, 69.37406776248666063 ) ) ;
#9354 = EDGE_CURVE ( 'NONE', #4066, #31755, #27271, .T. ) ;
#9355 = CARTESIAN_POINT ( 'NONE',  ( -19.05654524761795443, -8.000564681511368903, 67.01144978564013854 ) ) ;
#9356 = ORIENTED_EDGE ( 'NONE', *, *, #6211, .T. ) ;
#9357 = DIRECTION ( 'NONE',  ( -3.549360974554993999E-17, 6.371834667797927122E-18, 1.000000000000000000 ) ) ;
#9358 = VERTEX_POINT ( 'NONE', #40672 ) ;
#9359 = DIRECTION ( 'NONE',  ( -2.723496480336737305E-06, -1.584719851758938193E-07, -0.9999999999962786434 ) ) ;
#9360 = DIRECTION ( 'NONE',  ( 0.9163203205182085531, 0.4004460890125010053, -2.380681616944615956E-09 ) ) ;
#9361 = ORIENTED_EDGE ( 'NONE', *, *, #1620, .F. ) ;
#9362 = CARTESIAN_POINT ( 'NONE',  ( -50.42609385541305755, -14.90920654474422058, 68.06470588235292496 ) ) ;
#9363 = CARTESIAN_POINT ( 'NONE',  ( -14.39909385650551776, -8.114302828567740988, 52.18300498402516041 ) ) ;
#9364 = AXIS2_PLACEMENT_3D ( 'NONE', #1963, #28063, #13034 ) ;
#9365 = ORIENTED_EDGE ( 'NONE', *, *, #1561, .F. ) ;
#9366 = CARTESIAN_POINT ( 'NONE',  ( -13.54823245630066175, -20.69819609872914157, 61.81646323537678001 ) ) ;
#9367 =( GEOMETRIC_REPRESENTATION_CONTEXT ( 3 ) GLOBAL_UNCERTAINTY_ASSIGNED_CONTEXT ( ( #26814 ) ) GLOBAL_UNIT_ASSIGNED_CONTEXT ( ( #11559, #45075, #12052 ) ) REPRESENTATION_CONTEXT ( 'NONE', 'WORKASPACE' ) );
#9368 = LINE ( 'NONE', #6633, #9464 ) ;
#9369 = CARTESIAN_POINT ( 'NONE',  ( -10.89683688409922269, -17.33836331364876315, 64.92739378817780960 ) ) ;
#9370 = ORIENTED_EDGE ( 'NONE', *, *, #14520, .T. ) ;
#9371 = CARTESIAN_POINT ( 'NONE',  ( -23.89126246139208121, -17.48811810169603831, 62.54649106506063561 ) ) ;
#9372 = VECTOR ( 'NONE', #12601, 1000.000000000000000 ) ;
#9373 = CARTESIAN_POINT ( 'NONE',  ( -11.47140389976542529, -10.32934621678965037, 74.69531023250135604 ) ) ;
#9374 = CARTESIAN_POINT ( 'NONE',  ( -24.02655296236175175, -11.35792967378293916, 66.53719098615387395 ) ) ;
#9375 = CARTESIAN_POINT ( 'NONE',  ( -20.78261577219678813, -20.95102001000085323, 62.41471427792803439 ) ) ;
#9376 = ORIENTED_EDGE ( 'NONE', *, *, #43442, .T. ) ;
#9377 = VERTEX_POINT ( 'NONE', #41406 ) ;
#9378 = CARTESIAN_POINT ( 'NONE',  ( -22.67332665777710332, -19.52078802573384664, 72.85220588380256856 ) ) ;
#9379 = FACE_OUTER_BOUND ( 'NONE', #36152, .T. ) ;
#9380 = ORIENTED_EDGE ( 'NONE', *, *, #21156, .F. ) ;
#9381 = VECTOR ( 'NONE', #38543, 1000.000000000000114 ) ;
#9382 = CARTESIAN_POINT ( 'NONE',  ( -17.54909385759799179, -8.112991634885936776, 51.74999426922421719 ) ) ;
#9383 = CARTESIAN_POINT ( 'NONE',  ( -23.83096212394601565, -11.00696669973021713, 73.52339839455761705 ) ) ;
#9384 = ADVANCED_FACE ( 'NONE', ( #36873 ), #47731, .T. ) ;
#9385 = CARTESIAN_POINT ( 'NONE',  ( -24.72409385541305582, -14.90920654474428630, 74.09999999999998010 ) ) ;
#9386 = EDGE_LOOP ( 'NONE', ( #39903, #12423 ) ) ;
#9387 = CARTESIAN_POINT ( 'NONE',  ( -16.79181145072023185, -21.83380975027498039, 65.11075561446135396 ) ) ;
#9388 = CARTESIAN_POINT ( 'NONE',  ( -19.43707224927095822, -8.044379180677138308, 63.57522333692026706 ) ) ;
#9389 = CARTESIAN_POINT ( 'NONE',  ( -16.19814381282456495, -21.75179583453235210, 58.58585572026734667 ) ) ;
#9390 = DIRECTION ( 'NONE',  ( 0.8858372764600319638, 0.4639960340712761533, -4.734734194490108743E-17 ) ) ;
#9391 = CYLINDRICAL_SURFACE ( 'NONE', #43432, 5.249999999999998224 ) ;
#9392 = EDGE_CURVE ( 'NONE', #8331, #38602, #13728, .T. ) ;
#9393 = ORIENTED_EDGE ( 'NONE', *, *, #26062, .F. ) ;
#9394 = EDGE_LOOP ( 'NONE', ( #2721, #26083, #45524, #37326 ) ) ;
#9395 = ORIENTED_EDGE ( 'NONE', *, *, #11731, .T. ) ;
#9396 = CARTESIAN_POINT ( 'NONE',  ( -10.83683317046381234, -12.44108562964681219, 57.62857332099802932 ) ) ;
#9397 = CARTESIAN_POINT ( 'NONE',  ( -22.57847124554494300, -10.07283119406621452, 70.29713180003925288 ) ) ;
#9398 = ADVANCED_FACE ( 'NONE', ( #25570 ), #25333, .T. ) ;
#9399 = VECTOR ( 'NONE', #16309, 1000.000000000000000 ) ;
#9400 = CARTESIAN_POINT ( 'NONE',  ( -10.98483237281456404, -18.55601372762673407, 57.90690960667243559 ) ) ;
#9401 =( BOUNDED_SURFACE ( )  B_SPLINE_SURFACE ( 3, 1, ( 
 ( #33450, #18688 ),
 ( #25131, #44105 ),
 ( #18202, #48014 ),
 ( #33210, #10358 ),
 ( #40149, #36426 ),
 ( #7146, #25370 ),
 ( #6414, #11078 ) ),
 .UNSPECIFIED., .T., .F., .F. ) 
 B_SPLINE_SURFACE_WITH_KNOTS ( ( 4, 3, 4 ),
 ( 2, 2 ),
 ( 0.000000000000000000, 0.5000000000000000000, 1.000000000000000000 ),
 ( 0.000000000000000000, 1.000000000000000000 ),
 .UNSPECIFIED. ) 
 GEOMETRIC_REPRESENTATION_ITEM ( )  RATIONAL_B_SPLINE_SURFACE ( (
 ( 1.000000000000000000, 1.000000000000000000),
 ( 0.3333333333333335369, 0.3333333333333330373),
 ( 0.3333333333333335369, 0.3333333333333330373),
 ( 1.000000000000000000, 1.000000000000000000),
 ( 0.3333333333333333703, 0.3333333333333333703),
 ( 0.3333333333333333703, 0.3333333333333333703),
 ( 1.000000000000000000, 1.000000000000000000) ) ) 
 REPRESENTATION_ITEM ( '' )  SURFACE ( )  );
#9402 = ORIENTED_EDGE ( 'NONE', *, *, #25351, .F. ) ;
#9403 = AXIS2_PLACEMENT_3D ( 'NONE', #43365, #31543, #35696 ) ;
#9404 = CARTESIAN_POINT ( 'NONE',  ( -21.95523233784883033, -8.895446131873137929, 66.77654700642760588 ) ) ;
#9405 = EDGE_CURVE ( 'NONE', #31463, #47353, #30459, .T. ) ;
#9406 = CARTESIAN_POINT ( 'NONE',  ( -10.38423141237398895, -15.23952324640539935, 57.98281521108167880 ) ) ;
#9407 = ORIENTED_EDGE ( 'NONE', *, *, #40432, .F. ) ;
#9408 = CARTESIAN_POINT ( 'NONE',  ( -11.42787535746950667, -18.52272177604094239, 57.69225786326394001 ) ) ;
#9409 = AXIS2_PLACEMENT_3D ( 'NONE', #32614, #6027, #13639 ) ;
#9410 = ADVANCED_FACE ( 'NONE', ( #10072 ), #9607, .T. ) ;
#9411 = CARTESIAN_POINT ( 'NONE',  ( -10.46342116995388061, -14.06823698635533759, 57.55710969353301465 ) ) ;
#9412 = EDGE_LOOP ( 'NONE', ( #19311, #46300 ) ) ;
#9413 = CARTESIAN_POINT ( 'NONE',  ( -21.91761355075745854, -8.866908028128893449, 66.86138764422409508 ) ) ;
#9414 = ORIENTED_EDGE ( 'NONE', *, *, #42422, .T. ) ;
#9415 = DIRECTION ( 'NONE',  ( 1.000000000000000000, 1.669677910507523057E-21, 6.493791346278465266E-22 ) ) ;
#9416 = ORIENTED_EDGE ( 'NONE', *, *, #44339, .T. ) ;
#9417 = CARTESIAN_POINT ( 'NONE',  ( -17.42409385541299471, -14.80920654474434883, 62.02966884056656482 ) ) ;
#9418 = CARTESIAN_POINT ( 'NONE',  ( -50.42609385541305755, -14.80920654474423159, 69.07058823529411029 ) ) ;
#9419 = CARTESIAN_POINT ( 'NONE',  ( -21.04131466462198574, -20.86482832106620933, 62.11471242509498580 ) ) ;
#9420 = VERTEX_POINT ( 'NONE', #43334 ) ;
#9421 = CARTESIAN_POINT ( 'NONE',  ( -17.85555652284939043, -7.772123375420258107, 60.09532845646905486 ) ) ;
#9422 = FACE_OUTER_BOUND ( 'NONE', #32956, .T. ) ;
#9423 = CARTESIAN_POINT ( 'NONE',  ( -22.19982498210932675, -20.00606685933203366, 58.92009921125114857 ) ) ;
#9424 = EDGE_CURVE ( 'NONE', #36602, #32895, #18141, .T. ) ;
#9425 = CARTESIAN_POINT ( 'NONE',  ( -19.80301194551662647, -21.44571530912114099, 68.93482476707502826 ) ) ;
#9426 = DIRECTION ( 'NONE',  ( -3.071710424422018668E-17, 6.404604876783312462E-16, 1.000000000000000000 ) ) ;
#9427 = CARTESIAN_POINT ( 'NONE',  ( -10.39215589072981416, -14.30487699944780289, 64.68803863382906627 ) ) ;
#9428 = ORIENTED_EDGE ( 'NONE', *, *, #11661, .F. ) ;
#9429 = FACE_OUTER_BOUND ( 'NONE', #24035, .T. ) ;
#9430 = ADVANCED_FACE ( 'NONE', ( #17195 ), #17681, .T. ) ;
#9431 = DIRECTION ( 'NONE',  ( 0.9466432954593471116, 0.3222832157619555660, 8.771047036255756069E-09 ) ) ;
#9432 = CARTESIAN_POINT ( 'NONE',  ( -24.30112618867181240, -13.25578303422174997, 59.64795780745660636 ) ) ;
#9433 = CARTESIAN_POINT ( 'NONE',  ( -23.58616457878146377, -18.99640866789479432, 66.00884704819274873 ) ) ;
#9434 = CARTESIAN_POINT ( 'NONE',  ( -19.94963503706584973, -21.81807911492407825, 69.03458852897473719 ) ) ;
#9435 = ADVANCED_FACE ( 'NONE', ( #36151 ), #2439, .F. ) ;
#9436 = CARTESIAN_POINT ( 'NONE',  ( -15.60534385650552025, -8.801233750844183135, 48.81488406609782515 ) ) ;
#9437 = ORIENTED_EDGE ( 'NONE', *, *, #45815, .F. ) ;
#9438 = AXIS2_PLACEMENT_3D ( 'NONE', #46417, #31873, #5783 ) ;
#9439 = CARTESIAN_POINT ( 'NONE',  ( -22.02670722051955465, -15.75340237016373202, 52.02966884056656482 ) ) ;
#9440 = CARTESIAN_POINT ( 'NONE',  ( -20.75354924259569245, -21.52967727414722532, 53.49999999999994316 ) ) ;
#9441 = VERTEX_POINT ( 'NONE', #44069 ) ;
#9442 = CARTESIAN_POINT ( 'NONE',  ( -11.37476892658000160, -19.15884210479704208, 68.33034228280476441 ) ) ;
#9443 = DIRECTION ( 'NONE',  ( -0.2737502900231349456, -0.9618007999124592589, 5.400150802763565238E-08 ) ) ;
#9444 = CARTESIAN_POINT ( 'NONE',  ( -11.60526899143904345, -18.79015832504765626, 68.23161775275829655 ) ) ;
#9445 = CARTESIAN_POINT ( 'NONE',  ( -18.47409385541327964, -6.859212275519742441, 50.50378509014038997 ) ) ;
#9446 = LINE ( 'NONE', #24937, #25032 ) ;
#9447 = EDGE_LOOP ( 'NONE', ( #45798, #47356, #11485, #14983 ) ) ;
#9448 = CARTESIAN_POINT ( 'NONE',  ( -23.71873335871097410, -11.74668215431234586, 62.95218284853060453 ) ) ;
#9449 = AXIS2_PLACEMENT_3D ( 'NONE', #47652, #21559, #17106 ) ;
#9450 = CARTESIAN_POINT ( 'NONE',  ( -16.56761320685650318, -19.87745396966068157, 52.02966884056656482 ) ) ;
#9451 = CARTESIAN_POINT ( 'NONE',  ( -22.11565237232494496, -20.07634252930852981, 58.97262747901392288 ) ) ;
#9452 = ORIENTED_EDGE ( 'NONE', *, *, #22163, .T. ) ;
#9453 = DIRECTION ( 'NONE',  ( -0.7489133456531319455, -0.6626679415081375701, 6.686399169904807035E-09 ) ) ;
#9454 = AXIS2_PLACEMENT_3D ( 'NONE', #14308, #58, #29358 ) ;
#9455 = CARTESIAN_POINT ( 'NONE',  ( -13.37043874031056490, -9.101841881849773941, 63.92563223505148784 ) ) ;
#9456 = CARTESIAN_POINT ( 'NONE',  ( -24.20371252810814866, -12.87440185077122834, 66.58774614429587757 ) ) ;
#9457 =( BOUNDED_CURVE ( )  B_SPLINE_CURVE ( 3, ( #30063, #33464, #22923, #38148 ),
 .UNSPECIFIED., .F., .F. ) 
 B_SPLINE_CURVE_WITH_KNOTS ( ( 4, 4 ),
 ( 0.4074455897393656212, 0.5000000000000000000 ),
 .UNSPECIFIED. ) 
 CURVE ( )  GEOMETRIC_REPRESENTATION_ITEM ( )  RATIONAL_B_SPLINE_CURVE ( ( 0.6983129098260936196, 0.7760317562606803277, 0.8765941196519769774, 0.9999999999999708011 ) ) 
 REPRESENTATION_ITEM ( '' )  );
#9458 = DIRECTION ( 'NONE',  ( 0.3667195576449455152, -0.9303315355510074491, -1.591455084066187253E-08 ) ) ;
#9459 = CARTESIAN_POINT ( 'NONE',  ( -21.82233664355339542, -16.46178511230714037, 49.52966884056655772 ) ) ;
#9460 = ORIENTED_EDGE ( 'NONE', *, *, #22169, .T. ) ;
#9461 = ORIENTED_EDGE ( 'NONE', *, *, #23526, .T. ) ;
#9462 = CARTESIAN_POINT ( 'NONE',  ( -18.19284385541304161, -8.630756214087126565, 51.74842643355248129 ) ) ;
#9463 = DIRECTION ( 'NONE',  ( 1.616182858256114592E-16, 0.003028072113811714535, -0.9999954153791273948 ) ) ;
#9464 = VECTOR ( 'NONE', #29032, 1000.000000000000114 ) ;
#9465 = B_SPLINE_CURVE_WITH_KNOTS ( 'NONE', 3,
 ( #6300, #42997, #47429, #9273, #31678, #20354, #46467, #46933, #32409, #28476 ),
 .UNSPECIFIED., .F., .F.,
 ( 4, 2, 2, 2, 4 ),
 ( 0.000000000000000000, 0.2500000000000000000, 0.5000000000000000000, 0.7500000000000000000, 1.000000000000000000 ),
 .UNSPECIFIED. ) ;
#9466 = CARTESIAN_POINT ( 'NONE',  ( -12.42812249138612835, -20.42751868149720096, 53.76227901944322696 ) ) ;
#9467 = CARTESIAN_POINT ( 'NONE',  ( -12.09966231065201825, -10.17612992894743229, 71.11326093460978370 ) ) ;
#9468 =( BOUNDED_CURVE ( )  B_SPLINE_CURVE ( 2, ( #43723, #22269, #7268, #21779, #44446, #36304, #10696, #18308, #6767 ),
 .UNSPECIFIED., .F., .F. ) 
 B_SPLINE_CURVE_WITH_KNOTS ( ( 3, 2, 2, 2, 3 ),
 ( 0.04720854346325247669, 0.04819199384251378337, 0.04917544422177509700, 0.05015889460103639674, 0.05114234498029770343 ),
 .UNSPECIFIED. ) 
 CURVE ( )  GEOMETRIC_REPRESENTATION_ITEM ( )  RATIONAL_B_SPLINE_CURVE ( ( 0.9999999999999715783, 0.9238795325113151602, 1.000000000000000000, 0.9238795325112867385, 1.000000000000000000, 0.9238795325112867385, 1.000000000000000000, 0.9238795325108096756, 1.000000000000476952 ) ) 
 REPRESENTATION_ITEM ( '' )  );
#9469 = EDGE_CURVE ( 'NONE', #48485, #9377, #40787, .T. ) ;
#9470 = CARTESIAN_POINT ( 'NONE',  ( -14.15319410108614129, -8.620341405635986831, 70.80245711640594664 ) ) ;
#9471 = CYLINDRICAL_SURFACE ( 'NONE', #8128, 0.1500000000000067668 ) ;
#9472 = ORIENTED_EDGE ( 'NONE', *, *, #33306, .F. ) ;
#9473 = CIRCLE ( 'NONE', #4756, 2.000000000000000888 ) ;
#9474 = CARTESIAN_POINT ( 'NONE',  ( -21.11381757457507646, -20.75781470100932680, 65.69339893210704417 ) ) ;
#9475 = AXIS2_PLACEMENT_3D ( 'NONE', #29391, #15078, #7487 ) ;
#9476 = CYLINDRICAL_SURFACE ( 'NONE', #40625, 0.1500000000000049349 ) ;
#9477 = VERTEX_POINT ( 'NONE', #24852 ) ;
#9478 = FACE_OUTER_BOUND ( 'NONE', #17649, .T. ) ;
#9479 = VECTOR ( 'NONE', #1631, 1000.000000000000227 ) ;
#9480 = CARTESIAN_POINT ( 'NONE',  ( -11.92656900268342035, -15.22777080260183169, 53.88362224778186516 ) ) ;
#9481 =( BOUNDED_CURVE ( )  B_SPLINE_CURVE ( 3, ( #36606, #2887, #47959, #29735 ),
 .UNSPECIFIED., .F., .F. ) 
 B_SPLINE_CURVE_WITH_KNOTS ( ( 4, 4 ),
 ( 0.5000000000000000000, 0.9074455897393665094 ),
 .UNSPECIFIED. ) 
 CURVE ( )  GEOMETRIC_REPRESENTATION_ITEM ( )  RATIONAL_B_SPLINE_CURVE ( ( 0.9999999999999996669, 0.4567392136813316350, 0.3561768502900302114, 0.6983129098260952849 ) ) 
 REPRESENTATION_ITEM ( '' )  );
#9482 = EDGE_LOOP ( 'NONE', ( #41171, #19535, #8400, #28358, #43335 ) ) ;
#9483 = LINE ( 'NONE', #3032, #42474 ) ;
#9484 = PLANE ( 'NONE',  #641 ) ;
#9485 = EDGE_LOOP ( 'NONE', ( #655, #1742 ) ) ;
#9486 = CARTESIAN_POINT ( 'NONE',  ( -17.84905175390062837, -22.24782703323402444, 58.51898120184483076 ) ) ;
#9487 = CARTESIAN_POINT ( 'NONE',  ( -19.57699614054808634, -21.94144247634149281, 62.17999043330664222 ) ) ;
#9488 = VECTOR ( 'NONE', #40551, 1000.000000000000114 ) ;
#9489 = CYLINDRICAL_SURFACE ( 'NONE', #34492, 5.249999999999998224 ) ;
#9490 = CARTESIAN_POINT ( 'NONE',  ( -11.22844613476422282, -11.44458948612160221, 64.43409918096024569 ) ) ;
#9491 = ORIENTED_EDGE ( 'NONE', *, *, #15666, .T. ) ;
#9492 = DIRECTION ( 'NONE',  ( -6.446466763177039895E-06, 1.047023821809670710E-05, 0.9999999999244085780 ) ) ;
#9493 = CYLINDRICAL_SURFACE ( 'NONE', #19510, 4.686499999999997002 ) ;
#9494 = CARTESIAN_POINT ( 'NONE',  ( -16.98991614605047218, -22.24663000551990777, 72.35038637723081933 ) ) ;
#9495 = EDGE_CURVE ( 'NONE', #44063, #38493, #32705, .T. ) ;
#9496 = CARTESIAN_POINT ( 'NONE',  ( -18.55662820153069248, -10.26160847489872374, 49.52966884056655772 ) ) ;
#9497 = EDGE_CURVE ( 'NONE', #31797, #9250, #3393, .T. ) ;
#9498 = EDGE_CURVE ( 'NONE', #15459, #8859, #25092, .T. ) ;
#9499 = DIRECTION ( 'NONE',  ( 0.06357898915123501304, -0.9979768094191904249, 0.000000000000000000 ) ) ;
#9500 = CARTESIAN_POINT ( 'NONE',  ( -11.44117212203710032, -11.17454305509652634, 60.69502469113133714 ) ) ;
#9501 = CLOSED_SHELL ( 'NONE', ( #4705, #45294, #39550, #40874, #47027, #1206, #22024, #6233, #21624, #3610, #20114, #25033, #5169, #31215, #30850, #38442, #48572, #44056, #40644, #35283, #19024, #24014, #38093, #11064, #39206, #11174, #23756, #5553, #6487, #2156, #20729, #489, #34395, #836, #23556, #38157, #2172, #48543, #4544, #23617, #36992, #26353, #6820, #24965, #30064, #11215, #17555, #8213, #2557, #17240, #25758, #27743, #15194, #41695, #5774, #45691, #38020, #26583, #39855, #41872, #19012, #23144, #3539, #46010, #26601, #360, #30014, #35373, #17328, #37130, #30969, #27214, #12344, #26261, #6493, #2363, #46162, #37110, #6087, #7716, #17578, #47055, #33457, #29511, #25537, #26242, #30909, #908, #33541, #46594, #46724, #12004, #45768, #19789, #6959, #21125, #10246, #31272, #409, #12044, #8805, #40164, #36421, #15931, #45764, #36145, #45723, #35958, #889, #42006, #25972, #43811, #38638, #758, #14289, #703, #33584, #1500, #33808, #41731, #29097, #28097, #11268, #1576, #48688, #31077, #46592, #13285, #21990, #37406, #14457, #24885, #29732, #16543, #24696, #29734, #48183, #36222, #24012, #12997, #12203, #14615, #15045, #7409, #43178, #21464, #30474, #46531, #22720, #17012, #36322, #358, #35302, #12204, #20103, #40507, #4841, #24959, #159, #6419, #42998, #16585, #30157, #16893, #31069, #9983, #29769, #27132, #40214 ) ) ;
#9502 = DIRECTION ( 'NONE',  ( -0.09077643883959131410, 0.9958712959773468043, 4.338678762321648664E-08 ) ) ;
#9503 = EDGE_LOOP ( 'NONE', ( #22385, #32622, #21112, #18164, #20398 ) ) ;
#9504 = DIRECTION ( 'NONE',  ( 0.9687793358424821033, -0.2479245821708679909, 0.000000000000000000 ) ) ;
#9505 = CARTESIAN_POINT ( 'NONE',  ( -14.30193168523162761, -8.044807666815707137, 67.42121571432790006 ) ) ;
#9506 = CARTESIAN_POINT ( 'NONE',  ( -24.07704370891654122, -17.14264987453632827, 72.89808101046213551 ) ) ;
#9507 = EDGE_LOOP ( 'NONE', ( #178, #29217, #29700, #47309, #37899 ) ) ;
#9508 = CARTESIAN_POINT ( 'NONE',  ( -15.06493049075016977, -21.45670177733324380, 68.87592999875900546 ) ) ;
#9509 = ORIENTED_EDGE ( 'NONE', *, *, #25084, .T. ) ;
#9510 = ORIENTED_EDGE ( 'NONE', *, *, #22788, .F. ) ;
#9511 = ORIENTED_EDGE ( 'NONE', *, *, #11919, .T. ) ;
#9512 = CARTESIAN_POINT ( 'NONE',  ( -18.81428322969336620, -7.490049256398734201, 70.47093791628151394 ) ) ;
#9513 = DIRECTION ( 'NONE',  ( -0.3996021513128670266, -0.9166886716143755054, -9.834836654444679756E-09 ) ) ;
#9514 = CARTESIAN_POINT ( 'NONE',  ( -16.50530592306966682, -19.40475993746870387, 49.52966884056656482 ) ) ;
#9515 = CARTESIAN_POINT ( 'NONE',  ( 18.46573386768564973, 3.116243883476752963, 50.28399048308536123 ) ) ;
#9516 = CYLINDRICAL_SURFACE ( 'NONE', #4773, 2.000000000000001332 ) ;
#9517 = VECTOR ( 'NONE', #43744, 1000.000000000000000 ) ;
#9518 = ORIENTED_EDGE ( 'NONE', *, *, #44068, .F. ) ;
#9519 = ORIENTED_EDGE ( 'NONE', *, *, #42342, .T. ) ;
#9520 = CARTESIAN_POINT ( 'NONE',  ( -19.01159385650551670, -6.922745924619793101, 51.69366785382590024 ) ) ;
#9521 = EDGE_CURVE ( 'NONE', #1086, #39806, #36624, .T. ) ;
#9522 = DIRECTION ( 'NONE',  ( -2.161108586189011127E-06, -4.147204437186874712E-06, -0.9999999999890651914 ) ) ;
#9523 = DIRECTION ( 'NONE',  ( 3.071710424422018668E-17, -6.404604876783312462E-16, -1.000000000000000000 ) ) ;
#9524 = AXIS2_PLACEMENT_3D ( 'NONE', #47657, #48140, #17835 ) ;
#9525 = CARTESIAN_POINT ( 'NONE',  ( -11.79630000206883977, -19.05592701419838519, 71.97213747039440079 ) ) ;
#9526 = CARTESIAN_POINT ( 'NONE',  ( -22.49909385650551741, -8.114302828567740988, 52.18300498402516041 ) ) ;
#9527 = ORIENTED_EDGE ( 'NONE', *, *, #44583, .F. ) ;
#9528 = CARTESIAN_POINT ( 'NONE',  ( -12.27729947935473653, -9.991218615320079266, 60.85918086709605745 ) ) ;
#9529 = DIRECTION ( 'NONE',  ( 0.1464579420318390945, -0.9892168979631278392, -7.284849527857772841E-08 ) ) ;
#9530 = CIRCLE ( 'NONE', #46472, 2.000000000000000888 ) ;
#9531 = LINE ( 'NONE', #6551, #9517 ) ;
#9532 = ORIENTED_EDGE ( 'NONE', *, *, #19917, .F. ) ;
#9533 = B_SPLINE_CURVE_WITH_KNOTS ( 'NONE', 3,
 ( #25301, #7073, #10030, #17151, #13934, #6338, #10751, #24813, #32674, #25056 ),
 .UNSPECIFIED., .F., .F.,
 ( 4, 2, 2, 2, 4 ),
 ( 0.6272669072877784524, 0.7522669073072748569, 0.8772669073267711504, 1.002266907346267555, 1.127266907365763959 ),
 .UNSPECIFIED. ) ;
#9534 = CARTESIAN_POINT ( 'NONE',  ( -11.59752488401249160, -18.69167939738282413, 68.40616817336767497 ) ) ;
#9535 = B_SPLINE_CURVE_WITH_KNOTS ( 'NONE', 1,
 ( #7420, #26361 ),
 .UNSPECIFIED., .F., .F.,
 ( 2, 2 ),
 ( 0.000000000000000000, 1.000000000000000000 ),
 .UNSPECIFIED. ) ;
#9536 = AXIS2_PLACEMENT_3D ( 'NONE', #24782, #9990, #28223 ) ;
#9537 = CARTESIAN_POINT ( 'NONE',  ( -23.78500266573477262, -11.88707733699690827, 59.78235732566622573 ) ) ;
#9538 = CARTESIAN_POINT ( 'NONE',  ( -11.04141237841800560, -11.93494539390495568, 74.85840195306853673 ) ) ;
#9539 = CARTESIAN_POINT ( 'NONE',  ( -18.85724798917316392, -7.906108138700305155, 67.18599644112759961 ) ) ;
#9540 = AXIS2_PLACEMENT_3D ( 'NONE', #35866, #6333, #13930 ) ;
#9541 = ORIENTED_EDGE ( 'NONE', *, *, #8305, .T. ) ;
#9542 = CYLINDRICAL_SURFACE ( 'NONE', #40703, 0.1500000000000017153 ) ;
#9543 = FACE_OUTER_BOUND ( 'NONE', #37135, .T. ) ;
#9544 = ORIENTED_EDGE ( 'NONE', *, *, #18392, .T. ) ;
#9545 = CARTESIAN_POINT ( 'NONE',  ( -24.82717143659370507, -15.64415108208998539, 73.10329505203212364 ) ) ;
#9546 = VECTOR ( 'NONE', #3280, 1000.000000000000000 ) ;
#9547 = ORIENTED_EDGE ( 'NONE', *, *, #15031, .F. ) ;
#9548 = CARTESIAN_POINT ( 'NONE',  ( -11.76616827618561878, -10.68746712392528764, 74.72419580846755593 ) ) ;
#9549 = DIRECTION ( 'NONE',  ( -3.071710424422018668E-17, 6.404604876783312462E-16, 1.000000000000000000 ) ) ;
#9550 = ORIENTED_EDGE ( 'NONE', *, *, #15725, .F. ) ;
#9551 = EDGE_CURVE ( 'NONE', #8240, #39661, #8435, .T. ) ;
#9552 = CYLINDRICAL_SURFACE ( 'NONE', #38379, 7.500000000000001776 ) ;
#9553 = CARTESIAN_POINT ( 'NONE',  ( -12.84719740098974583, -9.512790884556105553, 74.61923006383901225 ) ) ;
#9554 = CARTESIAN_POINT ( 'NONE',  ( -24.20877031762658049, -12.89276232856998661, 66.59686929038259962 ) ) ;
#9555 = B_SPLINE_CURVE_WITH_KNOTS ( 'NONE', 3,
 ( #13836, #36489, #2770, #3008, #43434, #9704, #24720, #5987, #21015, #2294 ),
 .UNSPECIFIED., .F., .F.,
 ( 4, 2, 2, 2, 4 ),
 ( 0.6272669072877555818, 0.7522669073072774104, 0.8772669073267993500, 1.002266907346321290, 1.127266907365843007 ),
 .UNSPECIFIED. ) ;
#9556 = DIRECTION ( 'NONE',  ( 0.000000000000000000, 1.000000000000000000, 0.000000000000000000 ) ) ;
#9557 = ORIENTED_EDGE ( 'NONE', *, *, #24060, .T. ) ;
#9558 = CYLINDRICAL_SURFACE ( 'NONE', #17386, 7.500000000000001776 ) ;
#9559 = CIRCLE ( 'NONE', #31548, 5.249999999999998224 ) ;
#9560 = CARTESIAN_POINT ( 'NONE',  ( -15.12736045941317897, -21.89643407171298151, 68.69097498501147925 ) ) ;
#9561 = LINE ( 'NONE', #39579, #37664 ) ;
#9562 = VERTEX_POINT ( 'NONE', #43816 ) ;
#9563 = CARTESIAN_POINT ( 'NONE',  ( -10.61641583932764910, -11.78277314028518319, 74.74335662173743344 ) ) ;
#9564 = ADVANCED_FACE ( 'NONE', ( #22608 ), #11288, .T. ) ;
#9565 = EDGE_CURVE ( 'NONE', #34714, #6531, #44051, .T. ) ;
#9566 = CARTESIAN_POINT ( 'NONE',  ( -11.10470733248389230, -18.75498039752055490, 61.46206112672981448 ) ) ;
#9568 = ORIENTED_EDGE ( 'NONE', *, *, #20848, .T. ) ;
#9567 = CIRCLE ( 'NONE', #48074, 4.686499999999999666 ) ;
#9569 = ORIENTED_EDGE ( 'NONE', *, *, #42763, .F. ) ;
#9570 = EDGE_CURVE ( 'NONE', #9308, #30495, #37866, .T. ) ;
#9571 = DIRECTION ( 'NONE',  ( -0.9956360040033418457, 0.09332174201255234725, 0.000000000000000000 ) ) ;
#9572 = LINE ( 'NONE', #13471, #37580 ) ;
#9573 = CARTESIAN_POINT ( 'NONE',  ( -21.08382089131013259, -22.19632712819893428, 53.49999999999995026 ) ) ;
#9574 = CARTESIAN_POINT ( 'NONE',  ( -19.43034385650552309, -9.794322478646142471, 51.19202720610083901 ) ) ;
#9575 = ADVANCED_FACE ( 'NONE', ( #4379 ), #33413, .F. ) ;
#9576 = CARTESIAN_POINT ( 'NONE',  ( -12.44869033171645611, -9.885248809711741913, 57.38935532200543577 ) ) ;
#9577 = CYLINDRICAL_SURFACE ( 'NONE', #5925, 0.1500000000000007161 ) ;
#9578 = DIRECTION ( 'NONE',  ( -0.9294853595766571219, -0.3688590060343552857, 0.000000000000000000 ) ) ;
#9579 = CARTESIAN_POINT ( 'NONE',  ( -10.99582063857411995, -11.91441743271276188, 74.55840195587596497 ) ) ;
#9580 = CARTESIAN_POINT ( 'NONE',  ( -13.83778161524790384, -21.33926439188370594, 72.03333559426305044 ) ) ;
#9581 = ORIENTED_EDGE ( 'NONE', *, *, #35320, .T. ) ;
#9582 = ORIENTED_EDGE ( 'NONE', *, *, #8938, .T. ) ;
#9584 = CARTESIAN_POINT ( 'NONE',  ( -18.79049830835916524, -7.892586073225762000, 70.38540174208183942 ) ) ;
#9583 = CIRCLE ( 'NONE', #30803, 2.500000000000002220 ) ;
#9585 = ADVANCED_FACE ( 'NONE', ( #14687 ), #38098, .T. ) ;
#9586 = DIRECTION ( 'NONE',  ( 1.000000000000000000, 0.000000000000000000, 0.000000000000000000 ) ) ;
#9587 = CARTESIAN_POINT ( 'NONE',  ( -22.10255287824656989, -12.42708119714673742, 49.52966884056655772 ) ) ;
#9588 = CARTESIAN_POINT ( 'NONE',  ( -16.01712388020451883, -7.950755688058114501, 67.36837251840358931 ) ) ;
#9589 = LINE ( 'NONE', #24605, #29561 ) ;
#9590 = CARTESIAN_POINT ( 'NONE',  ( -20.94477883430487708, -21.37566986424753068, 58.75819861804361466 ) ) ;
#9591 = ORIENTED_EDGE ( 'NONE', *, *, #28024, .T. ) ;
#9592 = PLANE ( 'NONE',  #17784 ) ;
#9593 = CARTESIAN_POINT ( 'NONE',  ( -10.23043904185361086, -12.87167706366568787, 67.83858103935695283 ) ) ;
#9594 = CARTESIAN_POINT ( 'NONE',  ( -14.60479746972646886, -7.913168098764732150, 60.50491608655884335 ) ) ;
#9595 = CARTESIAN_POINT ( 'NONE',  ( -19.44376929052122449, -7.638105555415076076, 60.07597592072836790 ) ) ;
#9596 = CIRCLE ( 'NONE', #37077, 5.249999999999998224 ) ;
#9597 =( BOUNDED_SURFACE ( )  B_SPLINE_SURFACE ( 3, 1, ( 
 ( #15525, #30590 ),
 ( #34495, #19739 ),
 ( #4464, #11865 ),
 ( #12103, #30833 ),
 ( #12339, #41902 ),
 ( #8660, #45848 ),
 ( #42144, #38429 ) ),
 .UNSPECIFIED., .T., .F., .F. ) 
 B_SPLINE_SURFACE_WITH_KNOTS ( ( 4, 3, 4 ),
 ( 2, 2 ),
 ( 0.000000000000000000, 0.5000000000000000000, 1.000000000000000000 ),
 ( 0.000000000000000000, 1.000000000000000000 ),
 .UNSPECIFIED. ) 
 GEOMETRIC_REPRESENTATION_ITEM ( )  RATIONAL_B_SPLINE_SURFACE ( (
 ( 1.000000000000000000, 1.000000000000000000),
 ( 0.3333333333333335369, 0.3333333333333330373),
 ( 0.3333333333333335369, 0.3333333333333330373),
 ( 1.000000000000000000, 1.000000000000000000),
 ( 0.3333333333333333703, 0.3333333333333333703),
 ( 0.3333333333333333703, 0.3333333333333333703),
 ( 1.000000000000000000, 1.000000000000000000) ) ) 
 REPRESENTATION_ITEM ( '' )  SURFACE ( )  );
#9598 = ORIENTED_EDGE ( 'NONE', *, *, #7017, .F. ) ;
#9599 = CARTESIAN_POINT ( 'NONE',  ( -11.49688049385021138, -18.62690763749001732, 64.76179218520604763 ) ) ;
#9600 = CARTESIAN_POINT ( 'NONE',  ( -16.60428136649079534, -9.623610389719635450, 49.52966884056655772 ) ) ;
#9601 = CARTESIAN_POINT ( 'NONE',  ( -41.04982914953070861, -14.90920654474427565, 73.99411764705880046 ) ) ;
#9602 = CARTESIAN_POINT ( 'NONE',  ( -45.37196614242555626, -14.20920654474410760, 70.87000000000000455 ) ) ;
#9603 = CARTESIAN_POINT ( 'NONE',  ( -17.00410685006708178, -7.771727545396207582, 73.96018273221115180 ) ) ;
#9604 = CARTESIAN_POINT ( 'NONE',  ( -14.80727700386144186, -7.833856537212772864, 56.95661706491381437 ) ) ;
#9605 = EDGE_CURVE ( 'NONE', #19379, #596, #4642, .T. ) ;
#9606 =( BOUNDED_SURFACE ( )  B_SPLINE_SURFACE ( 3, 1, ( 
 ( #4230, #27351 ),
 ( #19239, #41896 ),
 ( #19971, #42384 ),
 ( #34002, #30343 ),
 ( #23917, #34241 ),
 ( #26635, #41650 ),
 ( #23425, #38918 ) ),
 .UNSPECIFIED., .T., .F., .F. ) 
 B_SPLINE_SURFACE_WITH_KNOTS ( ( 4, 3, 4 ),
 ( 2, 2 ),
 ( 0.000000000000000000, 0.5000000000000000000, 1.000000000000000000 ),
 ( 0.000000000000000000, 1.000000000000000000 ),
 .UNSPECIFIED. ) 
 GEOMETRIC_REPRESENTATION_ITEM ( )  RATIONAL_B_SPLINE_SURFACE ( (
 ( 1.000000000000000000, 1.000000000000000000),
 ( 0.3333333333333335369, 0.3333333333333330373),
 ( 0.3333333333333335369, 0.3333333333333330373),
 ( 1.000000000000000000, 1.000000000000000000),
 ( 0.3333333333333333703, 0.3333333333333333703),
 ( 0.3333333333333333703, 0.3333333333333333703),
 ( 1.000000000000000000, 1.000000000000000000) ) ) 
 REPRESENTATION_ITEM ( '' )  SURFACE ( )  );
#9607 = CYLINDRICAL_SURFACE ( 'NONE', #6307, 0.1499999999999975242 ) ;
#9608 = EDGE_LOOP ( 'NONE', ( #22925, #14156, #627, #39821, #40220 ) ) ;
#9609 = CARTESIAN_POINT ( 'NONE',  ( -20.91839308061383562, -20.87517752881106503, 65.60070617543843241 ) ) ;
#9610 = ORIENTED_EDGE ( 'NONE', *, *, #33166, .F. ) ;
#9611 = CARTESIAN_POINT ( 'NONE',  ( -11.33040464740410158, -19.09525857600861798, 68.40963758452319610 ) ) ;
#9612 = ORIENTED_EDGE ( 'NONE', *, *, #37190, .T. ) ;
#9613 = EDGE_CURVE ( 'NONE', #20341, #10231, #33393, .T. ) ;
#9614 = CARTESIAN_POINT ( 'NONE',  ( -18.35341188057322981, -21.74886570111500461, 72.47438094868762448 ) ) ;
#9615 = CARTESIAN_POINT ( 'NONE',  ( -15.01784385650551457, -9.790100578890868377, 49.79778022625163203 ) ) ;
#9616 = VERTEX_POINT ( 'NONE', #26068 ) ;
#9617 = CARTESIAN_POINT ( 'NONE',  ( -13.58645566915974889, -20.72335281391582384, 61.81086499241362731 ) ) ;
#9618 = CARTESIAN_POINT ( 'NONE',  ( -22.07805708657739885, -20.69058616546009333, 53.49999999999994316 ) ) ;
#9619 = CARTESIAN_POINT ( 'NONE',  ( -16.45566506110110083, -21.79267588865899086, 62.04095995016087528 ) ) ;
#9620 = VERTEX_POINT ( 'NONE', #15198 ) ;
#9621 = DIRECTION ( 'NONE',  ( -1.000000000000000000, 4.164305804376849172E-17, -1.614929280266638808E-16 ) ) ;
#9622 =( BOUNDED_CURVE ( )  B_SPLINE_CURVE ( 3, ( #10784, #34827, #14942, #27205 ),
 .UNSPECIFIED., .F., .F. ) 
 B_SPLINE_CURVE_WITH_KNOTS ( ( 4, 4 ),
 ( 0.4074455897393676196, 0.5000000000000000000 ),
 .UNSPECIFIED. ) 
 CURVE ( )  GEOMETRIC_REPRESENTATION_ITEM ( )  RATIONAL_B_SPLINE_CURVE ( ( 0.6983129098260915102, 0.7760317562606854347, 0.8765941196519848599, 0.9999999999999816813 ) ) 
 REPRESENTATION_ITEM ( '' )  );
#9623 = DIRECTION ( 'NONE',  ( -0.8858372764600319638, -0.4639960340712762088, -2.848505657311710446E-17 ) ) ;
#9624 = DIRECTION ( 'NONE',  ( -0.9687793358424821033, 0.2479245821708679631, -1.885439946533205044E-16 ) ) ;
#9625 = DIRECTION ( 'NONE',  ( -3.071710424422018668E-17, 6.404604876783312462E-16, 1.000000000000000000 ) ) ;
#9626 = EDGE_LOOP ( 'NONE', ( #40589, #15009 ) ) ;
#9627 = ORIENTED_EDGE ( 'NONE', *, *, #11815, .T. ) ;
#9628 = EDGE_CURVE ( 'NONE', #40811, #20751, #36204, .T. ) ;
#9629 = CARTESIAN_POINT ( 'NONE',  ( -45.92409385541305511, -17.80920654474410370, 70.50000000000000000 ) ) ;
#9630 = CARTESIAN_POINT ( 'NONE',  ( -21.42200791050363051, -21.09572771556245740, 69.09804232902482113 ) ) ;
#9631 = ORIENTED_EDGE ( 'NONE', *, *, #25497, .T. ) ;
#9632 = CARTESIAN_POINT ( 'NONE',  ( -22.48547534937062409, -20.27602315292274326, 65.96067642556252508 ) ) ;
#9633 = CARTESIAN_POINT ( 'NONE',  ( -19.33968086220931326, -21.54245668240326950, 62.01120308345613807 ) ) ;
#9634 = CARTESIAN_POINT ( 'NONE',  ( -20.47409385759799250, -6.859212275519751323, 50.50378509014259265 ) ) ;
#9635 = ADVANCED_FACE ( 'NONE', ( #22360 ), #33926, .T. ) ;
#9636 = CARTESIAN_POINT ( 'NONE',  ( -23.79069799282712339, -10.94014436760912545, 73.55467436599077757 ) ) ;
#9637 = DIRECTION ( 'NONE',  ( -1.000000000000000000, -1.669677910507523057E-21, -6.493791346278465266E-22 ) ) ;
#9638 = CARTESIAN_POINT ( 'NONE',  ( -12.36731060793778525, -9.968227952340054543, 60.84301481710932080 ) ) ;
#9639 = ORIENTED_EDGE ( 'NONE', *, *, #45957, .F. ) ;
#9640 = ADVANCED_FACE ( 'NONE', ( #44537 ), #47420, .T. ) ;
#9641 = CARTESIAN_POINT ( 'NONE',  ( -16.57395829291861844, -22.21062093300318807, 65.26918445414273151 ) ) ;
#9642 = CARTESIAN_POINT ( 'NONE',  ( -19.10460565471617755, -7.550450307296652674, 63.54433857513910056 ) ) ;
#9643 = CARTESIAN_POINT ( 'NONE',  ( -24.47498361611929596, -14.63661054434306763, 59.12811639263489383 ) ) ;
#9644 = FACE_OUTER_BOUND ( 'NONE', #39418, .T. ) ;
#9645 = EDGE_CURVE ( 'NONE', #33881, #13202, #15434, .T. ) ;
#9646 = ORIENTED_EDGE ( 'NONE', *, *, #31562, .T. ) ;
#9647 = ORIENTED_EDGE ( 'NONE', *, *, #2436, .T. ) ;
#9648 = ORIENTED_EDGE ( 'NONE', *, *, #37063, .F. ) ;
#9649 = PRODUCT_DEFINITION ( 'UNKNOWN', '', #17973, #19903 ) ;
#9650 = CARTESIAN_POINT ( 'NONE',  ( -10.85011829770116876, -12.40413118360892142, 57.62857331434495478 ) ) ;
#9651 = CARTESIAN_POINT ( 'NONE',  ( -23.68302403447913562, -11.67432076229741078, 62.95218272177768881 ) ) ;
#9652 = CARTESIAN_POINT ( 'NONE',  ( -10.99655737938916289, -18.57624151290433900, 57.99209991576458378 ) ) ;
#9653 = EDGE_LOOP ( 'NONE', ( #7892, #42599 ) ) ;
#9654 = DIRECTION ( 'NONE',  ( -3.071710424422018668E-17, 6.404604876783312462E-16, 1.000000000000000000 ) ) ;
#9655 = CARTESIAN_POINT ( 'NONE',  ( -10.00132051839154457, -15.44646819276786154, 57.82438731113803243 ) ) ;
#9656 = ORIENTED_EDGE ( 'NONE', *, *, #5933, .T. ) ;
#9657 = CARTESIAN_POINT ( 'NONE',  ( -17.42409385541299471, -14.80920654474435771, 49.52966884056655772 ) ) ;
#9658 = CARTESIAN_POINT ( 'NONE',  ( -24.87453101240845399, -14.74101577129048835, 62.89951734912977344 ) ) ;
#9659 = ORIENTED_EDGE ( 'NONE', *, *, #6395, .F. ) ;
#9660 = CARTESIAN_POINT ( 'NONE',  ( -21.96649320589808241, -8.903988768509519147, 66.82296524986966801 ) ) ;
#9661 = EDGE_CURVE ( 'NONE', #12470, #11910, #45522, .T. ) ;
#9662 = EDGE_LOOP ( 'NONE', ( #27975, #44447, #233 ) ) ;
#9663 = CARTESIAN_POINT ( 'NONE',  ( -10.58358060774661702, -13.32320000501192325, 71.28116551139133605 ) ) ;
#9664 = ORIENTED_EDGE ( 'NONE', *, *, #15530, .T. ) ;
#9665 = CARTESIAN_POINT ( 'NONE',  ( -11.90372551521334721, -19.81226007308474379, 58.06648994900333349 ) ) ;
#9666 = CARTESIAN_POINT ( 'NONE',  ( -13.38462805196022742, -20.58720062598995426, 58.34650077712429095 ) ) ;
#9667 = CARTESIAN_POINT ( 'NONE',  ( -19.45974256962118787, -21.56279627256283149, 58.52507131872702928 ) ) ;
#9668 = EDGE_LOOP ( 'NONE', ( #38320, #38627, #2626, #6480 ) ) ;
#9669 = FACE_OUTER_BOUND ( 'NONE', #15978, .T. ) ;
#9670 = CARTESIAN_POINT ( 'NONE',  ( -17.42409385541299471, -14.80920654474435771, 49.52966884056655772 ) ) ;
#9671 = DIRECTION ( 'NONE',  ( 0.3037135924646502394, -0.9527633776296273727, -2.170275161112332872E-08 ) ) ;
#9672 = CARTESIAN_POINT ( 'NONE',  ( -11.18828695359561998, -11.51993516781315918, 67.62424403053286426 ) ) ;
#9673 = CARTESIAN_POINT ( 'NONE',  ( -24.72409385541305582, -14.80920654474418896, 65.94705882352940307 ) ) ;
#9674 = CARTESIAN_POINT ( 'NONE',  ( -10.00368807899092971, -15.89896712085359098, 54.27966884056655061 ) ) ;
#9675 = ORIENTED_EDGE ( 'NONE', *, *, #12666, .F. ) ;
#9676 = DIRECTION ( 'NONE',  ( -3.071710424422018668E-17, 6.404604876783312462E-16, 1.000000000000000000 ) ) ;
#9677 = FACE_BOUND ( 'NONE', #16955, .T. ) ;
#9678 = CARTESIAN_POINT ( 'NONE',  ( -24.69822963474414479, -13.19963333263893190, 59.54763306486673713 ) ) ;
#9679 = CARTESIAN_POINT ( 'NONE',  ( -13.19099303553301716, -20.93988663701172470, 58.22366935847014702 ) ) ;
#9680 = LINE ( 'NONE', #5967, #46489 ) ;
#9681 = CARTESIAN_POINT ( 'NONE',  ( -13.29909385650551812, -8.114302828567740988, 52.18300498402516041 ) ) ;
#9682 = ORIENTED_EDGE ( 'NONE', *, *, #6824, .F. ) ;
#9683 = EDGE_CURVE ( 'NONE', #1168, #8065, #31478, .T. ) ;
#9684 = CARTESIAN_POINT ( 'NONE',  ( -22.66113285952138767, -10.16448668345338646, 66.65068261271596839 ) ) ;
#9685 = CARTESIAN_POINT ( 'NONE',  ( -24.82475139314513868, -15.66597149415626156, 73.11808456017074320 ) ) ;
#9686 = ORIENTED_EDGE ( 'NONE', *, *, #24511, .T. ) ;
#9687 = CARTESIAN_POINT ( 'NONE',  ( -11.29476715451500723, -19.04418240398407391, 68.47335581180095687 ) ) ;
#9688 = CYLINDRICAL_SURFACE ( 'NONE', #30641, 1.999999999999999112 ) ;
#9689 = FACE_OUTER_BOUND ( 'NONE', #23041, .T. ) ;
#9690 = CARTESIAN_POINT ( 'NONE',  ( -18.53034385541318230, -6.857644439848909812, 49.98602051094048448 ) ) ;
#9691 = EDGE_CURVE ( 'NONE', #44542, #2764, #19889, .T. ) ;
#9692 = CARTESIAN_POINT ( 'NONE',  ( -24.72409385541305582, -14.90920654474414775, 61.02352941176469869 ) ) ;
#9693 = ORIENTED_EDGE ( 'NONE', *, *, #29115, .T. ) ;
#9694 = CARTESIAN_POINT ( 'NONE',  ( -24.41273239759876290, -14.40839838354480484, 66.18292728377200262 ) ) ;
#9695 = CARTESIAN_POINT ( 'NONE',  ( -46.29409385541305966, -16.70920654474410938, 70.50000000000000000 ) ) ;
#9696 = EDGE_CURVE ( 'NONE', #24254, #19672, #45846, .T. ) ;
#9697 = CARTESIAN_POINT ( 'NONE',  ( -14.85822224217540466, -7.814955975418383716, 57.04338293508369162 ) ) ;
#9698 = ORIENTED_EDGE ( 'NONE', *, *, #12126, .F. ) ;
#9699 = CARTESIAN_POINT ( 'NONE',  ( -22.07805708657739885, -20.69058616546009333, 54.27966884056654351 ) ) ;
#9700 = CARTESIAN_POINT ( 'NONE',  ( -16.78341213209640159, -22.23169296657789928, 68.88056055876903372 ) ) ;
#9701 =( BOUNDED_CURVE ( )  B_SPLINE_CURVE ( 3, ( #37678, #282, #7919, #7181 ),
 .UNSPECIFIED., .F., .F. ) 
 B_SPLINE_CURVE_WITH_KNOTS ( ( 4, 4 ),
 ( 0.5000000000000000000, 0.9074455897393652881 ),
 .UNSPECIFIED. ) 
 CURVE ( )  GEOMETRIC_REPRESENTATION_ITEM ( )  RATIONAL_B_SPLINE_CURVE ( ( 1.000000000000003775, 0.4567392136813372971, 0.3561768502900295452, 0.6983129098260845158 ) ) 
 REPRESENTATION_ITEM ( '' )  );
#9702 = ADVANCED_FACE ( 'NONE', ( #8567 ), #30171, .T. ) ;
#9703 = CARTESIAN_POINT ( 'NONE',  ( -13.30711168077662521, -9.147894172712071281, 64.20946529582356277 ) ) ;
#9704 = CARTESIAN_POINT ( 'NONE',  ( -24.17671788954033474, -17.95647625464824060, 59.11040117746514255 ) ) ;
#9705 = CARTESIAN_POINT ( 'NONE',  ( -50.42609385541305755, -14.80920654474423159, 69.97058823529410176 ) ) ;
#9706 = CARTESIAN_POINT ( 'NONE',  ( -22.04114742393716142, -9.481025248639417313, 59.73643293354757589 ) ) ;
#9707 = ORIENTED_EDGE ( 'NONE', *, *, #35231, .T. ) ;
#9708 = VERTEX_POINT ( 'NONE', #16165 ) ;
#9709 = CARTESIAN_POINT ( 'NONE',  ( -16.89909385541304232, -8.105421454601382081, 49.25000573077640098 ) ) ;
#9710 = CARTESIAN_POINT ( 'NONE',  ( -14.97188219925329378, -8.199429090594037461, 57.14999999999993463 ) ) ;
#9711 = CIRCLE ( 'NONE', #30126, 4.686499999999997890 ) ;
#9712 = EDGE_CURVE ( 'NONE', #26867, #9986, #6383, .T. ) ;
#9713 = ADVANCED_FACE ( 'NONE', ( #45992 ), #12492, .F. ) ;
#9714 = DIRECTION ( 'NONE',  ( 0.3667195576449454042, -0.9303315355510073381, -1.591455084066186922E-08 ) ) ;
#9715 = CARTESIAN_POINT ( 'NONE',  ( -14.03886453949006707, -20.93621418299524350, 68.64728233417358183 ) ) ;
#9716 = ORIENTED_EDGE ( 'NONE', *, *, #45811, .F. ) ;
#9717 = CARTESIAN_POINT ( 'NONE',  ( -19.29319497538623551, -22.02110451082404907, 58.66474050209521351 ) ) ;
#9718 = CARTESIAN_POINT ( 'NONE',  ( -24.14854887165027009, -16.95319183457820955, 69.56907079017828721 ) ) ;
#9719 = ORIENTED_EDGE ( 'NONE', *, *, #20772, .F. ) ;
#9720 = CARTESIAN_POINT ( 'NONE',  ( -17.99345148343727985, -22.23754510569404630, 62.05252827920184444 ) ) ;
#9721 = CARTESIAN_POINT ( 'NONE',  ( -12.87691022455662448, -9.487114556874418625, 74.61923044615130607 ) ) ;
#9722 = ORIENTED_EDGE ( 'NONE', *, *, #13982, .F. ) ;
#9723 = FACE_OUTER_BOUND ( 'NONE', #35253, .T. ) ;
#9724 = CARTESIAN_POINT ( 'NONE',  ( -14.93917828805464687, -21.41072449876059380, 58.16617918585938440 ) ) ;
#9725 = EDGE_LOOP ( 'NONE', ( #11244, #45278, #14368, #35975 ) ) ;
#9726 = CARTESIAN_POINT ( 'NONE',  ( -17.07160637253920044, -10.12398423200249731, 49.52966884056655772 ) ) ;
#9727 = CARTESIAN_POINT ( 'NONE',  ( -24.05420634179087358, -17.20676946999824608, 69.69867738674849988 ) ) ;
#9728 = CARTESIAN_POINT ( 'NONE',  ( -16.78411497196904278, -21.83009869597352903, 68.69560651670111895 ) ) ;
#9729 = CARTESIAN_POINT ( 'NONE',  ( -10.70566809389435647, -16.94585225683366048, 57.68760548748759476 ) ) ;
#9730 = ORIENTED_EDGE ( 'NONE', *, *, #675, .T. ) ;
#9731 = CARTESIAN_POINT ( 'NONE',  ( -14.44809135640554487, -8.473323881223761234, 67.55975083863336295 ) ) ;
#9732 = CARTESIAN_POINT ( 'NONE',  ( -22.14090652532222236, -20.04928072148792495, 62.51967078134249078 ) ) ;
#9733 = CARTESIAN_POINT ( 'NONE',  ( -15.44650868948020594, -21.52416737904487576, 72.04575487468440542 ) ) ;
#9734 = DIRECTION ( 'NONE',  ( 0.9087012777736581670, -0.4174469879787382487, -4.853707507795077342E-09 ) ) ;
#9735 = CARTESIAN_POINT ( 'NONE',  ( -19.94917705995926482, -8.226604131702123013, 74.00624557436877637 ) ) ;
#9736 = CARTESIAN_POINT ( 'NONE',  ( -11.42128120280088943, -11.20812582466128760, 60.97885827003174342 ) ) ;
#9737 = VECTOR ( 'NONE', #48040, 1000.000000000000000 ) ;
#9738 = CYLINDRICAL_SURFACE ( 'NONE', #36901, 0.1500000000000035194 ) ;
#9739 = CARTESIAN_POINT ( 'NONE',  ( -23.27284462870851911, -18.74605969774991010, 66.10917289053097079 ) ) ;
#9740 = ORIENTED_EDGE ( 'NONE', *, *, #43640, .F. ) ;
#9741 = CARTESIAN_POINT ( 'NONE',  ( -50.42409385541305511, -14.80920654474410725, 74.99999999999998579 ) ) ;
#9742 = CARTESIAN_POINT ( 'NONE',  ( -14.29604390987698714, -8.047573190463928938, 67.38258169132794251 ) ) ;
#9743 = CARTESIAN_POINT ( 'NONE',  ( -20.79160213123634193, -10.44367524184475826, 53.88362224778187226 ) ) ;
#9744 =( BOUNDED_CURVE ( )  B_SPLINE_CURVE ( 3, ( #10712, #40746, #3323, #36317 ),
 .UNSPECIFIED., .F., .F. ) 
 B_SPLINE_CURVE_WITH_KNOTS ( ( 4, 4 ),
 ( 3.703566858574705169E-15, 0.2013579207903336277 ),
 .UNSPECIFIED. ) 
 CURVE ( )  GEOMETRIC_REPRESENTATION_ITEM ( )  RATIONAL_B_SPLINE_CURVE ( ( 1.000000000000000000, 0.9966241020034161124, 0.9966241020034161124, 1.000000000000000000 ) ) 
 REPRESENTATION_ITEM ( '' )  );
#9745 = ORIENTED_EDGE ( 'NONE', *, *, #27071, .F. ) ;
#9746 = LINE ( 'NONE', #13159, #23933 ) ;
#9747 = EDGE_CURVE ( 'NONE', #23337, #10698, #35764, .T. ) ;
#9748 = ORIENTED_EDGE ( 'NONE', *, *, #38935, .T. ) ;
#9749 = ORIENTED_EDGE ( 'NONE', *, *, #11263, .T. ) ;
#9750 = EDGE_LOOP ( 'NONE', ( #19968, #4997 ) ) ;
#9751 = EDGE_CURVE ( 'NONE', #1645, #17537, #12249, .T. ) ;
#9752 = CARTESIAN_POINT ( 'NONE',  ( -21.93588290314558265, -13.54151500546508657, 49.52966884056655772 ) ) ;
#9753 = CARTESIAN_POINT ( 'NONE',  ( -12.91473374035863841, -8.878720881321301661, 67.54089325269804078 ) ) ;
#9754 = CARTESIAN_POINT ( 'NONE',  ( -20.66696806162329025, -21.06910005082376358, 58.79475164909958096 ) ) ;
#9755 = DIRECTION ( 'NONE',  ( -3.549360974551883545E-17, 6.371834667872732552E-18, 1.000000000000000000 ) ) ;
#9756 = CARTESIAN_POINT ( 'NONE',  ( -10.71275542623144972, -16.80315959844558549, 57.75930835357964099 ) ) ;
#9757 =( BOUNDED_CURVE ( )  B_SPLINE_CURVE ( 3, ( #38239, #26449, #7757, #45901 ),
 .UNSPECIFIED., .F., .F. ) 
 B_SPLINE_CURVE_WITH_KNOTS ( ( 4, 4 ),
 ( 0.000000000000000000, 0.4074455897393695625 ),
 .UNSPECIFIED. ) 
 CURVE ( )  GEOMETRIC_REPRESENTATION_ITEM ( )  RATIONAL_B_SPLINE_CURVE ( ( 1.000000000000000000, 0.4567392136813288595, 0.3561768502900291566, 0.6983129098261007250 ) ) 
 REPRESENTATION_ITEM ( '' )  );
#9758 = EDGE_LOOP ( 'NONE', ( #23837, #22042 ) ) ;
#9759 = EDGE_LOOP ( 'NONE', ( #26592, #19100 ) ) ;
#9760 = CARTESIAN_POINT ( 'NONE',  ( -19.96784385650551741, -6.428312510596451368, 51.20221977374900035 ) ) ;
#9761 = CARTESIAN_POINT ( 'NONE',  ( -24.87384330133638599, -14.87999890626018384, 59.35804801245023299 ) ) ;
#9762 = CARTESIAN_POINT ( 'NONE',  ( -20.72573962529263625, -8.580110715261016097, 59.99125250080121674 ) ) ;
#9764 = EDGE_CURVE ( 'NONE', #27258, #48679, #2106, .T. ) ;
#9763 = CARTESIAN_POINT ( 'NONE',  ( -19.46159385650551599, -9.295667164867525756, 49.30633214617472504 ) ) ;
#9765 = EDGE_CURVE ( 'NONE', #26524, #33229, #46231, .T. ) ;
#9766 = AXIS2_PLACEMENT_3D ( 'NONE', #36758, #17340, #37013 ) ;
#9767 = EDGE_LOOP ( 'NONE', ( #18322, #36387 ) ) ;
#9768 = EDGE_CURVE ( 'NONE', #2153, #24134, #29314, .T. ) ;
#9769 = EDGE_CURVE ( 'NONE', #21456, #27235, #28095, .T. ) ;
#9770 = EDGE_CURVE ( 'NONE', #43599, #3423, #3686, .T. ) ;
#9771 = CARTESIAN_POINT ( 'NONE',  ( -24.36278207060129830, -15.73458306695098941, 69.53307441226529306 ) ) ;
#9772 = AXIS2_PLACEMENT_3D ( 'NONE', #21477, #44371, #6687 ) ;
#9773 = CARTESIAN_POINT ( 'NONE',  ( -10.64854695470030599, -12.86019059820356780, 64.55364013863997741 ) ) ;
#9774 = ORIENTED_EDGE ( 'NONE', *, *, #5468, .T. ) ;
#9775 = DIRECTION ( 'NONE',  ( -0.1464579420318390668, 0.9892168979631277281, 7.284849527811297202E-08 ) ) ;
#9776 = CARTESIAN_POINT ( 'NONE',  ( -22.44487633517903902, -9.931440556337857828, 73.76695770713021716 ) ) ;
#9777 = CARTESIAN_POINT ( 'NONE',  ( -21.38467548909741467, -8.976808945791946215, 73.60128784396469825 ) ) ;
#9778 = CARTESIAN_POINT ( 'NONE',  ( -22.48547534937062409, -20.27602315292274326, 65.96067642556252508 ) ) ;
#9779 = EDGE_LOOP ( 'NONE', ( #11544, #3134, #18778, #36394 ) ) ;
#9780 = CARTESIAN_POINT ( 'NONE',  ( -22.58065782673598676, -12.89613362149922260, 54.49999999999995026 ) ) ;
#9781 = DIRECTION ( 'NONE',  ( 0.000000000000000000, 1.000000000000000000, -0.000000000000000000 ) ) ;
#9782 = CARTESIAN_POINT ( 'NONE',  ( -17.98078303480458473, -21.78831889235732078, 65.57362029541940274 ) ) ;
#9783 = ORIENTED_EDGE ( 'NONE', *, *, #2394, .T. ) ;
#9784 = DIRECTION ( 'NONE',  ( 1.000000000000000000, 0.000000000000000000, 0.000000000000000000 ) ) ;
#9785 = ORIENTED_EDGE ( 'NONE', *, *, #26585, .T. ) ;
#9786 = FACE_OUTER_BOUND ( 'NONE', #18427, .T. ) ;
#9787 = CARTESIAN_POINT ( 'NONE',  ( -14.59168816866676188, -7.918454268363332993, 60.45849798934733599 ) ) ;
#9788 = ORIENTED_EDGE ( 'NONE', *, *, #15735, .F. ) ;
#9789 = CARTESIAN_POINT ( 'NONE',  ( -13.17733471316897642, -8.687979735119538915, 60.61667131793516461 ) ) ;
#9791 = ADVANCED_FACE ( 'NONE', ( #10532 ), #15310, .T. ) ;
#9790 = DIRECTION ( 'NONE',  ( 2.342027643795563533E-48, 1.912410701131276611E-32, 1.000000000000000000 ) ) ;
#9792 = CARTESIAN_POINT ( 'NONE',  ( -17.33887285826562774, -7.751749031259347333, 74.10451155337131013 ) ) ;
#9793 = CARTESIAN_POINT ( 'NONE',  ( -14.27198868620293482, -8.503074456523135538, 70.72957634543823247 ) ) ;
#9794 = ORIENTED_EDGE ( 'NONE', *, *, #38030, .F. ) ;
#9795 = CARTESIAN_POINT ( 'NONE',  ( -16.36834455927873222, -22.18410795223847387, 61.94063518049016182 ) ) ;
#9796 = DIRECTION ( 'NONE',  ( -2.866981220435666553E-17, 1.000000000000000000, 1.190614954331866791E-16 ) ) ;
#9797 = CARTESIAN_POINT ( 'NONE',  ( -16.56382623105763230, -21.80656378348893654, 65.22564414072157035 ) ) ;
#9798 = ORIENTED_EDGE ( 'NONE', *, *, #217, .T. ) ;
#9799 = CARTESIAN_POINT ( 'NONE',  ( -17.42409385541305511, -14.80920654474410725, 48.99999999999997868 ) ) ;
#9800 = VECTOR ( 'NONE', #39528, 1000.000000000000114 ) ;
#9801 = CARTESIAN_POINT ( 'NONE',  ( -24.35037712455101655, -13.45216126592925754, 62.97697330661279835 ) ) ;
#9802 = CIRCLE ( 'NONE', #5860, 4.686499999999997002 ) ;
#9803 = VERTEX_POINT ( 'NONE', #26039 ) ;
#9804 = ORIENTED_EDGE ( 'NONE', *, *, #37351, .T. ) ;
#9805 = PLANE ( 'NONE',  #18064 ) ;
#9806 = DIRECTION ( 'NONE',  ( 1.000000000000000000, 2.866981220435666553E-17, 0.000000000000000000 ) ) ;
#9807 = CARTESIAN_POINT ( 'NONE',  ( -10.02109181922889292, -15.64579944599920402, 61.21601811723743225 ) ) ;
#9808 = CARTESIAN_POINT ( 'NONE',  ( -16.89909385650551599, -8.114302828567740988, 52.18300498402516041 ) ) ;
#9809 = CARTESIAN_POINT ( 'NONE',  ( -21.88682393090045508, -8.843550627677114306, 66.82183330550128630 ) ) ;
#9810 = CARTESIAN_POINT ( 'NONE',  ( -10.40492013132468863, -15.46819742413635268, 57.86792798853620923 ) ) ;
#9811 = FACE_OUTER_BOUND ( 'NONE', #26683, .T. ) ;
#9812 = LINE ( 'NONE', #9579, #20022 ) ;
#9813 = CARTESIAN_POINT ( 'NONE',  ( -16.69812366561379591, -22.22391868458808517, 68.85707174038356015 ) ) ;
#9814 = VERTEX_POINT ( 'NONE', #40324 ) ;
#9815 = EDGE_LOOP ( 'NONE', ( #10745, #27773 ) ) ;
#9816 = CARTESIAN_POINT ( 'NONE',  ( -28.42409385541305511, -6.859206544744110623, 52.99999999999997158 ) ) ;
#9817 = CARTESIAN_POINT ( 'NONE',  ( -22.02419907101585395, -20.08547720931746383, 58.87328889079346794 ) ) ;
#9818 = CARTESIAN_POINT ( 'NONE',  ( -19.55442184481404766, -21.52995072282663358, 65.47958309245051112 ) ) ;
#9819 = CARTESIAN_POINT ( 'NONE',  ( -24.55648639541664124, -12.65693619758180688, 69.87968855437600268 ) ) ;
#9820 = DIRECTION ( 'NONE',  ( -0.5497669574358331479, 0.8353180786453390239, 7.898837271846010071E-08 ) ) ;
#9821 = ORIENTED_EDGE ( 'NONE', *, *, #5491, .F. ) ;
#9822 = EDGE_CURVE ( 'NONE', #45300, #32600, #18138, .T. ) ;
#9823 = ADVANCED_FACE ( 'NONE', ( #17659 ), #13443, .T. ) ;
#9824 = CARTESIAN_POINT ( 'NONE',  ( -21.10164091802717223, -17.71419016815049119, 49.52966884056655772 ) ) ;
#9825 = DIRECTION ( 'NONE',  ( -2.117869065290744265E-07, -2.255668823645213100E-07, -0.9999999999999521494 ) ) ;
#9826 = CARTESIAN_POINT ( 'NONE',  ( -10.43098718212803000, -15.70539730037032911, 61.32316937334011442 ) ) ;
#9827 = EDGE_LOOP ( 'NONE', ( #28920, #23508, #32255, #28106, #27987 ) ) ;
#9828 = VECTOR ( 'NONE', #37956, 1000.000000000000000 ) ;
#9829 = EDGE_CURVE ( 'NONE', #6268, #44129, #19368, .T. ) ;
#9830 = EDGE_CURVE ( 'NONE', #10899, #24601, #18475, .T. ) ;
#9831 = CARTESIAN_POINT ( 'NONE',  ( -10.56627932147773308, -16.21290872759732693, 71.74750383609593030 ) ) ;
#9832 = FACE_OUTER_BOUND ( 'NONE', #36532, .T. ) ;
#9833 = CIRCLE ( 'NONE', #3525, 3.982850737850967437 ) ;
#9834 = DIRECTION ( 'NONE',  ( 1.000000000000000000, 2.866981220435666553E-17, 0.000000000000000000 ) ) ;
#9835 = CARTESIAN_POINT ( 'NONE',  ( -24.85359113602694237, -14.25571898851532460, 69.76779851910008290 ) ) ;
#9836 = CARTESIAN_POINT ( 'NONE',  ( -10.90759836534377492, -17.49952001658422063, 68.39721944423101263 ) ) ;
#9837 = ORIENTED_EDGE ( 'NONE', *, *, #32122, .F. ) ;
#9838 = CARTESIAN_POINT ( 'NONE',  ( -23.01170616074242758, -19.02577216718165332, 58.89913050316314269 ) ) ;
#9839 = ORIENTED_EDGE ( 'NONE', *, *, #26525, .F. ) ;
#9840 = CARTESIAN_POINT ( 'NONE',  ( -24.36611147337434957, -16.04009697885371111, 66.07797069094537790 ) ) ;
#9841 = CARTESIAN_POINT ( 'NONE',  ( -10.23976007159296486, -12.83681284056133265, 67.89978877642941768 ) ) ;
#9842 = ORIENTED_EDGE ( 'NONE', *, *, #21563, .F. ) ;
#9843 = CARTESIAN_POINT ( 'NONE',  ( -10.98022799891133516, -11.94040251240491202, 71.29680800581914468 ) ) ;
#9844 = ADVANCED_FACE ( 'NONE', ( #45744 ), #4357, .T. ) ;
#9845 = CARTESIAN_POINT ( 'NONE',  ( -14.28659385650551528, -9.302874398569244363, 51.68646062012417985 ) ) ;
#9846 = B_SPLINE_CURVE_WITH_KNOTS ( 'NONE', 1,
 ( #10843, #3958 ),
 .UNSPECIFIED., .F., .F.,
 ( 2, 2 ),
 ( 0.000000000000000000, 1.000000000000000000 ),
 .UNSPECIFIED. ) ;
#9847 = EDGE_LOOP ( 'NONE', ( #29149, #35788, #18129, #14326, #4391 ) ) ;
#9848 = DIRECTION ( 'NONE',  ( -3.413470714839332458E-33, 1.190614954331866791E-16, -1.000000000000000000 ) ) ;
#9849 = CARTESIAN_POINT ( 'NONE',  ( -20.76617135726475993, -8.601540970369937256, 59.84685049461698014 ) ) ;
#9850 = CARTESIAN_POINT ( 'NONE',  ( -23.83080496556880945, -17.75212211224490133, 59.28906343887996400 ) ) ;
#9851 = ORIENTED_EDGE ( 'NONE', *, *, #1771, .F. ) ;
#9852 = CARTESIAN_POINT ( 'NONE',  ( -19.96446419288020735, -21.81276346405129019, 69.12756636080516159 ) ) ;
#9853 = CARTESIAN_POINT ( 'NONE',  ( -23.54964580958837672, -11.31912319124952759, 70.19210731698237282 ) ) ;
#9854 = CARTESIAN_POINT ( 'NONE',  ( -24.14679772577363437, -12.68507108172156705, 70.05770892828130059 ) ) ;
#9855 = CARTESIAN_POINT ( 'NONE',  ( -21.68499490698325971, -9.192515188766618550, 66.81149992326716358 ) ) ;
#9856 = ORIENTED_EDGE ( 'NONE', *, *, #3273, .T. ) ;
#9857 = ORIENTED_EDGE ( 'NONE', *, *, #7587, .T. ) ;
#9858 = CARTESIAN_POINT ( 'NONE',  ( -23.78452478447325547, -18.68833123104472449, 72.86393997050505789 ) ) ;
#9859 = CARTESIAN_POINT ( 'NONE',  ( -21.12516169987187098, -20.80993955427394582, 69.06922321213187388 ) ) ;
#9860 = ORIENTED_EDGE ( 'NONE', *, *, #29798, .F. ) ;
#9861 = CARTESIAN_POINT ( 'NONE',  ( -17.74685204685923523, -7.816528611283073857, 60.38060757087333030 ) ) ;
#9862 = CARTESIAN_POINT ( 'NONE',  ( -18.84284385759798752, -7.587656875400192291, 49.25157356644813689 ) ) ;
#9863 = CARTESIAN_POINT ( 'NONE',  ( -10.42462062702805703, -14.89507852762941198, 74.79778901763455679 ) ) ;
#9864 = CARTESIAN_POINT ( 'NONE',  ( -10.90176001668674743, -17.49323270848192635, 71.98206789237249836 ) ) ;
#9865 = CARTESIAN_POINT ( 'NONE',  ( -36.42409385541304800, -9.359200813967566646, 50.49621490985803263 ) ) ;
#9866 = ORIENTED_EDGE ( 'NONE', *, *, #10446, .T. ) ;
#9867 = CARTESIAN_POINT ( 'NONE',  ( -21.02205230129062485, -8.737166911425223503, 59.98558246646761916 ) ) ;
#9868 = CIRCLE ( 'NONE', #20763, 2.000000000000001332 ) ;
#9869 = CARTESIAN_POINT ( 'NONE',  ( -16.47989802999360265, -19.41181990985090877, 52.02966884056656482 ) ) ;
#9870 = CARTESIAN_POINT ( 'NONE',  ( -11.82948135756627117, -23.21535936243710552, 54.54971261817297545 ) ) ;
#9871 = FACE_OUTER_BOUND ( 'NONE', #39643, .T. ) ;
#9872 =( BOUNDED_SURFACE ( )  B_SPLINE_SURFACE ( 3, 1, ( 
 ( #28977, #29226 ),
 ( #32201, #2395 ),
 ( #47217, #13461 ),
 ( #47939, #28506 ),
 ( #24810, #14170 ),
 ( #25298, #21833 ),
 ( #6085, #40537 ) ),
 .UNSPECIFIED., .T., .F., .F. ) 
 B_SPLINE_SURFACE_WITH_KNOTS ( ( 4, 3, 4 ),
 ( 2, 2 ),
 ( 0.000000000000000000, 0.5000000000000000000, 1.000000000000000000 ),
 ( 0.000000000000000000, 1.000000000000000000 ),
 .UNSPECIFIED. ) 
 GEOMETRIC_REPRESENTATION_ITEM ( )  RATIONAL_B_SPLINE_SURFACE ( (
 ( 1.000000000000000000, 1.000000000000000000),
 ( 0.3333333333333335369, 0.3333333333333330373),
 ( 0.3333333333333335369, 0.3333333333333330373),
 ( 1.000000000000000000, 1.000000000000000000),
 ( 0.3333333333333333703, 0.3333333333333333703),
 ( 0.3333333333333333703, 0.3333333333333333703),
 ( 1.000000000000000000, 1.000000000000000000) ) ) 
 REPRESENTATION_ITEM ( '' )  SURFACE ( )  );
#9873 = EDGE_LOOP ( 'NONE', ( #2133, #12822 ) ) ;
#9874 = VERTEX_POINT ( 'NONE', #23315 ) ;
#9875 = EDGE_CURVE ( 'NONE', #508, #40402, #10009, .T. ) ;
#9876 = DIRECTION ( 'NONE',  ( 1.209056813000714825E-06, 5.657077699801570473E-07, 0.9999999999991090460 ) ) ;
#9877 = DIRECTION ( 'NONE',  ( -0.000000000000000000, -0.000000000000000000, 1.000000000000000000 ) ) ;
#9878 = CARTESIAN_POINT ( 'NONE',  ( -23.89622975106627223, -11.11939700565759459, 69.99872433690991613 ) ) ;
#9879 =( BOUNDED_SURFACE ( )  B_SPLINE_SURFACE ( 3, 1, ( 
 ( #18808, #40724 ),
 ( #15337, #33818 ),
 ( #7504, #45180 ),
 ( #44684, #25958 ),
 ( #25470, #114 ),
 ( #11418, #26443 ),
 ( #41456, #7752 ) ),
 .UNSPECIFIED., .T., .F., .F. ) 
 B_SPLINE_SURFACE_WITH_KNOTS ( ( 4, 3, 4 ),
 ( 2, 2 ),
 ( 0.000000000000000000, 0.5000000000000000000, 1.000000000000000000 ),
 ( 0.000000000000000000, 1.000000000000000000 ),
 .UNSPECIFIED. ) 
 GEOMETRIC_REPRESENTATION_ITEM ( )  RATIONAL_B_SPLINE_SURFACE ( (
 ( 1.000000000000000000, 1.000000000000000000),
 ( 0.3333333333333335369, 0.3333333333333330373),
 ( 0.3333333333333335369, 0.3333333333333330373),
 ( 1.000000000000000000, 1.000000000000000000),
 ( 0.3333333333333333703, 0.3333333333333333703),
 ( 0.3333333333333333703, 0.3333333333333333703),
 ( 1.000000000000000000, 1.000000000000000000) ) ) 
 REPRESENTATION_ITEM ( '' )  SURFACE ( )  );
#9880 = VERTEX_POINT ( 'NONE', #18888 ) ;
#9881 =( BOUNDED_CURVE ( )  B_SPLINE_CURVE ( 3, ( #9710, #24239, #21514, #39730 ),
 .UNSPECIFIED., .F., .F. ) 
 B_SPLINE_CURVE_WITH_KNOTS ( ( 4, 4 ),
 ( 0.9074455897393685078, 1.000000000000000000 ),
 .UNSPECIFIED. ) 
 CURVE ( )  GEOMETRIC_REPRESENTATION_ITEM ( )  RATIONAL_B_SPLINE_CURVE ( ( 0.6983129098261030565, 0.7760317562607068620, 0.8765941196520058432, 1.000000000000000000 ) ) 
 REPRESENTATION_ITEM ( '' )  );
#9882 = CARTESIAN_POINT ( 'NONE',  ( -24.26595263201846109, -13.32969024507516309, 59.66267925069213618 ) ) ;
#9883 = EDGE_CURVE ( 'NONE', #30449, #7311, #38562, .T. ) ;
#9884 = CARTESIAN_POINT ( 'NONE',  ( -12.76547314785493192, -9.517330534081262172, 74.60450883341005124 ) ) ;
#9885 = VERTEX_POINT ( 'NONE', #29980 ) ;
#9886 = EDGE_CURVE ( 'NONE', #7245, #47302, #39261, .T. ) ;
#9887 = CARTESIAN_POINT ( 'NONE',  ( -11.03161394367693049, -18.63672047605813376, 57.92059234540772650 ) ) ;
#9888 = CARTESIAN_POINT ( 'NONE',  ( -20.40273017466792638, -8.415258652480821056, 70.55100319412855470 ) ) ;
#9889 = EDGE_CURVE ( 'NONE', #2374, #41728, #31072, .T. ) ;
#9890 = CARTESIAN_POINT ( 'NONE',  ( -23.37950063508610299, -10.33300044972819975, 59.70929291905022751 ) ) ;
#9891 = B_SPLINE_CURVE_WITH_KNOTS ( 'NONE', 3,
 ( #35241, #5473, #23712, #27862, #20489, #15797, #20230, #38201, #43129, #8684 ),
 .UNSPECIFIED., .F., .F.,
 ( 4, 2, 2, 2, 4 ),
 ( 0.1272669073658402039, 0.2522669073488030267, 0.3772669073317658217, 0.5022669073147286722, 0.6272669072976915228 ),
 .UNSPECIFIED. ) ;
#9892 = VERTEX_POINT ( 'NONE', #19131 ) ;
#9893 =( BOUNDED_CURVE ( )  B_SPLINE_CURVE ( 3, ( #1277, #31326, #42425, #28369 ),
 .UNSPECIFIED., .F., .F. ) 
 B_SPLINE_CURVE_WITH_KNOTS ( ( 4, 4 ),
 ( 0.9074455897393621795, 1.000000000000000000 ),
 .UNSPECIFIED. ) 
 CURVE ( )  GEOMETRIC_REPRESENTATION_ITEM ( )  RATIONAL_B_SPLINE_CURVE ( ( 0.6983129098260923984, 0.7760317562606976471, 0.8765941196520001810, 1.000000000000000000 ) ) 
 REPRESENTATION_ITEM ( '' )  );
#9894 = VECTOR ( 'NONE', #22399, 1000.000000000000000 ) ;
#9895 = EDGE_LOOP ( 'NONE', ( #35276, #38994 ) ) ;
#9896 = CARTESIAN_POINT ( 'NONE',  ( -15.95707318215220205, -7.504986700048139170, 63.85506303619484214 ) ) ;
#9897 = CARTESIAN_POINT ( 'NONE',  ( -24.47658614515328779, -17.21021725504682109, 73.03336031685063290 ) ) ;
#9898 = CARTESIAN_POINT ( 'NONE',  ( -18.11889358109259973, -21.82488563948435711, 65.64532159284070190 ) ) ;
#9899 = ORIENTED_EDGE ( 'NONE', *, *, #16207, .T. ) ;
#9900 = CARTESIAN_POINT ( 'NONE',  ( -46.92409385541305511, -17.80920654474410370, 60.24999999999999289 ) ) ;
#9901 = CARTESIAN_POINT ( 'NONE',  ( -10.29385316490627211, -12.64970523595484231, 64.38340807599202265 ) ) ;
#9902 = FACE_OUTER_BOUND ( 'NONE', #33414, .T. ) ;
#9903 = LINE ( 'NONE', #2263, #5448 ) ;
#9904 = CARTESIAN_POINT ( 'NONE',  ( -24.72409385541305582, -14.80920654474414810, 61.92352941176469727 ) ) ;
#9905 = CARTESIAN_POINT ( 'NONE',  ( -20.51077960756537522, -21.09370107797763083, 58.75548229756886798 ) ) ;
#9906 = ORIENTED_EDGE ( 'NONE', *, *, #27818, .T. ) ;
#9907 = CARTESIAN_POINT ( 'NONE',  ( -24.80275449484538441, -15.83773296361996863, 69.68307485620266561 ) ) ;
#9908 = FACE_OUTER_BOUND ( 'NONE', #40140, .T. ) ;
#9909 = DIRECTION ( 'NONE',  ( -3.597453700672850830E-07, -4.264980243973025121E-06, 0.9999999999908403270 ) ) ;
#9910 = CARTESIAN_POINT ( 'NONE',  ( -16.26195973558533936, -21.76306465430365122, 58.57113428431811997 ) ) ;
#9911 = CARTESIAN_POINT ( 'NONE',  ( -17.42409385541299471, -14.80920654474435594, 52.02966884056656482 ) ) ;
#9912 = ORIENTED_EDGE ( 'NONE', *, *, #37031, .T. ) ;
#9913 = EDGE_LOOP ( 'NONE', ( #3613, #3786 ) ) ;
#9914 = DIRECTION ( 'NONE',  ( -3.071710424422018668E-17, 6.404604876783312462E-16, 1.000000000000000000 ) ) ;
#9915 = DIRECTION ( 'NONE',  ( 0.2843796944294933460, 0.9587117342539337450, 5.205739956168971478E-08 ) ) ;
#9916 = VERTEX_POINT ( 'NONE', #34867 ) ;
#9917 = CARTESIAN_POINT ( 'NONE',  ( 6.575906144586949331, -6.109215713985405749, 50.50605614422795497 ) ) ;
#9918 = CARTESIAN_POINT ( 'NONE',  ( -10.10423179225323054, -16.19963241119870645, 71.63405780323361682 ) ) ;
#9919 = FACE_OUTER_BOUND ( 'NONE', #6489, .T. ) ;
#9920 = CARTESIAN_POINT ( 'NONE',  ( -22.98758735661991892, -9.854289139077749837, 70.26824437992965500 ) ) ;
#9921 = CARTESIAN_POINT ( 'NONE',  ( -17.00402163565062708, -22.24752138760033660, 72.30396712152169414 ) ) ;
#9922 = ORIENTED_EDGE ( 'NONE', *, *, #37266, .F. ) ;
#9923 = FACE_BOUND ( 'NONE', #20795, .T. ) ;
#9924 = LINE ( 'NONE', #24941, #10559 ) ;
#9925 = LINE ( 'NONE', #12644, #15454 ) ;
#9926 = FACE_OUTER_BOUND ( 'NONE', #23938, .T. ) ;
#9927 = ORIENTED_EDGE ( 'NONE', *, *, #3692, .T. ) ;
#9928 = FACE_OUTER_BOUND ( 'NONE', #11344, .T. ) ;
#9929 = LINE ( 'NONE', #40213, #16406 ) ;
#9930 = CARTESIAN_POINT ( 'NONE',  ( -16.98029472128749617, -7.773148622573092581, 74.26018263347066295 ) ) ;
#9931 = DIRECTION ( 'NONE',  ( 0.9757441136919974278, 0.2189141945955503377, 0.000000000000000000 ) ) ;
#9932 = EDGE_CURVE ( 'NONE', #4040, #34525, #45267, .T. ) ;
#9933 = CARTESIAN_POINT ( 'NONE',  ( -10.70297003644833644, -11.59513240183115279, 71.27356180636090244 ) ) ;
#9934 = FACE_OUTER_BOUND ( 'NONE', #44936, .T. ) ;
#9935 = ORIENTED_EDGE ( 'NONE', *, *, #37779, .T. ) ;
#9936 = AXIS2_PLACEMENT_3D ( 'NONE', #38398, #23657, #754 ) ;
#9937 = ORIENTED_EDGE ( 'NONE', *, *, #45297, .F. ) ;
#9938 = VECTOR ( 'NONE', #36268, 1000.000000000000000 ) ;
#9939 = CARTESIAN_POINT ( 'NONE',  ( -19.76784385541304090, -9.357632978295830739, 49.97845033065684106 ) ) ;
#9940 = DIRECTION ( 'NONE',  ( 8.419732586906766855E-06, -4.907637678936094986E-06, -0.9999999999525116534 ) ) ;
#9941 = CARTESIAN_POINT ( 'NONE',  ( -20.13067924262885100, -8.351893229360399573, 73.91023551582938467 ) ) ;
#9942 = CARTESIAN_POINT ( 'NONE',  ( -17.42409385541299471, -14.80920654474435594, 52.02966884056656482 ) ) ;
#9943 = CARTESIAN_POINT ( 'NONE',  ( -42.07024770156689897, -25.10920654474410441, 65.83076923076922071 ) ) ;
#9944 = VERTEX_POINT ( 'NONE', #195 ) ;
#9945 = EDGE_CURVE ( 'NONE', #26800, #44868, #11831, .T. ) ;
#9946 = CARTESIAN_POINT ( 'NONE',  ( -10.99230636966125729, -11.04936141590450127, 60.80072991414726147 ) ) ;
#9947 = CARTESIAN_POINT ( 'NONE',  ( -9.424093855413051557, -25.10920654474410441, 77.00000000000000000 ) ) ;
#9948 = EDGE_CURVE ( 'NONE', #11779, #744, #45492, .T. ) ;
#9949 = ORIENTED_EDGE ( 'NONE', *, *, #36195, .F. ) ;
#9950 = CARTESIAN_POINT ( 'NONE',  ( -24.41485939984550058, -14.44976655980182834, 66.48292729254383460 ) ) ;
#9951 = CYLINDRICAL_SURFACE ( 'NONE', #20431, 0.1499999999999985234 ) ;
#9952 = ORIENTED_EDGE ( 'NONE', *, *, #43579, .F. ) ;
#9953 = EDGE_CURVE ( 'NONE', #17470, #13199, #25400, .T. ) ;
#9954 = DIRECTION ( 'NONE',  ( 7.105595952316565779E-06, 6.912614981796274630E-07, -0.9999999999745162738 ) ) ;
#9955 = CARTESIAN_POINT ( 'NONE',  ( -12.23896285002386719, -13.98645721660588315, 49.52966884056655772 ) ) ;
#9956 = ORIENTED_EDGE ( 'NONE', *, *, #9764, .T. ) ;
#9957 = CARTESIAN_POINT ( 'NONE',  ( -10.51282180855659298, -13.41675832278428615, 74.97257849336672564 ) ) ;
#9958 = CARTESIAN_POINT ( 'NONE',  ( -23.40706704545067041, -18.44294168544361057, 72.76368236816873036 ) ) ;
#9959 = EDGE_CURVE ( 'NONE', #46068, #30656, #7150, .T. ) ;
#9960 = CARTESIAN_POINT ( 'NONE',  ( -16.74223095289501018, -21.77591761258009839, 65.33450335857290270 ) ) ;
#9961 = CARTESIAN_POINT ( 'NONE',  ( -10.57110082969170683, -13.38215148069720861, 74.67817647591368768 ) ) ;
#9962 = VERTEX_POINT ( 'NONE', #39296 ) ;
#9963 = CARTESIAN_POINT ( 'NONE',  ( -21.93816111929147539, -20.22843456855405364, 62.64927864921646261 ) ) ;
#9964 = CARTESIAN_POINT ( 'NONE',  ( -24.37683822056718697, -15.97618770311995462, 66.06324926631656069 ) ) ;
#9965 = CARTESIAN_POINT ( 'NONE',  ( -21.40553701582064150, -22.29995169140471845, 54.49999999999995026 ) ) ;
#9966 = FACE_OUTER_BOUND ( 'NONE', #41028, .T. ) ;
#9967 = CARTESIAN_POINT ( 'NONE',  ( -20.38066051823377478, -10.47086428435309102, 52.02966884056656482 ) ) ;
#9968 = FACE_OUTER_BOUND ( 'NONE', #13619, .T. ) ;
#9969 = CARTESIAN_POINT ( 'NONE',  ( -23.50612575731066656, -19.11299006986292071, 66.01044822673141255 ) ) ;
#9970 = VERTEX_POINT ( 'NONE', #5328 ) ;
#9971 = CARTESIAN_POINT ( 'NONE',  ( -24.34180841910587034, -17.57479211026192090, 66.05018951071652111 ) ) ;
#9972 =( BOUNDED_CURVE ( )  B_SPLINE_CURVE ( 3, ( #24859, #36400, #13980, #6627 ),
 .UNSPECIFIED., .F., .F. ) 
 B_SPLINE_CURVE_WITH_KNOTS ( ( 4, 4 ),
 ( 0.4074455897393663428, 0.5000000000000000000 ),
 .UNSPECIFIED. ) 
 CURVE ( )  GEOMETRIC_REPRESENTATION_ITEM ( )  RATIONAL_B_SPLINE_CURVE ( ( 0.6983129098261003920, 0.7760317562607003117, 0.8765941196519989598, 0.9999999999999932276 ) ) 
 REPRESENTATION_ITEM ( '' )  );
#9973 = VECTOR ( 'NONE', #9775, 1000.000000000000227 ) ;
#9974 = DIRECTION ( 'NONE',  ( 1.927470528863119542E-16, 0.000000000000000000, -1.000000000000000000 ) ) ;
#9975 = CARTESIAN_POINT ( 'NONE',  ( -20.84119746710918974, -20.97572115929791892, 62.11471400470772863 ) ) ;
#9976 = ORIENTED_EDGE ( 'NONE', *, *, #14187, .F. ) ;
#9977 = CARTESIAN_POINT ( 'NONE',  ( -24.34138173484706158, -16.17068648017255583, 62.59328676670276792 ) ) ;
#9978 = EDGE_LOOP ( 'NONE', ( #46193, #26231, #42590, #43524, #27930 ) ) ;
#9979 = ORIENTED_EDGE ( 'NONE', *, *, #34875, .F. ) ;
#9980 = EDGE_LOOP ( 'NONE', ( #10965, #3624 ) ) ;
#9981 = CARTESIAN_POINT ( 'NONE',  ( -45.92409385541306222, -14.20920654474410760, 70.50000000000000000 ) ) ;
#9982 = DIRECTION ( 'NONE',  ( -3.071710424422018668E-17, 6.404604876783312462E-16, 1.000000000000000000 ) ) ;
#9983 = ADVANCED_FACE ( 'NONE', ( #6042 ), #9516, .T. ) ;
#9984 = FACE_OUTER_BOUND ( 'NONE', #16247, .T. ) ;
#9985 = CARTESIAN_POINT ( 'NONE',  ( -12.74071780128996423, -9.015264284427722430, 70.96430057504635158 ) ) ;
#9986 = VERTEX_POINT ( 'NONE', #5089 ) ;
#9987 = ORIENTED_EDGE ( 'NONE', *, *, #47660, .F. ) ;
#9988 = CARTESIAN_POINT ( 'NONE',  ( -19.18034385650551599, -6.424090610841176385, 49.80797279389977916 ) ) ;
#9989 = CARTESIAN_POINT ( 'NONE',  ( -14.09463846823036981, -8.088735815341543400, 54.27966884056655061 ) ) ;
#9990 = DIRECTION ( 'NONE',  ( 3.413470714839332458E-33, -1.190614954331866791E-16, 1.000000000000000000 ) ) ;
#9991 = CARTESIAN_POINT ( 'NONE',  ( -19.79909385650551457, -8.114302828567740988, 52.18300498402516041 ) ) ;
#9992 = EDGE_CURVE ( 'NONE', #656, #29137, #31591, .T. ) ;
#9993 = AXIS2_PLACEMENT_3D ( 'NONE', #16022, #15047, #3742 ) ;
#9994 = AXIS2_PLACEMENT_3D ( 'NONE', #1560, #38985, #27667 ) ;
#9995 = ORIENTED_EDGE ( 'NONE', *, *, #17579, .T. ) ;
#9996 = CARTESIAN_POINT ( 'NONE',  ( -13.50190746284422794, -17.39609839546894321, 52.02966884056656482 ) ) ;
#9997 = DIRECTION ( 'NONE',  ( 0.000000000000000000, 1.000000000000000000, 0.000000000000000000 ) ) ;
#9998 = CIRCLE ( 'NONE', #44588, 1.999999999999999112 ) ;
#9999 = EDGE_LOOP ( 'NONE', ( #29029, #11595 ) ) ;
#10000 = DIRECTION ( 'NONE',  ( -3.071710424422018668E-17, 6.404604876783312462E-16, 1.000000000000000000 ) ) ;
#10001 = VERTEX_POINT ( 'NONE', #12463 ) ;
#10002 = EDGE_CURVE ( 'NONE', #30760, #37795, #39351, .T. ) ;
#10003 = CARTESIAN_POINT ( 'NONE',  ( -10.65419218092657339, -12.82848081120560479, 60.79853508363822101 ) ) ;
#10004 = DIRECTION ( 'NONE',  ( 0.000000000000000000, 1.000000000000000000, -0.000000000000000000 ) ) ;
#10005 = EDGE_CURVE ( 'NONE', #48717, #31810, #29853, .T. ) ;
#10006 = EDGE_LOOP ( 'NONE', ( #37719, #36610 ) ) ;
#10007 = CARTESIAN_POINT ( 'NONE',  ( -12.77988270905505175, -9.504878500073925096, 74.61363196716065715 ) ) ;
#10008 = EDGE_CURVE ( 'NONE', #7399, #26571, #13168, .T. ) ;
#10009 =( BOUNDED_CURVE ( )  B_SPLINE_CURVE ( 3, ( #23084, #11750, #8074, #4850 ),
 .UNSPECIFIED., .F., .F. ) 
 B_SPLINE_CURVE_WITH_KNOTS ( ( 4, 4 ),
 ( 0.4074455897393599590, 0.5000000000000000000 ),
 .UNSPECIFIED. ) 
 CURVE ( )  GEOMETRIC_REPRESENTATION_ITEM ( )  RATIONAL_B_SPLINE_CURVE ( ( 0.6983129098260680845, 0.7760317562606778852, 0.8765941196519888567, 1.000000000000001998 ) ) 
 REPRESENTATION_ITEM ( '' )  );
#10010 = CARTESIAN_POINT ( 'NONE',  ( -22.88419851978063591, -10.42888047092867865, 63.07185995612697837 ) ) ;
#10011 = DIRECTION ( 'NONE',  ( 3.549360974554993999E-17, -6.371834667797928663E-18, -1.000000000000000000 ) ) ;
#10012 = VERTEX_POINT ( 'NONE', #13418 ) ;
#10013 = CYLINDRICAL_SURFACE ( 'NONE', #46, 0.1500000000000009104 ) ;
#10014 = CARTESIAN_POINT ( 'NONE',  ( -24.84793648988037518, -14.18443574041886457, 69.83770584630335065 ) ) ;
#10015 = ORIENTED_EDGE ( 'NONE', *, *, #21286, .F. ) ;
#10016 = CARTESIAN_POINT ( 'NONE',  ( -13.35818949714929360, -21.05197827947291955, 61.70141596610112344 ) ) ;
#10017 = CARTESIAN_POINT ( 'NONE',  ( -16.25049964979334050, -21.71175520172467444, 61.94495303334971936 ) ) ;
#10018 = EDGE_LOOP ( 'NONE', ( #9860, #22151, #12995, #17928 ) ) ;
#10019 = CARTESIAN_POINT ( 'NONE',  ( -13.22450642086665873, -8.655658357931690361, 60.53976038923259750 ) ) ;
#10020 = DIRECTION ( 'NONE',  ( -0.6562885720885137664, 0.7545099801500437797, 1.193821363054684963E-08 ) ) ;
#10021 = CARTESIAN_POINT ( 'NONE',  ( -16.94458744105653381, -7.374567917109038362, 74.14513580114275726 ) ) ;
#10022 = CARTESIAN_POINT ( 'NONE',  ( -21.24554616535955631, -21.20453920045676810, 65.76949338751086316 ) ) ;
#10023 = ORIENTED_EDGE ( 'NONE', *, *, #1093, .F. ) ;
#10024 = FACE_OUTER_BOUND ( 'NONE', #34646, .T. ) ;
#10025 = UNCERTAINTY_MEASURE_WITH_UNIT (LENGTH_MEASURE( 1.000000000000000082E-05 ), #43856, 'distance_accuracy_value', 'NONE');
#10026 = CARTESIAN_POINT ( 'NONE',  ( -19.01558049692976482, -7.531172701354427623, 67.10082990693875615 ) ) ;
#10028 = EDGE_CURVE ( 'NONE', #24855, #23931, #27490, .T. ) ;
#10027 = CARTESIAN_POINT ( 'NONE',  ( -16.58751095051766455, -21.80939428823196025, 65.22564390318969174 ) ) ;
#10029 = ORIENTED_EDGE ( 'NONE', *, *, #23184, .T. ) ;
#10030 = CARTESIAN_POINT ( 'NONE',  ( -10.16417196683383217, -13.13632154568680477, 71.36861914326480871 ) ) ;
#10031 =( BOUNDED_CURVE ( )  B_SPLINE_CURVE ( 3, ( #17960, #32977, #2234, #48022 ),
 .UNSPECIFIED., .F., .F. ) 
 B_SPLINE_CURVE_WITH_KNOTS ( ( 4, 4 ),
 ( 0.000000000000000000, 0.4074455897393655102 ),
 .UNSPECIFIED. ) 
 CURVE ( )  GEOMETRIC_REPRESENTATION_ITEM ( )  RATIONAL_B_SPLINE_CURVE ( ( 1.000000000000000000, 0.4567392136813288595, 0.3561768502900291566, 0.6983129098261007250 ) ) 
 REPRESENTATION_ITEM ( '' )  );
#10032 = EDGE_CURVE ( 'NONE', #4358, #46391, #42760, .T. ) ;
#10033 = TOROIDAL_SURFACE ( 'NONE', #18655, 1.499999999999998224, 0.5000000000000000000 ) ;
#10034 = CARTESIAN_POINT ( 'NONE',  ( -24.77961554291793789, -15.99297619861334674, 66.22358246620183309 ) ) ;
#10035 = EDGE_CURVE ( 'NONE', #43753, #27411, #23552, .T. ) ;
#10036 = EDGE_CURVE ( 'NONE', #46554, #35531, #20086, .T. ) ;
#10037 = ORIENTED_EDGE ( 'NONE', *, *, #12809, .T. ) ;
#10038 = EDGE_LOOP ( 'NONE', ( #48294, #12256, #12435, #341 ) ) ;
#10039 = CARTESIAN_POINT ( 'NONE',  ( -23.40706900507760224, -18.44293855997280929, 73.06368236814604700 ) ) ;
#10040 = CARTESIAN_POINT ( 'NONE',  ( -17.42409385541299471, -14.80920654474435771, 49.52966884056655772 ) ) ;
#10041 = DIRECTION ( 'NONE',  ( 1.927470528863184130E-16, 1.434740771370715221E-29, -1.000000000000000000 ) ) ;
#10042 = AXIS2_PLACEMENT_3D ( 'NONE', #2019, #40410, #5960 ) ;
#10043 = CARTESIAN_POINT ( 'NONE',  ( -23.42981297399330742, -19.21767893247333348, 62.46132742258500770 ) ) ;
#10044 = CARTESIAN_POINT ( 'NONE',  ( -17.42409385541300892, -14.80920654474439679, 56.49999999999994316 ) ) ;
#10045 = CARTESIAN_POINT ( 'NONE',  ( -10.52215087187021325, -13.37195826583270808, 74.67817647370830514 ) ) ;
#10046 = CARTESIAN_POINT ( 'NONE',  ( -12.40421236734144728, -20.31415489762336435, 68.38011531907731921 ) ) ;
#10047 = VECTOR ( 'NONE', #29408, 1000.000000000000000 ) ;
#10048 = CARTESIAN_POINT ( 'NONE',  ( -23.13015969901951863, -18.95476373626217281, 58.76921843841908810 ) ) ;
#10049 = ORIENTED_EDGE ( 'NONE', *, *, #25936, .T. ) ;
#10050 = ORIENTED_EDGE ( 'NONE', *, *, #45821, .T. ) ;
#10051 = DIRECTION ( 'NONE',  ( 0.9687793358424822143, -0.2479245821708672415, 0.000000000000000000 ) ) ;
#10052 = CARTESIAN_POINT ( 'NONE',  ( -23.12041803196159506, -10.00762535718595991, 66.64908106505099283 ) ) ;
#10053 = CARTESIAN_POINT ( 'NONE',  ( -14.85449537034919132, -21.32098772481755944, 61.65217026632952013 ) ) ;
#10054 = DIRECTION ( 'NONE',  ( 0.4461977533473618363, -0.8949343913984794119, -2.476895096511287196E-17 ) ) ;
#10055 = CARTESIAN_POINT ( 'NONE',  ( -50.42609385541305755, -14.90920654474424367, 70.97647058823527288 ) ) ;
#10056 = CARTESIAN_POINT ( 'NONE',  ( -19.20534385650551457, -8.801233750844183135, 48.81488406609782515 ) ) ;
#10057 = ORIENTED_EDGE ( 'NONE', *, *, #24352, .T. ) ;
#10058 = EDGE_CURVE ( 'NONE', #32101, #18786, #14603, .T. ) ;
#10059 = CARTESIAN_POINT ( 'NONE',  ( -14.86587017669673649, -21.80700303724089295, 61.74945191855038473 ) ) ;
#10060 = SURFACE_STYLE_FILL_AREA ( #16704 ) ;
#10061 = CARTESIAN_POINT ( 'NONE',  ( -14.84764829735760649, -8.246537290690364230, 60.33468334944129197 ) ) ;
#10062 = AXIS2_PLACEMENT_3D ( 'NONE', #46895, #13137, #17073 ) ;
#10063 = CARTESIAN_POINT ( 'NONE',  ( -11.18327426895797494, -18.87804038469763768, 64.94045401417226060 ) ) ;
#10064 = ORIENTED_EDGE ( 'NONE', *, *, #13548, .F. ) ;
#10065 = AXIS2_PLACEMENT_3D ( 'NONE', #11972, #26981, #6519 ) ;
#10066 = VECTOR ( 'NONE', #45100, 1000.000000000000000 ) ;
#10067 = ADVANCED_FACE ( 'NONE', ( #36777 ), #33086, .T. ) ;
#10068 = FACE_OUTER_BOUND ( 'NONE', #16029, .T. ) ;
#10069 = DIRECTION ( 'NONE',  ( -1.000000000000000000, -2.866981220435666553E-17, 0.000000000000000000 ) ) ;
#10070 = CIRCLE ( 'NONE', #47821, 0.5000000000000004441 ) ;
#10071 = CARTESIAN_POINT ( 'NONE',  ( -16.93941734680482725, -7.775588144984237005, 74.24546186738449194 ) ) ;
#10072 = FACE_OUTER_BOUND ( 'NONE', #11166, .T. ) ;
#10073 = ORIENTED_EDGE ( 'NONE', *, *, #26946, .F. ) ;
#10074 = CARTESIAN_POINT ( 'NONE',  ( -19.08220441618011520, -7.953150065343516317, 59.96092815196451653 ) ) ;
#10075 = ORIENTED_EDGE ( 'NONE', *, *, #46856, .T. ) ;
#10076 = CARTESIAN_POINT ( 'NONE',  ( -11.47236213698566054, -10.32806074475630886, 74.55389686390628867 ) ) ;
#10077 = LINE ( 'NONE', #36398, #20929 ) ;
#10078 = ORIENTED_EDGE ( 'NONE', *, *, #7889, .F. ) ;
#10079 = CARTESIAN_POINT ( 'NONE',  ( -11.07857854458970692, -11.73724703412850801, 71.08860870961423473 ) ) ;
#10080 = CARTESIAN_POINT ( 'NONE',  ( -13.27409385650551599, -9.792211528768504536, 50.49490371617623197 ) ) ;
#10081 = ORIENTED_EDGE ( 'NONE', *, *, #30101, .T. ) ;
#10082 = CARTESIAN_POINT ( 'NONE',  ( -18.75616178366165698, -7.937006232909297410, 70.67068081708849547 ) ) ;
#10083 = CARTESIAN_POINT ( 'NONE',  ( -19.77283897654775657, -21.87935945976245122, 65.50840285157048015 ) ) ;
#10084 = CARTESIAN_POINT ( 'NONE',  ( -20.35492123770571382, -11.13690394275196560, 49.52966884056655772 ) ) ;
#10085 = EDGE_LOOP ( 'NONE', ( #44111, #9899, #42656, #36054, #44307 ) ) ;
#10086 = CARTESIAN_POINT ( 'NONE',  ( -17.64006181755907932, -7.293987387894279806, 54.02312124697527906 ) ) ;
#10087 = ADVANCED_FACE ( 'NONE', ( #7277 ), #2597, .F. ) ;
#10088 = CARTESIAN_POINT ( 'NONE',  ( -23.53886599083197240, -11.30005350631630279, 70.18650949724866450 ) ) ;
#10089 = FACE_OUTER_BOUND ( 'NONE', #35623, .T. ) ;
#10090 = CARTESIAN_POINT ( 'NONE',  ( -22.84116833803633284, -10.28479860924217704, 59.75770304231562591 ) ) ;
#10091 = EDGE_CURVE ( 'NONE', #28258, #45882, #28579, .T. ) ;
#10092 = ADVANCED_FACE ( 'NONE', ( #6774 ), #43686, .T. ) ;
#10093 = ORIENTED_EDGE ( 'NONE', *, *, #44150, .F. ) ;
#10094 = ORIENTED_EDGE ( 'NONE', *, *, #28474, .T. ) ;
#10095 = LINE ( 'NONE', #31536, #42458 ) ;
#10096 = CARTESIAN_POINT ( 'NONE',  ( -21.23484681875272884, -20.74088929683185611, 69.33978048267414351 ) ) ;
#10097 = ORIENTED_EDGE ( 'NONE', *, *, #2640, .T. ) ;
#10099 = CARTESIAN_POINT ( 'NONE',  ( -23.83080496556880945, -17.75212211224490133, 59.28906343887996400 ) ) ;
#10098 = VECTOR ( 'NONE', #33608, 1000.000000000000000 ) ;
#10100 = CARTESIAN_POINT ( 'NONE',  ( -20.41784385759799036, -6.860780111191487229, 51.02154966934377001 ) ) ;
#10101 = FACE_OUTER_BOUND ( 'NONE', #19683, .T. ) ;
#10102 = VECTOR ( 'NONE', #23626, 1000.000000000000114 ) ;
#10103 = CARTESIAN_POINT ( 'NONE',  ( -16.86552742978648212, -21.78694546712621616, 68.71063070142631091 ) ) ;
#10104 = CARTESIAN_POINT ( 'NONE',  ( -14.81535805098777736, -7.777528402031247623, 53.89198173725363716 ) ) ;
#10105 = CIRCLE ( 'NONE', #44733, 2.000000000000000000 ) ;
#10106 = AXIS2_PLACEMENT_3D ( 'NONE', #36821, #22075, #21826 ) ;
#10107 = VERTEX_POINT ( 'NONE', #10238 ) ;
#10108 = EDGE_CURVE ( 'NONE', #48382, #19712, #25253, .T. ) ;
#10109 = CARTESIAN_POINT ( 'NONE',  ( -10.56265612243206498, -13.42270443805417379, 74.67817617528319829 ) ) ;
#10110 = AXIS2_PLACEMENT_3D ( 'NONE', #37859, #37598, #19640 ) ;
#10111 = CARTESIAN_POINT ( 'NONE',  ( -14.66630222544869078, -8.320656262913125545, 63.80450889863892172 ) ) ;
#10112 = CARTESIAN_POINT ( 'NONE',  ( -16.55233368891663659, -22.20803663120749505, 65.32540755232676588 ) ) ;
#10113 = VERTEX_POINT ( 'NONE', #47897 ) ;
#10114 = VERTEX_POINT ( 'NONE', #36539 ) ;
#10115 = ADVANCED_FACE ( 'NONE', ( #29183 ), #48699, .T. ) ;
#10116 = FACE_OUTER_BOUND ( 'NONE', #38031, .T. ) ;
#10117 = CARTESIAN_POINT ( 'NONE',  ( -23.68301487380630377, -11.67430220541036867, 63.25218272174556944 ) ) ;
#10118 = CARTESIAN_POINT ( 'NONE',  ( -23.88493932675476472, -11.09942404494770152, 70.05244096366236306 ) ) ;
#10119 = VERTEX_POINT ( 'NONE', #7767 ) ;
#10120 = LINE ( 'NONE', #2002, #30611 ) ;
#10121 = CARTESIAN_POINT ( 'NONE',  ( -22.92319755143357440, -10.39759026177046941, 63.37185995336193400 ) ) ;
#10122 = ORIENTED_EDGE ( 'NONE', *, *, #47583, .F. ) ;
#10123 = CARTESIAN_POINT ( 'NONE',  ( -4.424093855413056886, -8.109206544744111511, 50.49999999999999289 ) ) ;
#10124 = VECTOR ( 'NONE', #13330, 1000.000000000000000 ) ;
#10125 = CARTESIAN_POINT ( 'NONE',  ( -12.89349882295773320, -9.473050026692668268, 71.07598649106860478 ) ) ;
#10126 = AXIS2_PLACEMENT_3D ( 'NONE', #14416, #32682, #44038 ) ;
#10127 = CARTESIAN_POINT ( 'NONE',  ( -15.75476274255337472, -8.011104503670525290, 67.36680511887003320 ) ) ;
#10128 = B_SPLINE_CURVE_WITH_KNOTS ( 'NONE', 3,
 ( #27343, #37428, #7679, #766, #30086, #45343, #22687, #11596, #3723, #15761 ),
 .UNSPECIFIED., .F., .F.,
 ( 4, 2, 2, 2, 4 ),
 ( 0.000000000000000000, 0.2500000000000000000, 0.5000000000000000000, 0.7500000000000000000, 1.000000000000000000 ),
 .UNSPECIFIED. ) ;
#10129 = ORIENTED_EDGE ( 'NONE', *, *, #41438, .T. ) ;
#10130 = CARTESIAN_POINT ( 'NONE',  ( -8.424093855413063991, -15.80920654474410725, 48.99999999999997868 ) ) ;
#10131 = AXIS2_PLACEMENT_3D ( 'NONE', #7458, #36968, #30109 ) ;
#10132 = CIRCLE ( 'NONE', #10909, 6.999999999999999112 ) ;
#10133 = ORIENTED_EDGE ( 'NONE', *, *, #3829, .T. ) ;
#10134 = CARTESIAN_POINT ( 'NONE',  ( -23.93648101794248362, -17.51022725521227841, 65.95829288617392194 ) ) ;
#10135 = FACE_OUTER_BOUND ( 'NONE', #36829, .T. ) ;
#10136 = CARTESIAN_POINT ( 'NONE',  ( -19.26582040957177355, -21.56270631561501006, 58.52507339225701344 ) ) ;
#10137 = VERTEX_POINT ( 'NONE', #26219 ) ;
#10138 = DIRECTION ( 'NONE',  ( 0.9687793358424821033, -0.2479245821708680464, 0.000000000000000000 ) ) ;
#10139 = CARTESIAN_POINT ( 'NONE',  ( -10.27345486655506868, -12.71824029969684844, 64.45331411623358520 ) ) ;
#10140 = CARTESIAN_POINT ( 'NONE',  ( -24.36611147337434957, -16.04009697885371111, 66.07797069094537790 ) ) ;
#10141 = AXIS2_PLACEMENT_3D ( 'NONE', #24450, #35509, #13087 ) ;
#10142 = DIRECTION ( 'NONE',  ( 0.7224352045700187519, 0.6914386272098739239, -9.340627245513716657E-09 ) ) ;
#10143 = CARTESIAN_POINT ( 'NONE',  ( -22.35721049598137711, -20.39193527001060957, 62.38439161571156433 ) ) ;
#10144 = DIRECTION ( 'NONE',  ( -0.06498076606345576378, -0.4424675129789833461, 0.8944271909999158554 ) ) ;
#10145 = ORIENTED_EDGE ( 'NONE', *, *, #25506, .T. ) ;
#10146 = CARTESIAN_POINT ( 'NONE',  ( -16.96567540528316442, -22.24509813497291333, 72.36532000937602049 ) ) ;
#10147 = CARTESIAN_POINT ( 'NONE',  ( -12.05806040642128707, -10.23620046216302448, 67.51368956197082127 ) ) ;
#10148 = CARTESIAN_POINT ( 'NONE',  ( -21.65914559189701194, -18.31838547852702703, 54.07175714974879099 ) ) ;
#10149 = CARTESIAN_POINT ( 'NONE',  ( -17.42409385541299471, -14.80920654474435594, 52.02966884056656482 ) ) ;
#10150 = CARTESIAN_POINT ( 'NONE',  ( -18.64167402801552242, -7.915852103407403639, 70.38570403504697026 ) ) ;
#10151 = CARTESIAN_POINT ( 'NONE',  ( -26.42409385541305511, -6.359206544744109735, 52.99999999999997158 ) ) ;
#10152 = EDGE_CURVE ( 'NONE', #44898, #30449, #46424, .T. ) ;
#10153 = ORIENTED_EDGE ( 'NONE', *, *, #3073, .F. ) ;
#10154 = ORIENTED_EDGE ( 'NONE', *, *, #46851, .T. ) ;
#10155 = CARTESIAN_POINT ( 'NONE',  ( -21.29994498387370427, -20.70774380606181708, 65.74020874375150925 ) ) ;
#10156 = FACE_OUTER_BOUND ( 'NONE', #28841, .T. ) ;
#10157 = VERTEX_POINT ( 'NONE', #45194 ) ;
#10158 = CARTESIAN_POINT ( 'NONE',  ( -24.34502428176253019, -17.56683243011407924, 66.12852677468319484 ) ) ;
#10160 = CARTESIAN_POINT ( 'NONE',  ( -11.75134185092603900, -18.91115923382153596, 71.70302575940529266 ) ) ;
#10159 = DIRECTION ( 'NONE',  ( -3.071710424422018668E-17, 6.404604876783312462E-16, 1.000000000000000000 ) ) ;
#10161 = CARTESIAN_POINT ( 'NONE',  ( -13.22576123393696967, -9.135673809461350103, 70.99358371225501685 ) ) ;
#10162 = CARTESIAN_POINT ( 'NONE',  ( -19.44222556512714917, -7.637678758653525968, 60.21738930846358073 ) ) ;
#10163 = CARTESIAN_POINT ( 'NONE',  ( -14.54176669294802693, -21.67913874359843973, 58.28122557424108408 ) ) ;
#10164 =( BOUNDED_CURVE ( )  B_SPLINE_CURVE ( 3, ( #43839, #28566, #43595, #21428 ),
 .UNSPECIFIED., .F., .F. ) 
 B_SPLINE_CURVE_WITH_KNOTS ( ( 4, 4 ),
 ( 0.9074455897393630677, 1.000000000000000000 ),
 .UNSPECIFIED. ) 
 CURVE ( )  GEOMETRIC_REPRESENTATION_ITEM ( )  RATIONAL_B_SPLINE_CURVE ( ( 0.6983129098260874024, 0.7760317562606933173, 0.8765941196519975165, 1.000000000000000000 ) ) 
 REPRESENTATION_ITEM ( '' )  );
#10165 = LINE ( 'NONE', #17766, #14192 ) ;
#10166 = DIRECTION ( 'NONE',  ( -2.866981220435666553E-17, 1.000000000000000000, 1.190614954331866791E-16 ) ) ;
#10167 = CARTESIAN_POINT ( 'NONE',  ( -47.17409385541305511, -15.81020654474410847, 70.50000000000000000 ) ) ;
#10168 = PLANE ( 'NONE',  #40498 ) ;
#10169 = EDGE_CURVE ( 'NONE', #47803, #29080, #25125, .T. ) ;
#10170 = EDGE_CURVE ( 'NONE', #11860, #14807, #18565, .T. ) ;
#10171 = CARTESIAN_POINT ( 'NONE',  ( -23.70099247935880982, -17.91057002971143675, 59.07548647231428163 ) ) ;
#10172 = EDGE_LOOP ( 'NONE', ( #18067, #20625, #24788, #32555, #9107 ) ) ;
#10173 = FACE_OUTER_BOUND ( 'NONE', #16834, .T. ) ;
#10174 = CARTESIAN_POINT ( 'NONE',  ( -15.90674806925635032, -7.920628488110523335, 70.90990109588881296 ) ) ;
#10175 = EDGE_CURVE ( 'NONE', #733, #1179, #3959, .T. ) ;
#10176 = AXIS2_PLACEMENT_3D ( 'NONE', #27045, #7621, #22627 ) ;
#10177 = EDGE_CURVE ( 'NONE', #35577, #32087, #26711, .T. ) ;
#10178 = CARTESIAN_POINT ( 'NONE',  ( -23.41977899678227004, -11.19648470850049904, 73.36193302072521760 ) ) ;
#10179 = AXIS2_PLACEMENT_3D ( 'NONE', #43053, #9332, #5879 ) ;
#10180 = CARTESIAN_POINT ( 'NONE',  ( -21.04010602215687342, -20.80440203143702149, 69.12620543858641042 ) ) ;
#10181 = CARTESIAN_POINT ( 'NONE',  ( -13.65110067086344792, -21.23324738024127356, 68.57129742521463811 ) ) ;
#10182 = CARTESIAN_POINT ( 'NONE',  ( -16.51569948449359515, -21.75045648492761430, 65.24181065036900407 ) ) ;
#10183 = B_SPLINE_CURVE_WITH_KNOTS ( 'NONE', 1,
 ( #34942, #1211 ),
 .UNSPECIFIED., .F., .F.,
 ( 2, 2 ),
 ( 0.000000000000000000, 1.000000000000000000 ),
 .UNSPECIFIED. ) ;
#10184 =( BOUNDED_CURVE ( )  B_SPLINE_CURVE ( 3, ( #20608, #27502, #5828, #9528 ),
 .UNSPECIFIED., .F., .F. ) 
 B_SPLINE_CURVE_WITH_KNOTS ( ( 4, 4 ),
 ( 0.5000000000000000000, 0.9074455897393653991 ),
 .UNSPECIFIED. ) 
 CURVE ( )  GEOMETRIC_REPRESENTATION_ITEM ( )  RATIONAL_B_SPLINE_CURVE ( ( 1.000000000000005551, 0.4567392136813330783, 0.3561768502900267697, 0.6983129098260927314 ) ) 
 REPRESENTATION_ITEM ( '' )  );
#10185 = AXIS2_PLACEMENT_3D ( 'NONE', #18239, #6932, #2742 ) ;
#10186 = ORIENTED_EDGE ( 'NONE', *, *, #29114, .T. ) ;
#10187 = ORIENTED_EDGE ( 'NONE', *, *, #35041, .F. ) ;
#10188 = CARTESIAN_POINT ( 'NONE',  ( -17.06784385541304516, -9.357632978295830739, 49.97845033065684106 ) ) ;
#10189 = ADVANCED_FACE ( 'NONE', ( #3813 ), #8245, .T. ) ;
#10190 = FACE_OUTER_BOUND ( 'NONE', #48418, .T. ) ;
#10191 = CARTESIAN_POINT ( 'NONE',  ( -11.88446955661387783, -10.44372876568607467, 67.38408161429789800 ) ) ;
#10192 = AXIS2_PLACEMENT_3D ( 'NONE', #46377, #31598, #31346 ) ;
#10193 =( BOUNDED_CURVE ( )  B_SPLINE_CURVE ( 3, ( #20247, #13562, #31331, #46360 ),
 .UNSPECIFIED., .F., .F. ) 
 B_SPLINE_CURVE_WITH_KNOTS ( ( 4, 4 ),
 ( 0.4074455897393697290, 0.5000000000000000000 ),
 .UNSPECIFIED. ) 
 CURVE ( )  GEOMETRIC_REPRESENTATION_ITEM ( )  RATIONAL_B_SPLINE_CURVE ( ( 0.6983129098261150469, 0.7760317562607150776, 0.8765941196520095069, 0.9999999999999966693 ) ) 
 REPRESENTATION_ITEM ( '' )  );
#10194 = DIRECTION ( 'NONE',  ( 0.9979768094191905359, 0.06357898915123233463, -6.487762650558261530E-18 ) ) ;
#10195 = CARTESIAN_POINT ( 'NONE',  ( -15.57436938376845603, -7.592477944586329741, 70.70966202169438475 ) ) ;
#10196 = EDGE_LOOP ( 'NONE', ( #5665, #19156, #28775, #27809 ) ) ;
#10197 = PLANE ( 'NONE',  #34660 ) ;
#10198 = CARTESIAN_POINT ( 'NONE',  ( -22.86447931068992290, -19.99836516962492183, 54.02312124697528617 ) ) ;
#10199 = ORIENTED_EDGE ( 'NONE', *, *, #44149, .T. ) ;
#10200 = CARTESIAN_POINT ( 'NONE',  ( -22.83929682888979329, -10.29453308790037980, 66.55654356380499337 ) ) ;
#10201 = FACE_OUTER_BOUND ( 'NONE', #11246, .T. ) ;
#10202 = VERTEX_POINT ( 'NONE', #37775 ) ;
#10203 = CARTESIAN_POINT ( 'NONE',  ( -17.77594298899184366, -7.367433885636743618, 60.26556189360973548 ) ) ;
#10204 = DIRECTION ( 'NONE',  ( -1.000000000000000000, 0.000000000000000000, 0.000000000000000000 ) ) ;
#10205 = FACE_OUTER_BOUND ( 'NONE', #40440, .T. ) ;
#10206 = ORIENTED_EDGE ( 'NONE', *, *, #47557, .T. ) ;
#10207 = DIRECTION ( 'NONE',  ( -0.1240347345892086062, 1.145860353393066553E-16, -0.9922778767136676281 ) ) ;
#10208 = DIRECTION ( 'NONE',  ( 3.071710424422018668E-17, -6.404604876783312462E-16, -1.000000000000000000 ) ) ;
#10209 = B_SPLINE_CURVE_WITH_KNOTS ( 'NONE', 1,
 ( #5299, #38533 ),
 .UNSPECIFIED., .F., .F.,
 ( 2, 2 ),
 ( 0.000000000000000000, 1.000000000000000000 ),
 .UNSPECIFIED. ) ;
#10210 = EDGE_CURVE ( 'NONE', #43576, #37207, #35175, .T. ) ;
#10211 = CARTESIAN_POINT ( 'NONE',  ( -10.69327888247252467, -16.91860816364039621, 61.24923186240393136 ) ) ;
#10212 = DIRECTION ( 'NONE',  ( -3.071710424422018668E-17, 6.404604876783312462E-16, 1.000000000000000000 ) ) ;
#10213 = ORIENTED_EDGE ( 'NONE', *, *, #1284, .T. ) ;
#10214 = CARTESIAN_POINT ( 'NONE',  ( -22.33161753753789469, -20.41455022152800325, 62.49085083065315160 ) ) ;
#10215 = VECTOR ( 'NONE', #46741, 1000.000000000000000 ) ;
#10216 = CARTESIAN_POINT ( 'NONE',  ( -21.57995947450667984, -9.113990939708573435, 70.14604673427196246 ) ) ;
#10217 = CARTESIAN_POINT ( 'NONE',  ( -12.03178671929730115, -10.26761072191531277, 67.49896879719585741 ) ) ;
#10218 = DIRECTION ( 'NONE',  ( 1.927470528863184130E-16, 1.434740771370715221E-29, -1.000000000000000000 ) ) ;
#10219 = CARTESIAN_POINT ( 'NONE',  ( -22.69284385650551883, -7.406986770994972602, 48.81910596585309747 ) ) ;
#10220 = EDGE_CURVE ( 'NONE', #37693, #4839, #38249, .T. ) ;
#10221 = PLANE ( 'NONE',  #7050 ) ;
#10222 = CARTESIAN_POINT ( 'NONE',  ( -12.01648161716052954, -10.28590799842451098, 67.79896869921920199 ) ) ;
#10223 = VERTEX_POINT ( 'NONE', #19310 ) ;
#10224 = DIRECTION ( 'NONE',  ( 0.000000000000000000, 0.000000000000000000, 1.000000000000000000 ) ) ;
#10225 = VECTOR ( 'NONE', #17918, 1000.000000000000114 ) ;
#10226 = DIRECTION ( 'NONE',  ( -1.000000000000000000, 0.000000000000000000, -0.000000000000000000 ) ) ;
#10227 = LINE ( 'NONE', #13405, #17214 ) ;
#10228 = VERTEX_POINT ( 'NONE', #30662 ) ;
#10229 = CARTESIAN_POINT ( 'NONE',  ( -17.02791773878522719, -7.770306534664505271, 73.96018283094906565 ) ) ;
#10230 = ORIENTED_EDGE ( 'NONE', *, *, #33305, .T. ) ;
#10231 = VERTEX_POINT ( 'NONE', #29918 ) ;
#10232 = ORIENTED_EDGE ( 'NONE', *, *, #3275, .F. ) ;
#10233 = VECTOR ( 'NONE', #26081, 1000.000000000000000 ) ;
#10234 = EDGE_CURVE ( 'NONE', #29199, #30767, #43299, .T. ) ;
#10235 = EDGE_CURVE ( 'NONE', #6219, #39482, #38023, .T. ) ;
#10236 = CARTESIAN_POINT ( 'NONE',  ( -23.72107644662085590, -11.75175493167614427, 59.59121838756593803 ) ) ;
#10237 = CARTESIAN_POINT ( 'NONE',  ( -16.00334498133122096, -7.954840756278199088, 63.95545613112251004 ) ) ;
#10238 = CARTESIAN_POINT ( 'NONE',  ( -18.47956468449850931, -19.37530592812942842, 49.52966884056656482 ) ) ;
#10239 = VERTEX_POINT ( 'NONE', #601 ) ;
#10240 = EDGE_LOOP ( 'NONE', ( #48353, #27571, #9568, #8456 ) ) ;
#10241 = EDGE_CURVE ( 'NONE', #18786, #26541, #5166, .T. ) ;
#10242 = CARTESIAN_POINT ( 'NONE',  ( -18.95534385650551457, -7.417179338643134834, 52.18511593390279302 ) ) ;
#10243 = CONICAL_SURFACE ( 'NONE', #1581, 0.5560000000000009379, 0.06981317007976595157 ) ;
#10244 = FACE_OUTER_BOUND ( 'NONE', #47889, .T. ) ;
#10245 = CIRCLE ( 'NONE', #4757, 5.249999999999998224 ) ;
#10246 = ADVANCED_FACE ( 'NONE', ( #12653 ), #42463, .T. ) ;
#10247 = CARTESIAN_POINT ( 'NONE',  ( -19.63034385650551883, -9.794322478646142471, 51.19202720610083901 ) ) ;
#10248 = VECTOR ( 'NONE', #27303, 1000.000000000000000 ) ;
#10249 = VERTEX_POINT ( 'NONE', #43187 ) ;
#10250 = CARTESIAN_POINT ( 'NONE',  ( -15.39235221195410652, -21.97689038623625635, 72.08929527613493349 ) ) ;
#10251 = CARTESIAN_POINT ( 'NONE',  ( -24.87421248883078917, -14.80150407957441061, 59.36487506370225731 ) ) ;
#10252 = AXIS2_PLACEMENT_3D ( 'NONE', #13364, #34813, #16085 ) ;
#10253 = ORIENTED_EDGE ( 'NONE', *, *, #12071, .F. ) ;
#10254 = DIRECTION ( 'NONE',  ( 4.924618305738831318E-06, 4.007739938527551184E-06, 0.9999999999798430128 ) ) ;
#10255 = ORIENTED_EDGE ( 'NONE', *, *, #40879, .F. ) ;
#10256 = DIRECTION ( 'NONE',  ( 0.9687793358424819923, -0.2479245821708680464, 0.000000000000000000 ) ) ;
#10257 = CARTESIAN_POINT ( 'NONE',  ( -10.43158760916531591, -13.88200553355761713, 61.21821478144431694 ) ) ;
#10258 = CARTESIAN_POINT ( 'NONE',  ( -9.995738443926455830, -14.24059931954510816, 64.50308448303212572 ) ) ;
#10259 = CLOSED_SHELL ( 'NONE', ( #22850, #44015, #137, #21554, #22902, #37205, #46705, #44406, #40620, #40007, #20806, #22460, #11338, #27811, #5679, #13135, #8518, #22405, #20876, #19507, #7659, #28880, #21414, #8616, #10502, #21618, #44668, #24572, #47905, #1636, #2540, #488, #5668, #32169, #18750, #28499, #22292, #22398, #35834, #9384, #42155, #6273, #24561, #16350, #38827, #44060, #32773, #27136, #18460, #34621, #48289, #16761, #22922, #34561, #18375, #17902, #29264, #47146, #21453, #45135, #3108, #28587, #33489, #44343, #18521, #10754, #35895, #26377, #38576, #7473, #19318, #25436, #16992, #40760, #34213, #32757, #47923, #48138, #17777, #28173, #16710, #3597, #25773, #1547, #34421, #3269, #42832, #28006, #44818, #20661, #7599, #4958, #11825, #15594, #42264, #20049, #42571, #21952, #31634, #37403, #2316, #37701, #23011, #22077, #29985, #36115, #14279, #39383, #10919, #38514, #26267, #23458, #24571, #265, #35438, #25966, #25868, #20825, #24419, #48500, #40344, #37964, #38512, #11438, #20991, #45091, #2798, #18262, #6423, #35649, #3000, #9702, #9410, #11441, #26855, #9791, #843, #45783, #19206, #6546, #42647, #8467, #24730, #30680, #28687, #32076, #974, #43058, #4914, #38236, #9216, #5928, #41559, #36433, #9289, #8333, #10832, #1909, #21683, #43112, #15723, #14010, #46034, #3374, #28894, #21013, #46197, #36973, #36647, #42963, #41864, #23350, #46297, #42574, #20877, #15921, #30002, #38719, #35837, #12678, #26921, #30753, #3473, #3203, #5238, #26116, #34820, #7728, #32181, #41710, #6836, #1813, #8603, #9192, #3664, #28449, #41612, #38999, #31034, #8879, #29745, #8140, #25053, #41797, #27471, #18183, #13627, #34210, #6212, #13288, #42955, #24849, #24358, #43179, #14437, #22359, #40434, #13674, #5977, #25674, #40994, #42287, #15236, #15244, #2711, #47471, #34616, #8443, #15738, #4706, #31990, #20323, #43079, #28040, #10837, #28556, #16050, #40097, #37588, #17912, #20406, #10115, #28386, #12008, #42646, #14572, #16912, #26400, #44263, #16759, #31640, #14085, #36591, #47485, #4021, #24019, #20674, #40209, #984, #2241, #37828, #40690, #23616, #22916, #33453, #3907, #28220, #4426, #25409, #5203, #19092, #15970, #38106, #43454, #15813, #33367, #5604, #17282, #43733, #19616, #14138, #46632, #20537, #32307, #17239, #13410, #17373, #45426, #20526, #12651, #9844, #11445, #18758, #39183, #17308, #24426, #40756, #35563, #45604, #41076, #22701, #43015, #32564, #25169, #45349, #17421, #13826, #36039, #18128, #15299, #47189, #22807, #20518, #6141, #29038, #28348, #8132, #24294, #29657, #15742, #31476, #29073, #43444, #47861, #12780, #3138, #31376, #13371, #13176, #21675, #20838, #23126, #27416, #24260, #39820, #2, #17023, #7493, #43318, #33323, #41454, #47852, #29395, #21471, #9435, #42033, #15452, #23088, #33235, #12534, #18633, #17313, #19910, #16258, #17717, #5529, #4767, #27437, #21005, #8194, #36930, #28450, #34148, #23737, #15428, #37296, #5320, #22981, #23674, #37622, #32595, #46710, #13253, #37708, #47598, #39343, #22037, #22372, #26029, #25459, #27716, #32662, #1665, #3758, #1849, #27210, #34012, #32341, #14658, #36316, #3553, #10666, #43687, #43032, #33954, #47338, #15916, #39466, #20400, #45242, #7979, #12982, #5982, #39774, #21789, #15870, #2909, #21211, #39740, #22348, #15401, #2438, #46290, #13431, #15315, #36107, #47466, #41643, #13946, #33047, #31773, #29518, #12215, #33577, #8798, #24229, #36927, #21421, #31159, #11952, #32313, #1258, #9585, #39414, #30269, #283, #16413, #29120, #35073, #46439, #2919, #31285, #22999, #437, #42019, #42309, #7031, #46239, #15398, #16131, #35508, #15629, #37053, #19090, #25698, #21672, #36267, #2225, #32837, #8129, #28072, #44269, #10377, #22534, #33104, #31134, #35155, #8077, #14309, #9635, #2780, #11588, #17152, #5674, #24164, #34059, #9112, #3460, #32794, #14361, #18586, #33247, #4678, #13210, #12590, #30558, #16809, #23885, #13732, #9066, #893, #21446, #46405, #4617, #17842, #31651, #7453, #32395, #22234, #13621, #6049, #31230, #27877, #25616, #39897, #32623, #45273, #10461, #2323, #4723, #27846, #6073, #277, #2532, #40439, #11047, #31618, #1638, #21344, #29015, #39361, #338, #825, #39615, #7378, #24509, #5041, #22787, #5103, #3841, #43509, #33635, #4897, #17926, #39484, #28379, #47785, #157, #43237, #47782, #23889, #556, #11883, #2424, #27951, #39750, #42018, #13181, #48630, #13567, #38591, #14552, #7859, #39118, #438, #14829, #25490, #2321, #10700, #44943, #21606, #30401, #19603, #16804, #22016, #32582, #16078, #22580, #5061, #44609, #39755, #42351, #19930, #12731, #10827, #9640, #5997, #19374, #46698, #26016, #22353, #41648, #27069, #1293, #27616, #24505, #10824, #26690, #26782, #18042, #15186, #29739, #17165, #39800, #8249, #23392, #10562, #29210, #35318, #10643, #43374, #41408, #1427, #6665, #28002, #13003, #1440, #21261, #2238, #37006, #34361, #606, #45408, #27889, #4490, #24831, #19352, #7287, #39677, #22962, #30636, #14091, #19994, #26322, #5282, #2187, #35922, #11948, #15534, #3879, #37084, #24772, #13623, #41743, #16149, #36388, #42510, #45035, #36573, #48729, #20417, #13052, #3820, #8511, #12808, #36719, #28634, #18508, #47297, #15431, #15812, #17366, #8495, #30208, #8561, #17631, #32843, #13687, #17090, #35782, #26731, #37222, #20321, #2538, #41221, #1345, #10780, #36998, #29942, #48020, #34484, #18532, #28515, #42700, #19548, #44948, #5374, #28691, #4044, #21885, #7950, #8066, #43710, #44894, #45503, #42632, #4228, #4367, #1322, #2910, #24349, #21571, #14066, #43459, #17518, #31520, #36153, #5526, #43073, #43787, #34892, #26602, #15251, #14142, #7653, #34182, #12823, #30422, #39059, #18892, #28944, #39674, #19135, #6682, #14337, #926, #13201, #6808, #9398, #33977, #11184, #8752, #43405, #31128, #29871, #19849, #46850, #22420, #40972, #38161, #36704, #31172, #48720, #11269, #45052, #10092, #10067, #10710, #23005, #945, #30715, #19437, #45427, #48378, #15074, #11388, #14965, #29880, #9129, #10318, #26321, #6669, #30023, #29056, #32933, #9430, #16315, #25192, #35374, #5393, #16154, #4049, #21065, #29362, #14971, #3408, #4878, #37659, #33137, #34593, #45210, #28364, #36522, #14418, #14667, #29063, #43869, #19986, #45373, #23940, #9823, #29180, #24861, #34334, #28172, #22267, #23206, #44795, #47380, #14489, #44329, #6142, #4917, #35312, #40686, #1411, #2185, #34849, #32126, #39419, #12063, #8740, #34500, #24995, #24560, #20606, #47606, #45758, #22796, #17646, #47192, #29187, #1639, #42633, #11788, #27204, #25990, #8743, #41235, #4586, #31020, #25828, #12758, #38522, #20550, #36675, #19167, #7413, #14386, #11532, #2050, #48130, #42433, #32028, #32973 ) ) ;
#10260 = ORIENTED_EDGE ( 'NONE', *, *, #4498, .F. ) ;
#10261 = DIRECTION ( 'NONE',  ( 1.224646799147353207E-16, 1.000000000000000000, -1.912410701131276611E-32 ) ) ;
#10262 =( BOUNDED_CURVE ( )  B_SPLINE_CURVE ( 3, ( #44491, #30450, #10993, #14640 ),
 .UNSPECIFIED., .F., .F. ) 
 B_SPLINE_CURVE_WITH_KNOTS ( ( 4, 4 ),
 ( 0.5000000000000000000, 0.9074455897393685078 ),
 .UNSPECIFIED. ) 
 CURVE ( )  GEOMETRIC_REPRESENTATION_ITEM ( )  RATIONAL_B_SPLINE_CURVE ( ( 0.9999999999999921174, 0.4567392136813224202, 0.3561768502900321542, 0.6983129098261128265 ) ) 
 REPRESENTATION_ITEM ( '' )  );
#10263 = EDGE_CURVE ( 'NONE', #12881, #25767, #40225, .T. ) ;
#10264 = CARTESIAN_POINT ( 'NONE',  ( -22.78885683033217902, -10.31261690998277381, 63.26289122890993610 ) ) ;
#10265 = DIRECTION ( 'NONE',  ( 0.9687793358424817702, -0.2479245821708688791, 0.000000000000000000 ) ) ;
#10266 = VERTEX_POINT ( 'NONE', #38506 ) ;
#10267 = DIRECTION ( 'NONE',  ( -3.071710424422018668E-17, 6.404604876783312462E-16, 1.000000000000000000 ) ) ;
#10268 = DIRECTION ( 'NONE',  ( 1.590464103011092396E-07, -3.579926632912963412E-07, 0.9999999999999231726 ) ) ;
#10269 = CARTESIAN_POINT ( 'NONE',  ( -23.91010245674826251, -17.57297063409389537, 62.75888927877479517 ) ) ;
#10270 = ORIENTED_EDGE ( 'NONE', *, *, #12721, .F. ) ;
#10271 = CARTESIAN_POINT ( 'NONE',  ( -13.72009916595086132, -20.81131062084115513, 61.40157432139535842 ) ) ;
#10272 = B_SPLINE_CURVE_WITH_KNOTS ( 'NONE', 1,
 ( #10427, #2772 ),
 .UNSPECIFIED., .F., .F.,
 ( 2, 2 ),
 ( 0.000000000000000000, 1.000000000000000000 ),
 .UNSPECIFIED. ) ;
#10273 = ORIENTED_EDGE ( 'NONE', *, *, #32771, .F. ) ;
#10274 = DIRECTION ( 'NONE',  ( -5.731567514496413899E-31, -1.020425574103664789E-16, -1.000000000000000000 ) ) ;
#10275 = CARTESIAN_POINT ( 'NONE',  ( -24.44253391677669285, -17.31023895159264470, 73.06991310009190954 ) ) ;
#10276 = CARTESIAN_POINT ( 'NONE',  ( -22.68242704663779108, -10.18794451883025154, 70.29561946466137101 ) ) ;
#10277 = EDGE_LOOP ( 'NONE', ( #27575, #7237, #25909, #11918, #35859 ) ) ;
#10278 = DIRECTION ( 'NONE',  ( -0.3688590060343657218, 0.9294853595766530141, 0.000000000000000000 ) ) ;
#10279 = DIRECTION ( 'NONE',  ( -3.071710424422018668E-17, 6.404604876783312462E-16, 1.000000000000000000 ) ) ;
#10280 = ORIENTED_EDGE ( 'NONE', *, *, #34771, .F. ) ;
#10281 = AXIS2_PLACEMENT_3D ( 'NONE', #45406, #23241, #41949 ) ;
#10282 = FACE_OUTER_BOUND ( 'NONE', #36666, .T. ) ;
#10283 = ORIENTED_EDGE ( 'NONE', *, *, #25985, .F. ) ;
#10284 = ORIENTED_EDGE ( 'NONE', *, *, #44681, .F. ) ;
#10285 = DIRECTION ( 'NONE',  ( 0.000000000000000000, 0.000000000000000000, 1.000000000000000000 ) ) ;
#10286 = ADVANCED_FACE ( 'NONE', ( #31621 ), #1815, .T. ) ;
#10287 = DIRECTION ( 'NONE',  ( 0.9687793358424804380, -0.2479245821708739583, 0.000000000000000000 ) ) ;
#10288 = B_SPLINE_CURVE_WITH_KNOTS ( 'NONE', 3,
 ( #47538, #23927, #42879, #9146, #8909, #39421, #46812, #32029, #43116, #39899 ),
 .UNSPECIFIED., .F., .F.,
 ( 4, 2, 2, 2, 4 ),
 ( 0.000000000000000000, 0.2500000000000000000, 0.5000000000000000000, 0.7500000000000000000, 1.000000000000000000 ),
 .UNSPECIFIED. ) ;
#10289 = VECTOR ( 'NONE', #43254, 999.9999999999998863 ) ;
#10290 = CARTESIAN_POINT ( 'NONE',  ( -10.13751350317288669, -13.25697809452625009, 74.93463578866538910 ) ) ;
#10291 = CARTESIAN_POINT ( 'NONE',  ( -19.37484620200115160, -7.619050568204919216, 60.14588398245204814 ) ) ;
#10292 = CARTESIAN_POINT ( 'NONE',  ( -23.81024772113315890, -18.64597811008791695, 72.94863512192290500 ) ) ;
#10293 = CYLINDRICAL_SURFACE ( 'NONE', #3517, 0.1499999999999998002 ) ;
#10294 = CARTESIAN_POINT ( 'NONE',  ( -22.65953014494242979, -19.53520302830625965, 72.52911954723420251 ) ) ;
#10295 = VERTEX_POINT ( 'NONE', #16815 ) ;
#10296 = VERTEX_POINT ( 'NONE', #20541 ) ;
#10297 = EDGE_CURVE ( 'NONE', #34062, #43456, #5274, .T. ) ;
#10298 = CARTESIAN_POINT ( 'NONE',  ( -10.42334066387008029, -15.64104445138816146, 61.03789045260960222 ) ) ;
#10299 = AXIS2_PLACEMENT_3D ( 'NONE', #38035, #37292, #38267 ) ;
#10300 = CARTESIAN_POINT ( 'NONE',  ( -17.18707620353899301, -7.362977788511615884, 70.64035839947293027 ) ) ;
#10301 = PLANE ( 'NONE',  #18133 ) ;
#10302 = FACE_OUTER_BOUND ( 'NONE', #18054, .T. ) ;
#10303 = EDGE_CURVE ( 'NONE', #9962, #20146, #17330, .T. ) ;
#10304 = CARTESIAN_POINT ( 'NONE',  ( -18.54561167675666411, -7.443937692776573911, 73.97917849299003024 ) ) ;
#10305 = CARTESIAN_POINT ( 'NONE',  ( -20.33034385650551812, -9.794322478646142471, 51.19202720610083901 ) ) ;
#10306 = VERTEX_POINT ( 'NONE', #46643 ) ;
#10307 = CARTESIAN_POINT ( 'NONE',  ( -14.80056043599933524, -21.78207186541723317, 61.82095768364339960 ) ) ;
#10308 = SURFACE_STYLE_USAGE ( .BOTH. , #17439 ) ;
#10309 = AXIS2_PLACEMENT_3D ( 'NONE', #39284, #8283, #23301 ) ;
#10310 = CARTESIAN_POINT ( 'NONE',  ( -14.47651980493331081, -8.396190447208750740, 60.47563573450432273 ) ) ;
#10311 = CARTESIAN_POINT ( 'NONE',  ( -19.04501905262167227, -19.80271247795941392, 49.52966884056656482 ) ) ;
#10312 =( BOUNDED_CURVE ( )  B_SPLINE_CURVE ( 3, ( #40976, #48598, #22504, #48118 ),
 .UNSPECIFIED., .F., .F. ) 
 B_SPLINE_CURVE_WITH_KNOTS ( ( 4, 4 ),
 ( 0.000000000000000000, 0.4074455897393696735 ),
 .UNSPECIFIED. ) 
 CURVE ( )  GEOMETRIC_REPRESENTATION_ITEM ( )  RATIONAL_B_SPLINE_CURVE ( ( 1.000000000000000000, 0.4567392136813212544, 0.3561768502900263256, 0.6983129098261152690 ) ) 
 REPRESENTATION_ITEM ( '' )  );
#10313 = ADVANCED_FACE ( 'NONE', ( #20289 ), #5034, .T. ) ;
#10314 = VERTEX_POINT ( 'NONE', #27429 ) ;
#10315 = VECTOR ( 'NONE', #20784, 1000.000000000000000 ) ;
#10316 = EDGE_CURVE ( 'NONE', #23071, #18406, #39488, .T. ) ;
#10317 = DIRECTION ( 'NONE',  ( 1.000000000000000000, 0.000000000000000000, -8.260587980841940012E-17 ) ) ;
#10318 = ADVANCED_FACE ( 'NONE', ( #32099 ), #46147, .T. ) ;
#10319 = CARTESIAN_POINT ( 'NONE',  ( -22.48964968825576705, -9.905448439006629968, 73.76689030015370463 ) ) ;
#10320 = DIRECTION ( 'NONE',  ( -3.071710424422018668E-17, 6.404604876783312462E-16, 1.000000000000000000 ) ) ;
#10321 = B_SPLINE_CURVE_WITH_KNOTS ( 'NONE', 3,
 ( #9260, #13416, #39773, #39535, #24286, #2348, #6040, #17358, #39293, #43729 ),
 .UNSPECIFIED., .F., .F.,
 ( 4, 2, 2, 2, 4 ),
 ( 0.000000000000000000, 0.2500000000000000000, 0.5000000000000000000, 0.7500000000000000000, 1.000000000000000000 ),
 .UNSPECIFIED. ) ;
#10322 = ORIENTED_EDGE ( 'NONE', *, *, #752, .T. ) ;
#10323 = CARTESIAN_POINT ( 'NONE',  ( -14.92409385541305333, -14.80920654474410725, 81.99999999999998579 ) ) ;
#10324 =( BOUNDED_SURFACE ( )  B_SPLINE_SURFACE ( 3, 1, ( 
 ( #2558, #33049 ),
 ( #17557, #36986 ),
 ( #6498, #21747 ),
 ( #29136, #6973 ),
 ( #3278, #32816 ),
 ( #25676, #48323 ),
 ( #41191, #48092 ) ),
 .UNSPECIFIED., .T., .F., .F. ) 
 B_SPLINE_SURFACE_WITH_KNOTS ( ( 4, 3, 4 ),
 ( 2, 2 ),
 ( 0.000000000000000000, 0.5000000000000000000, 1.000000000000000000 ),
 ( 0.000000000000000000, 1.000000000000000000 ),
 .UNSPECIFIED. ) 
 GEOMETRIC_REPRESENTATION_ITEM ( )  RATIONAL_B_SPLINE_SURFACE ( (
 ( 1.000000000000000000, 1.000000000000000000),
 ( 0.3333333333333335369, 0.3333333333333330373),
 ( 0.3333333333333335369, 0.3333333333333330373),
 ( 1.000000000000000000, 1.000000000000000000),
 ( 0.3333333333333333703, 0.3333333333333333703),
 ( 0.3333333333333333703, 0.3333333333333333703),
 ( 1.000000000000000000, 1.000000000000000000) ) ) 
 REPRESENTATION_ITEM ( '' )  SURFACE ( )  );
#10325 = ORIENTED_EDGE ( 'NONE', *, *, #24685, .T. ) ;
#10326 = CARTESIAN_POINT ( 'NONE',  ( -22.28468842640967651, -19.91619389767071269, 65.98949666203347419 ) ) ;
#10327 = LINE ( 'NONE', #26307, #20963 ) ;
#10328 = B_SPLINE_CURVE_WITH_KNOTS ( 'NONE', 1,
 ( #42115, #19950 ),
 .UNSPECIFIED., .F., .F.,
 ( 2, 2 ),
 ( 0.000000000000000000, 1.000000000000000000 ),
 .UNSPECIFIED. ) ;
#10329 = ORIENTED_EDGE ( 'NONE', *, *, #19969, .T. ) ;
#10330 = DIRECTION ( 'NONE',  ( -3.071710424422018668E-17, 6.404604876783312462E-16, 1.000000000000000000 ) ) ;
#10331 = AXIS2_PLACEMENT_3D ( 'NONE', #21816, #14632, #14886 ) ;
#10332 = CARTESIAN_POINT ( 'NONE',  ( -12.95250271175661183, -20.26353575427058828, 71.69165012371371404 ) ) ;
#10333 = VERTEX_POINT ( 'NONE', #16326 ) ;
#10334 = CARTESIAN_POINT ( 'NONE',  ( -22.38400322090610217, -20.36826016184844335, 62.41934579407823236 ) ) ;
#10335 = CARTESIAN_POINT ( 'NONE',  ( -40.92409385541305511, -14.80920654474410725, 74.99999999999998579 ) ) ;
#10336 = CARTESIAN_POINT ( 'NONE',  ( -19.94917705995926482, -8.226604131702123013, 74.00624557436877637 ) ) ;
#10337 = ORIENTED_EDGE ( 'NONE', *, *, #37031, .F. ) ;
#10338 = CARTESIAN_POINT ( 'NONE',  ( -13.53325622885376944, -21.16256470055228789, 65.17124264509627096 ) ) ;
#10339 = CARTESIAN_POINT ( 'NONE',  ( -17.29268214306257434, -7.359616301281327821, 70.67691090883880634 ) ) ;
#10340 = CARTESIAN_POINT ( 'NONE',  ( -17.97037870217379307, -19.46375863019785513, 49.52966884056656482 ) ) ;
#10341 = AXIS2_PLACEMENT_3D ( 'NONE', #18210, #7650, #262 ) ;
#10342 = CARTESIAN_POINT ( 'NONE',  ( 6.575906144586949331, -8.109206544743660316, 50.50000000000031264 ) ) ;
#10343 = ORIENTED_EDGE ( 'NONE', *, *, #22169, .F. ) ;
#10344 = VERTEX_POINT ( 'NONE', #12406 ) ;
#10345 = AXIS2_PLACEMENT_3D ( 'NONE', #18199, #25846, #44334 ) ;
#10346 = CARTESIAN_POINT ( 'NONE',  ( -22.48964968825576705, -9.905448439006629968, 73.76689030015370463 ) ) ;
#10347 = CARTESIAN_POINT ( 'NONE',  ( -24.68275079258767235, -16.48720463981601370, 59.23837148777906236 ) ) ;
#10348 = ORIENTED_EDGE ( 'NONE', *, *, #18691, .T. ) ;
#10349 = DIRECTION ( 'NONE',  ( 0.8788484374452878445, -0.3260506722428093695, 0.3483050145059469749 ) ) ;
#10350 = CARTESIAN_POINT ( 'NONE',  ( -14.56784385759798894, -9.357632978295830739, 49.97845033065684106 ) ) ;
#10351 = DIRECTION ( 'NONE',  ( -0.3688590060343657773, 0.9294853595766529031, 0.000000000000000000 ) ) ;
#10352 = CARTESIAN_POINT ( 'NONE',  ( -12.95651447042595095, -9.351591191262567548, 67.26453940287311184 ) ) ;
#10353 = CARTESIAN_POINT ( 'NONE',  ( -23.70429433613102432, -18.81713154275495370, 69.47088838593184335 ) ) ;
#10354 = VECTOR ( 'NONE', #6011, 1000.000000000000000 ) ;
#10355 = VERTEX_POINT ( 'NONE', #1085 ) ;
#10356 = EDGE_CURVE ( 'NONE', #39133, #30449, #34540, .T. ) ;
#10357 = CARTESIAN_POINT ( 'NONE',  ( -21.97751765269923041, -20.19167113790911827, 59.05883102620609293 ) ) ;
#10358 = CARTESIAN_POINT ( 'NONE',  ( -14.10256296019058198, -8.140532706836228982, 70.84462314181931220 ) ) ;
#10359 = EDGE_CURVE ( 'NONE', #34367, #31776, #1524, .T. ) ;
#10360 = VECTOR ( 'NONE', #21630, 1000.000000000000000 ) ;
#10361 = FACE_OUTER_BOUND ( 'NONE', #35168, .T. ) ;
#10362 = CARTESIAN_POINT ( 'NONE',  ( -16.57554889599778747, -22.21081103083016117, 65.41059783760971413 ) ) ;
#10363 = ORIENTED_EDGE ( 'NONE', *, *, #10008, .T. ) ;
#10364 = VERTEX_POINT ( 'NONE', #9212 ) ;
#10365 = CARTESIAN_POINT ( 'NONE',  ( -20.58212643533483543, -8.561992128821106718, 60.06798555086853497 ) ) ;
#10366 = VECTOR ( 'NONE', #45829, 1000.000000000000000 ) ;
#10367 = DIRECTION ( 'NONE',  ( -0.1240347345892086200, 1.145860353393066553E-16, -0.9922778767136676281 ) ) ;
#10368 = CARTESIAN_POINT ( 'NONE',  ( -50.42609385541305755, -14.90920654474425433, 71.08235294117645253 ) ) ;
#10369 = CARTESIAN_POINT ( 'NONE',  ( -11.67943375510494874, -18.89645239624664796, 68.50217487844219022 ) ) ;
#10370 = ORIENTED_EDGE ( 'NONE', *, *, #44467, .T. ) ;
#10371 = EDGE_CURVE ( 'NONE', #22230, #36064, #5785, .T. ) ;
#10372 = CARTESIAN_POINT ( 'NONE',  ( -16.20608744287016023, -7.459440102232786529, 60.40039685254514978 ) ) ;
#10373 = VECTOR ( 'NONE', #24305, 1000.000000000000114 ) ;
#10374 = CARTESIAN_POINT ( 'NONE',  ( -19.05047292022263505, -10.41396213884962840, 49.52966884056655772 ) ) ;
#10375 = EDGE_CURVE ( 'NONE', #23048, #9317, #6564, .T. ) ;
#10376 = EDGE_CURVE ( 'NONE', #10119, #7399, #10657, .T. ) ;
#10377 = ADVANCED_FACE ( 'NONE', ( #25664 ), #39726, .T. ) ;
#10378 = ORIENTED_EDGE ( 'NONE', *, *, #41515, .T. ) ;
#10379 = CIRCLE ( 'NONE', #31615, 2.000000000000001776 ) ;
#10380 = CARTESIAN_POINT ( 'NONE',  ( -22.33041860316855320, -20.41560964288588664, 62.34943852502606632 ) ) ;
#10381 = CARTESIAN_POINT ( 'NONE',  ( -24.46737407909346373, -14.43901797238471474, 62.59807894131280648 ) ) ;
#10382 = CARTESIAN_POINT ( 'NONE',  ( -21.94839310389095033, -8.890257795104481886, 66.85488308860405482 ) ) ;
#10383 = ORIENTED_EDGE ( 'NONE', *, *, #12231, .F. ) ;
#10384 = FACE_OUTER_BOUND ( 'NONE', #44448, .T. ) ;
#10385 = ORIENTED_EDGE ( 'NONE', *, *, #11882, .T. ) ;
#10386 = CARTESIAN_POINT ( 'NONE',  ( -24.47066272824306665, -14.57993217219608972, 62.99824437345091610 ) ) ;
#10387 = CARTESIAN_POINT ( 'NONE',  ( -18.61784385759798965, -6.860780111191480124, 51.02154966934376290 ) ) ;
#10388 = CARTESIAN_POINT ( 'NONE',  ( -22.29619887594318683, -17.36118473213641167, 53.49999999999995026 ) ) ;
#10389 = ORIENTED_EDGE ( 'NONE', *, *, #8608, .T. ) ;
#10390 = DIRECTION ( 'NONE',  ( -0.7171836970970658642, 0.6968841687240311389, -4.479616660400631173E-09 ) ) ;
#10391 = CARTESIAN_POINT ( 'NONE',  ( -24.45125044792649049, -12.33277093510790579, 73.35570258362008644 ) ) ;
#10392 = CARTESIAN_POINT ( 'NONE',  ( -22.83659385650551954, -6.915538690918074494, 49.31353937987644542 ) ) ;
#10393 = CARTESIAN_POINT ( 'NONE',  ( -10.75331649400429868, -16.93069871048427544, 57.68760548944693056 ) ) ;
#10394 = CARTESIAN_POINT ( 'NONE',  ( -42.68438797306012589, -14.80920654474413745, 60.91764705882351905 ) ) ;
#10395 = DIRECTION ( 'NONE',  ( 3.413470714839332458E-33, -1.190614954331866791E-16, 1.000000000000000000 ) ) ;
#10396 = ORIENTED_EDGE ( 'NONE', *, *, #20607, .F. ) ;
#10397 = CARTESIAN_POINT ( 'NONE',  ( -24.72409385541305582, -14.80920654474414810, 61.02352941176469869 ) ) ;
#10398 = CARTESIAN_POINT ( 'NONE',  ( 18.82590614458706924, 1.876518846661452411, 52.53023010607846288 ) ) ;
#10399 = CARTESIAN_POINT ( 'NONE',  ( -13.35685195715142193, -21.05109796036597913, 61.56000367517481919 ) ) ;
#10400 = FACE_OUTER_BOUND ( 'NONE', #28624, .T. ) ;
#10401 = CARTESIAN_POINT ( 'NONE',  ( -24.25940922233440489, -13.08205373389642823, 63.12704356492964308 ) ) ;
#10402 = EDGE_CURVE ( 'NONE', #566, #41338, #10272, .T. ) ;
#10403 = VERTEX_POINT ( 'NONE', #14073 ) ;
#10404 = ORIENTED_EDGE ( 'NONE', *, *, #27043, .F. ) ;
#10405 = CARTESIAN_POINT ( 'NONE',  ( -16.90447226888101895, -21.79033282223921830, 72.44926656220420114 ) ) ;
#10406 = CARTESIAN_POINT ( 'NONE',  ( -22.67409364490373491, -14.81069326838761135, 52.02966884056656482 ) ) ;
#10407 = VERTEX_POINT ( 'NONE', #47837 ) ;
#10409 = DIRECTION ( 'NONE',  ( -2.866981220435666553E-17, 1.000000000000000000, 1.190614954331866791E-16 ) ) ;
#10408 = CARTESIAN_POINT ( 'NONE',  ( -24.05923365589681140, -11.41972516488058176, 66.60869825954527812 ) ) ;
#10410 = CARTESIAN_POINT ( 'NONE',  ( -24.21255563026993940, -13.09477139695512449, 66.49173888256298426 ) ) ;
#10411 = CARTESIAN_POINT ( 'NONE',  ( -12.00790786851990610, -10.29148984397945377, 63.91425679989585973 ) ) ;
#10412 = CARTESIAN_POINT ( 'NONE',  ( -22.24723880939002996, -9.656319818818069223, 59.86604062818025795 ) ) ;
#10413 = B_SPLINE_CURVE_WITH_KNOTS ( 'NONE', 3,
 ( #45999, #4884, #27517, #31212, #35621, #38840, #42788, #12254, #15937, #1899 ),
 .UNSPECIFIED., .F., .F.,
 ( 4, 2, 2, 2, 4 ),
 ( 0.6272669072878207519, 0.7522669073073100510, 0.8772669073267994611, 1.002266907346288871, 1.127266907365778170 ),
 .UNSPECIFIED. ) ;
#10414 = FACE_OUTER_BOUND ( 'NONE', #39840, .T. ) ;
#10415 = FACE_BOUND ( 'NONE', #28422, .T. ) ;
#10416 = CARTESIAN_POINT ( 'NONE',  ( -24.82842054764507367, -13.98508042741895352, 73.22933195708579035 ) ) ;
#10417 = CARTESIAN_POINT ( 'NONE',  ( -10.42366004362047960, -14.81678656420000095, 74.81395567366212163 ) ) ;
#10418 = CARTESIAN_POINT ( 'NONE',  ( -12.23896285002386719, -13.98645721660588137, 50.77966884056655772 ) ) ;
#10419 = VERTEX_POINT ( 'NONE', #29368 ) ;
#10420 = CARTESIAN_POINT ( 'NONE',  ( -50.42609385541305755, -14.80920654474425291, 71.98235294117645822 ) ) ;
#10421 = CARTESIAN_POINT ( 'NONE',  ( -27.42409385541305511, -25.10920654474410441, 63.99999999999998579 ) ) ;
#10422 = EDGE_CURVE ( 'NONE', #22327, #39973, #8718, .T. ) ;
#10423 = CARTESIAN_POINT ( 'NONE',  ( -10.50429924535250414, -16.15944446069506668, 71.46222527016213633 ) ) ;
#10424 = CARTESIAN_POINT ( 'NONE',  ( -20.84178545912654457, -21.42902457554051310, 58.84486364983385442 ) ) ;
#10425 = CARTESIAN_POINT ( 'NONE',  ( -20.00946539473887142, -8.250368680643830999, 73.87096600125035195 ) ) ;
#10426 = B_SPLINE_CURVE_WITH_KNOTS ( 'NONE', 3,
 ( #27233, #4580, #34856, #38548, #1123, #46192, #15650, #20085, #45474, #42259 ),
 .UNSPECIFIED., .F., .F.,
 ( 4, 2, 2, 2, 4 ),
 ( 0.6272669072977097304, 0.7522669073147462138, 0.8772669073317826971, 1.002266907348819291, 1.127266907365855664 ),
 .UNSPECIFIED. ) ;
#10427 = CARTESIAN_POINT ( 'NONE',  ( -24.47066272824306665, -14.57993217219608972, 62.99824437345091610 ) ) ;
#10428 = ORIENTED_EDGE ( 'NONE', *, *, #2445, .T. ) ;
#10429 = ORIENTED_EDGE ( 'NONE', *, *, #46030, .T. ) ;
#10430 = CARTESIAN_POINT ( 'NONE',  ( -19.09284385541304019, -8.630756214087126565, 51.74842643355248129 ) ) ;
#10431 = VERTEX_POINT ( 'NONE', #21979 ) ;
#10432 = CARTESIAN_POINT ( 'NONE',  ( -16.26184114368905043, -7.855670183028919062, 60.20028478909662795 ) ) ;
#10433 = CARTESIAN_POINT ( 'NONE',  ( -11.77745829805909850, -9.948221969229217976, 67.68552175396945358 ) ) ;
#10434 = CARTESIAN_POINT ( 'NONE',  ( -27.30749335439299585, -15.43885699713180770, 53.49999999999995026 ) ) ;
#10435 = EDGE_CURVE ( 'NONE', #33004, #32745, #47246, .T. ) ;
#10436 = EDGE_CURVE ( 'NONE', #20304, #41932, #25200, .T. ) ;
#10437 = CARTESIAN_POINT ( 'NONE',  ( -15.59973365315860150, -7.586021664999528902, 70.71015599988244560 ) ) ;
#10438 = ORIENTED_EDGE ( 'NONE', *, *, #39533, .T. ) ;
#10439 = CARTESIAN_POINT ( 'NONE',  ( -21.10170628810619675, -20.76538187170625349, 65.81127219879576273 ) ) ;
#10440 = PLANE ( 'NONE',  #23360 ) ;
#10441 = ORIENTED_EDGE ( 'NONE', *, *, #23275, .T. ) ;
#10442 = CARTESIAN_POINT ( 'NONE',  ( -19.14414919534269899, -7.968427671776686871, 67.20072066290214252 ) ) ;
#10443 = CARTESIAN_POINT ( 'NONE',  ( -20.33034385541270339, -6.857644439845836715, 49.98602051094355403 ) ) ;
#10444 = VERTEX_POINT ( 'NONE', #6486 ) ;
#10445 = EDGE_CURVE ( 'NONE', #42966, #42781, #13724, .T. ) ;
#10446 = EDGE_CURVE ( 'NONE', #13430, #42667, #33850, .T. ) ;
#10447 = CARTESIAN_POINT ( 'NONE',  ( -17.83973810966541862, -7.370757045899419602, 60.18786608788675352 ) ) ;
#10448 = CARTESIAN_POINT ( 'NONE',  ( -45.55409385541305767, -14.20920654474410760, 69.94787228701220272 ) ) ;
#10449 = DIRECTION ( 'NONE',  ( 2.866981220435666553E-17, -1.000000000000000000, -1.190614954331866791E-16 ) ) ;
#10450 = EDGE_LOOP ( 'NONE', ( #6322, #21787, #46013, #38643, #36669 ) ) ;
#10451 = CARTESIAN_POINT ( 'NONE',  ( -20.18142963041198357, -7.888199563509442847, 73.91434887155375577 ) ) ;
#10452 = EDGE_CURVE ( 'NONE', #11801, #42866, #11592, .T. ) ;
#10453 = CARTESIAN_POINT ( 'NONE',  ( -23.32920216380910006, -18.57114719142387216, 72.87441430430278899 ) ) ;
#10454 =( BOUNDED_CURVE ( )  B_SPLINE_CURVE ( 3, ( #13450, #36101, #6572, #47451 ),
 .UNSPECIFIED., .F., .F. ) 
 B_SPLINE_CURVE_WITH_KNOTS ( ( 4, 4 ),
 ( 0.4074455897393662318, 0.5000000000000000000 ),
 .UNSPECIFIED. ) 
 CURVE ( )  GEOMETRIC_REPRESENTATION_ITEM ( )  RATIONAL_B_SPLINE_CURVE ( ( 0.6983129098260973944, 0.7760317562607075281, 0.8765941196520100620, 1.000000000000008882 ) ) 
 REPRESENTATION_ITEM ( '' )  );
#10455 = CARTESIAN_POINT ( 'NONE',  ( -15.49795884165273918, -21.59473877286356114, 68.78412844181838182 ) ) ;
#10456 = ORIENTED_EDGE ( 'NONE', *, *, #19969, .F. ) ;
#10457 = CARTESIAN_POINT ( 'NONE',  ( -20.00946503018472811, -8.250368534377352958, 73.72096600125085786 ) ) ;
#10458 = CARTESIAN_POINT ( 'NONE',  ( -10.74932326624039014, -12.70011325730971130, 60.81356021554577751 ) ) ;
#10459 = DIRECTION ( 'NONE',  ( 2.866981220435666553E-17, -1.000000000000000000, -1.190614954331866791E-16 ) ) ;
#10460 = CARTESIAN_POINT ( 'NONE',  ( -11.43058294688041165, -10.38410865082031442, 74.48239070398270201 ) ) ;
#10461 = ADVANCED_FACE ( 'NONE', ( #9934 ), #18019, .T. ) ;
#10462 = CARTESIAN_POINT ( 'NONE',  ( -16.09168231696496676, -7.478562553351938647, 60.31373090009974902 ) ) ;
#10463 = CYLINDRICAL_SURFACE ( 'NONE', #15859, 0.1499999999999991063 ) ;
#10464 = ORIENTED_EDGE ( 'NONE', *, *, #42731, .F. ) ;
#10465 = CYLINDRICAL_SURFACE ( 'NONE', #18982, 4.686499999999997002 ) ;
#10466 = FACE_OUTER_BOUND ( 'NONE', #20496, .T. ) ;
#10467 = CARTESIAN_POINT ( 'NONE',  ( -11.74181906717938695, -9.990828761398780955, 67.63863502377336090 ) ) ;
#10468 =( BOUNDED_SURFACE ( )  B_SPLINE_SURFACE ( 3, 1, ( 
 ( #32607, #47631 ),
 ( #13864, #28910 ),
 ( #26432, #22252 ),
 ( #3294, #36751 ),
 ( #45168, #25947 ),
 ( #33802, #14340 ),
 ( #22011, #6750 ) ),
 .UNSPECIFIED., .T., .F., .F. ) 
 B_SPLINE_SURFACE_WITH_KNOTS ( ( 4, 3, 4 ),
 ( 2, 2 ),
 ( 0.000000000000000000, 0.5000000000000000000, 1.000000000000000000 ),
 ( 0.000000000000000000, 1.000000000000000000 ),
 .UNSPECIFIED. ) 
 GEOMETRIC_REPRESENTATION_ITEM ( )  RATIONAL_B_SPLINE_SURFACE ( (
 ( 1.000000000000000000, 1.000000000000000000),
 ( 0.3333333333333335369, 0.3333333333333330373),
 ( 0.3333333333333335369, 0.3333333333333330373),
 ( 1.000000000000000000, 1.000000000000000000),
 ( 0.3333333333333333703, 0.3333333333333333703),
 ( 0.3333333333333333703, 0.3333333333333333703),
 ( 1.000000000000000000, 1.000000000000000000) ) ) 
 REPRESENTATION_ITEM ( '' )  SURFACE ( )  );
#10469 = ORIENTED_EDGE ( 'NONE', *, *, #8345, .F. ) ;
#10470 =( BOUNDED_CURVE ( )  B_SPLINE_CURVE ( 2, ( #26332, #33957, #4407, #7142, #23140, #3431, #14477, #38130, #4185 ),
 .UNSPECIFIED., .F., .F. ) 
 B_SPLINE_CURVE_WITH_KNOTS ( ( 3, 2, 2, 2, 3 ),
 ( 0.7500000000000000000, 0.7604166666666666297, 0.7708333333333334814, 0.7812500000000001110, 0.7916666666666667407 ),
 .UNSPECIFIED. ) 
 CURVE ( )  GEOMETRIC_REPRESENTATION_ITEM ( )  RATIONAL_B_SPLINE_CURVE ( ( 1.000000000000000000, 0.9238795325112867385, 1.000000000000000000, 0.9238795325112867385, 1.000000000000000000, 0.9238795325112867385, 1.000000000000000000, 0.9238795325112859613, 1.000000000000000888 ) ) 
 REPRESENTATION_ITEM ( '' )  );
#10471 = FACE_OUTER_BOUND ( 'NONE', #18278, .T. ) ;
#10472 = ORIENTED_EDGE ( 'NONE', *, *, #6592, .F. ) ;
#10473 = ORIENTED_EDGE ( 'NONE', *, *, #31968, .T. ) ;
#10474 = VERTEX_POINT ( 'NONE', #48313 ) ;
#10475 = AXIS2_PLACEMENT_3D ( 'NONE', #35786, #17063, #13372 ) ;
#10476 = DIRECTION ( 'NONE',  ( 1.000000000000000000, 2.866981220435666553E-17, 0.000000000000000000 ) ) ;
#10477 = CARTESIAN_POINT ( 'NONE',  ( -16.03800433270414061, -7.947685453143400913, 63.67010977152477835 ) ) ;
#10478 = CARTESIAN_POINT ( 'NONE',  ( -13.18362886651731358, -8.683667069837246899, 60.62445550483372614 ) ) ;
#10479 =( BOUNDED_SURFACE ( )  B_SPLINE_SURFACE ( 3, 1, ( 
 ( #12024, #34664 ),
 ( #23841, #15694 ),
 ( #37871, #34168 ),
 ( #46241, #19894 ),
 ( #30982, #15440 ),
 ( #20132, #34900 ),
 ( #27518, #8827 ) ),
 .UNSPECIFIED., .T., .F., .F. ) 
 B_SPLINE_SURFACE_WITH_KNOTS ( ( 4, 3, 4 ),
 ( 2, 2 ),
 ( 0.000000000000000000, 0.5000000000000000000, 1.000000000000000000 ),
 ( 0.000000000000000000, 1.000000000000000000 ),
 .UNSPECIFIED. ) 
 GEOMETRIC_REPRESENTATION_ITEM ( )  RATIONAL_B_SPLINE_SURFACE ( (
 ( 1.000000000000000000, 1.000000000000000000),
 ( 0.3333333333333335369, 0.3333333333333330373),
 ( 0.3333333333333335369, 0.3333333333333330373),
 ( 1.000000000000000000, 1.000000000000000000),
 ( 0.3333333333333333703, 0.3333333333333333703),
 ( 0.3333333333333333703, 0.3333333333333333703),
 ( 1.000000000000000000, 1.000000000000000000) ) ) 
 REPRESENTATION_ITEM ( '' )  SURFACE ( )  );
#10480 = ORIENTED_EDGE ( 'NONE', *, *, #48262, .T. ) ;
#10481 = ORIENTED_EDGE ( 'NONE', *, *, #36881, .T. ) ;
#10482 = CARTESIAN_POINT ( 'NONE',  ( -19.63034385650551883, -9.794322478646142471, 51.19202720610083901 ) ) ;
#10483 = CARTESIAN_POINT ( 'NONE',  ( -20.31649760022732565, -7.943510736669368910, 70.43595667626200907 ) ) ;
#10484 = DIRECTION ( 'NONE',  ( -0.8507615431891571989, 0.5255518971808581519, 6.876821558984484920E-08 ) ) ;
#10485 = EDGE_CURVE ( 'NONE', #34833, #38205, #24952, .T. ) ;
#10486 = CARTESIAN_POINT ( 'NONE',  ( -18.28034385650551741, -6.424090610841176385, 49.80797279389977916 ) ) ;
#10487 = ORIENTED_EDGE ( 'NONE', *, *, #27251, .F. ) ;
#10488 = EDGE_CURVE ( 'NONE', #39530, #45924, #43144, .T. ) ;
#10489 = FACE_OUTER_BOUND ( 'NONE', #28890, .T. ) ;
#10490 = CARTESIAN_POINT ( 'NONE',  ( -4.424093855413056886, -25.10920654474410441, 79.99999999999998579 ) ) ;
#10491 = CARTESIAN_POINT ( 'NONE',  ( -21.73662441638723308, -9.231682010981758779, 66.67622112302015580 ) ) ;
#10492 = EDGE_LOOP ( 'NONE', ( #35711, #683, #853, #6850, #23560 ) ) ;
#10493 = CARTESIAN_POINT ( 'NONE',  ( -23.96075626263749569, -17.45014286185010732, 66.24357239682277054 ) ) ;
#10494 = EDGE_LOOP ( 'NONE', ( #35247, #18373, #44585, #24044 ) ) ;
#10495 = EDGE_CURVE ( 'NONE', #7399, #46865, #7707, .T. ) ;
#10496 = CARTESIAN_POINT ( 'NONE',  ( -41.15852941833841783, -25.10920654474410441, 54.99999999999997868 ) ) ;
#10497 = CARTESIAN_POINT ( 'NONE',  ( -10.13106001268971212, -16.33070171280459704, 71.64024510068948359 ) ) ;
#10498 = CARTESIAN_POINT ( 'NONE',  ( -12.45873566688477929, -9.804017486950373339, 57.10407583662104258 ) ) ;
#10499 = ADVANCED_FACE ( 'NONE', ( #37960, #41911, #26169 ), #790, .F. ) ;
#10500 = EDGE_LOOP ( 'NONE', ( #37920, #45095 ) ) ;
#10501 = CARTESIAN_POINT ( 'NONE',  ( -22.83095840648717711, -19.93459376977450859, 72.82895984417613988 ) ) ;
#10502 = ADVANCED_FACE ( 'NONE', ( #33514 ), #17185, .T. ) ;
#10503 = CARTESIAN_POINT ( 'NONE',  ( -23.07906255732286738, -9.958937815627702861, 66.72677557046061736 ) ) ;
#10504 = CARTESIAN_POINT ( 'NONE',  ( -10.07803964209180414, -16.05037485348669435, 68.11734501381512530 ) ) ;
#10505 = ORIENTED_EDGE ( 'NONE', *, *, #17341, .F. ) ;
#10506 = DIRECTION ( 'NONE',  ( 0.9687793358424822143, -0.2479245821708672415, 0.000000000000000000 ) ) ;
#10507 = DIRECTION ( 'NONE',  ( 1.411223637948141806E-06, 4.279116285847032870E-06, 0.9999999999898486758 ) ) ;
#10508 = CARTESIAN_POINT ( 'NONE',  ( -10.39679176622870038, -14.24023819782134481, 64.40275955115841100 ) ) ;
#10509 = ORIENTED_EDGE ( 'NONE', *, *, #28020, .F. ) ;
#10510 = CARTESIAN_POINT ( 'NONE',  ( -11.78703052381813166, -10.65887729864124189, 74.43884969850331856 ) ) ;
#10511 = EDGE_LOOP ( 'NONE', ( #41011, #46638 ) ) ;
#10512 = CARTESIAN_POINT ( 'NONE',  ( -10.76802635004704989, -17.14192985119425572, 57.57271792098855201 ) ) ;
#10513 = CARTESIAN_POINT ( 'NONE',  ( -13.65248598864501339, -21.23405210337300630, 68.71271080785449215 ) ) ;
#10514 = CARTESIAN_POINT ( 'NONE',  ( -19.37484620200115160, -7.619050568204919216, 60.14588398245204814 ) ) ;
#10515 = APPLICATION_CONTEXT ( 'automotive_design' ) ;
#10516 = CARTESIAN_POINT ( 'NONE',  ( -23.42604898704557925, -18.50800750300421171, 72.76928057529130456 ) ) ;
#10517 = ORIENTED_EDGE ( 'NONE', *, *, #26898, .T. ) ;
#10518 = CARTESIAN_POINT ( 'NONE',  ( -40.92409385541305511, -14.80920654474410725, 74.99999999999998579 ) ) ;
#10519 = CARTESIAN_POINT ( 'NONE',  ( -11.42264205816738176, -11.09470156419723708, 64.29315101522172426 ) ) ;
#10520 = CARTESIAN_POINT ( 'NONE',  ( -24.34598896336966334, -16.14727844041069460, 62.89328645805750284 ) ) ;
#10521 = ORIENTED_EDGE ( 'NONE', *, *, #35107, .F. ) ;
#10522 = CARTESIAN_POINT ( 'NONE',  ( -9.979603264230430426, -14.52052340097724148, 68.04295441848455539 ) ) ;
#10523 = LINE ( 'NONE', #17411, #7041 ) ;
#10524 = VERTEX_POINT ( 'NONE', #41666 ) ;
#10525 = ORIENTED_EDGE ( 'NONE', *, *, #34781, .T. ) ;
#10526 = CARTESIAN_POINT ( 'NONE',  ( -15.03427660820159950, -21.44211488324610926, 65.12068745241758450 ) ) ;
#10527 = DIRECTION ( 'NONE',  ( 0.000000000000000000, 0.000000000000000000, 1.000000000000000000 ) ) ;
#10528 = DIRECTION ( 'NONE',  ( 0.3926557917762825145, -0.9196855055857631189, -5.808111619717074757E-09 ) ) ;
#10529 = CARTESIAN_POINT ( 'NONE',  ( -20.63243265594276110, -8.084608023805090582, 63.42466202532494890 ) ) ;
#10530 = CARTESIAN_POINT ( 'NONE',  ( -12.29927565234787679, -19.57981848576777040, 61.50751631702252098 ) ) ;
#10531 = CARTESIAN_POINT ( 'NONE',  ( -13.14999064602648637, -9.265557826385967033, 67.37942786034257381 ) ) ;
#10532 = FACE_OUTER_BOUND ( 'NONE', #26380, .T. ) ;
#10533 = ORIENTED_EDGE ( 'NONE', *, *, #10646, .F. ) ;
#10534 = ORIENTED_EDGE ( 'NONE', *, *, #2059, .F. ) ;
#10535 = FACE_OUTER_BOUND ( 'NONE', #19597, .T. ) ;
#10536 = VECTOR ( 'NONE', #46671, 1000.000000000000000 ) ;
#10537 = LINE ( 'NONE', #21853, #16548 ) ;
#10538 = DIRECTION ( 'NONE',  ( 0.7847243476406478013, 0.6198448985189423110, -4.433022207822421914E-08 ) ) ;
#10539 = CARTESIAN_POINT ( 'NONE',  ( -45.92409385541305511, -17.80920654474410370, 70.50000000000000000 ) ) ;
#10540 = CARTESIAN_POINT ( 'NONE',  ( -11.91343869374197695, -19.82283377674160718, 58.04186948019505365 ) ) ;
#10541 = ORIENTED_EDGE ( 'NONE', *, *, #12174, .T. ) ;
#10542 = EDGE_CURVE ( 'NONE', #20025, #45257, #43331, .T. ) ;
#10543 = CARTESIAN_POINT ( 'NONE',  ( -18.36159385650551812, -9.295667164867525756, 49.30633214617472504 ) ) ;
#10544 = VERTEX_POINT ( 'NONE', #34022 ) ;
#10545 = DIRECTION ( 'NONE',  ( -0.9687793358424817702, 0.2479245821708684905, 0.000000000000000000 ) ) ;
#10546 = CARTESIAN_POINT ( 'NONE',  ( -11.91343944425293522, -19.82283459374304968, 58.04187056893558605 ) ) ;
#10547 = DIRECTION ( 'NONE',  ( -0.7248509490090242480, 0.6889057277456162032, -1.880377065355346998E-09 ) ) ;
#10548 = LINE ( 'NONE', #40105, #18125 ) ;
#10549 = ORIENTED_EDGE ( 'NONE', *, *, #21275, .T. ) ;
#10550 = CARTESIAN_POINT ( 'NONE',  ( -50.42609385541305755, -14.90920654474417972, 64.04117647058822627 ) ) ;
#10551 = CARTESIAN_POINT ( 'NONE',  ( -14.60689809042303011, -8.346551666329650843, 64.08978840692947188 ) ) ;
#10552 = ADVANCED_FACE ( 'NONE', ( #44639 ), #44896, .F. ) ;
#10553 = VERTEX_POINT ( 'NONE', #18512 ) ;
#10554 = ADVANCED_FACE ( 'NONE', ( #22970 ), #34259, .T. ) ;
#10555 = CARTESIAN_POINT ( 'NONE',  ( -16.09245304043805191, -7.886071317471073705, 63.67011060592734140 ) ) ;
#10556 = EDGE_LOOP ( 'NONE', ( #28980, #9569, #47736, #40219 ) ) ;
#10557 = LINE ( 'NONE', #2441, #45653 ) ;
#10558 = VERTEX_POINT ( 'NONE', #22225 ) ;
#10559 = VECTOR ( 'NONE', #39959, 1000.000000000000000 ) ;
#10560 = DIRECTION ( 'NONE',  ( -0.000000000000000000, -1.000000000000000000, -0.000000000000000000 ) ) ;
#10561 = CARTESIAN_POINT ( 'NONE',  ( -21.67055903134415473, -17.89628178023893668, 52.02966884056656482 ) ) ;
#10562 = ADVANCED_FACE ( 'NONE', ( #15539 ), #8744, .T. ) ;
#10563 = ORIENTED_EDGE ( 'NONE', *, *, #42418, .T. ) ;
#10564 = DIRECTION ( 'NONE',  ( 0.003782665018460031406, 0.9999928456970870183, 9.532993539727310637E-09 ) ) ;
#10565 = AXIS2_PLACEMENT_3D ( 'NONE', #46739, #12511, #12983 ) ;
#10566 = CARTESIAN_POINT ( 'NONE',  ( -20.31063677401542833, -8.430306179186672466, 70.44027317730545690 ) ) ;
#10567 = ORIENTED_EDGE ( 'NONE', *, *, #41243, .F. ) ;
#10568 = CARTESIAN_POINT ( 'NONE',  ( -10.89280197141400919, -11.22507430941316642, 64.33377434530349603 ) ) ;
#10569 = EDGE_CURVE ( 'NONE', #43308, #22272, #18783, .T. ) ;
#10570 = CARTESIAN_POINT ( 'NONE',  ( -19.67760665824181388, -21.48965406232008490, 65.75014118398131302 ) ) ;
#10571 = CARTESIAN_POINT ( 'NONE',  ( -21.62445905946246327, -8.656051727655954764, 73.72411892793267896 ) ) ;
#10572 = ORIENTED_EDGE ( 'NONE', *, *, #46589, .T. ) ;
#10573 = DIRECTION ( 'NONE',  ( -3.071710424422018668E-17, 6.404604876783312462E-16, 1.000000000000000000 ) ) ;
#10574 = EDGE_CURVE ( 'NONE', #20146, #9962, #1633, .T. ) ;
#10575 = CARTESIAN_POINT ( 'NONE',  ( -12.02824346918037612, -10.34977652055329678, 67.79896853024506242 ) ) ;
#10576 = CYLINDRICAL_SURFACE ( 'NONE', #43577, 0.1500000000000011879 ) ;
#10577 = ORIENTED_EDGE ( 'NONE', *, *, #19807, .T. ) ;
#10578 = VERTEX_POINT ( 'NONE', #13719 ) ;
#10579 = CARTESIAN_POINT ( 'NONE',  ( -22.48964968825576705, -9.905448439006629968, 73.76689030015370463 ) ) ;
#10580 = CARTESIAN_POINT ( 'NONE',  ( -17.00708426123225436, -7.821638799215111071, 74.26018273346642218 ) ) ;
#10581 = CARTESIAN_POINT ( 'NONE',  ( -11.01197672498281044, -17.74032467813711733, 71.85246142747087106 ) ) ;
#10582 = CARTESIAN_POINT ( 'NONE',  ( -15.74909385759799108, -8.112991634885936776, 51.74999426922421719 ) ) ;
#10583 = CARTESIAN_POINT ( 'NONE',  ( -23.71751471349159601, -11.63122711669449316, 63.23746208799618529 ) ) ;
#10584 = CARTESIAN_POINT ( 'NONE',  ( -14.11063322135152909, -21.03236308526469855, 72.21135587486895702 ) ) ;
#10585 = CARTESIAN_POINT ( 'NONE',  ( -19.20962530548710845, -21.63318799521329083, 62.29503840543927851 ) ) ;
#10586 = FACE_OUTER_BOUND ( 'NONE', #29128, .T. ) ;
#10587 = VERTEX_POINT ( 'NONE', #17173 ) ;
#10588 = CARTESIAN_POINT ( 'NONE',  ( -11.75774095458083224, -19.00383931511212765, 71.68685884783835149 ) ) ;
#10589 = CARTESIAN_POINT ( 'NONE',  ( -18.28991377027465504, -21.80587894173146424, 68.81514722156398989 ) ) ;
#10590 =( BOUNDED_SURFACE ( )  B_SPLINE_SURFACE ( 3, 1, ( 
 ( #32435, #2141 ),
 ( #24325, #32196 ),
 ( #2388, #28502 ),
 ( #31944, #36106 ),
 ( #20632, #10275 ),
 ( #17635, #43527 ),
 ( #20864, #36351 ) ),
 .UNSPECIFIED., .T., .F., .F. ) 
 B_SPLINE_SURFACE_WITH_KNOTS ( ( 4, 3, 4 ),
 ( 2, 2 ),
 ( 0.000000000000000000, 0.5000000000000000000, 1.000000000000000000 ),
 ( 0.000000000000000000, 1.000000000000000000 ),
 .UNSPECIFIED. ) 
 GEOMETRIC_REPRESENTATION_ITEM ( )  RATIONAL_B_SPLINE_SURFACE ( (
 ( 1.000000000000000000, 1.000000000000000000),
 ( 0.3333333333333335369, 0.3333333333333330373),
 ( 0.3333333333333335369, 0.3333333333333330373),
 ( 1.000000000000000000, 1.000000000000000000),
 ( 0.3333333333333333703, 0.3333333333333333703),
 ( 0.3333333333333333703, 0.3333333333333333703),
 ( 1.000000000000000000, 1.000000000000000000) ) ) 
 REPRESENTATION_ITEM ( '' )  SURFACE ( )  );
#10591 = EDGE_CURVE ( 'NONE', #32748, #46547, #46990, .T. ) ;
#10592 = EDGE_LOOP ( 'NONE', ( #12859, #16556, #3731, #30021, #2834 ) ) ;
#10593 = AXIS2_PLACEMENT_3D ( 'NONE', #7084, #430, #6829 ) ;
#10594 = ORIENTED_EDGE ( 'NONE', *, *, #9086, .T. ) ;
#10595 = CARTESIAN_POINT ( 'NONE',  ( -20.58245214235086351, -8.562158453623027299, 59.91413264589528609 ) ) ;
#10596 = AXIS2_PLACEMENT_3D ( 'NONE', #40913, #25419, #22452 ) ;
#10597 = FACE_OUTER_BOUND ( 'NONE', #38196, .T. ) ;
#10598 = DIRECTION ( 'NONE',  ( 1.224646799147353207E-16, 1.000000000000000000, -1.912410701131276611E-32 ) ) ;
#10599 = CARTESIAN_POINT ( 'NONE',  ( -24.30112618867181240, -13.25578303422174997, 59.64795780745660636 ) ) ;
#10600 = EDGE_LOOP ( 'NONE', ( #47121, #29554 ) ) ;
#10601 = EDGE_CURVE ( 'NONE', #36615, #14276, #23179, .T. ) ;
#10602 =( BOUNDED_CURVE ( )  B_SPLINE_CURVE ( 3, ( #13899, #44708, #28942, #41237 ),
 .UNSPECIFIED., .F., .F. ) 
 B_SPLINE_CURVE_WITH_KNOTS ( ( 4, 4 ),
 ( 0.9074455897393655102, 1.000000000000000000 ),
 .UNSPECIFIED. ) 
 CURVE ( )  GEOMETRIC_REPRESENTATION_ITEM ( )  RATIONAL_B_SPLINE_CURVE ( ( 0.6983129098261073864, 0.7760317562607105257, 0.8765941196520080636, 1.000000000000000000 ) ) 
 REPRESENTATION_ITEM ( '' )  );
#10603 = CARTESIAN_POINT ( 'NONE',  ( -24.46896812518309972, -12.38541668854236200, 73.40258933594091673 ) ) ;
#10604 = CARTESIAN_POINT ( 'NONE',  ( -10.89280251029460622, -11.22507333849785027, 64.33377325762776877 ) ) ;
#10605 = EDGE_LOOP ( 'NONE', ( #46832, #40959 ) ) ;
#10606 = CARTESIAN_POINT ( 'NONE',  ( -10.12326195556307695, -13.32541703369907893, 74.86313051124790263 ) ) ;
#10607 = CARTESIAN_POINT ( 'NONE',  ( -24.47999924015074669, -14.97998867148549351, 62.85729180369179403 ) ) ;
#10608 = CARTESIAN_POINT ( 'NONE',  ( -12.27604185553471616, -19.62628656662749549, 58.21210303282668264 ) ) ;
#10609 = ORIENTED_EDGE ( 'NONE', *, *, #23132, .F. ) ;
#10610 = CARTESIAN_POINT ( 'NONE',  ( -24.11793993921729395, -12.76166543249827434, 70.07243002473258286 ) ) ;
#10611 = ORIENTED_EDGE ( 'NONE', *, *, #22229, .T. ) ;
#10612 = FACE_OUTER_BOUND ( 'NONE', #43722, .T. ) ;
#10613 = EDGE_CURVE ( 'NONE', #3341, #47047, #2063, .T. ) ;
#10614 = DIRECTION ( 'NONE',  ( -5.854827030937197869E-31, -1.020425574103664912E-16, -1.000000000000000000 ) ) ;
#10615 = ORIENTED_EDGE ( 'NONE', *, *, #37342, .F. ) ;
#10616 = CARTESIAN_POINT ( 'NONE',  ( -24.14992822999210276, -18.01341164000503525, 59.11882993461590274 ) ) ;
#10617 = CARTESIAN_POINT ( 'NONE',  ( -20.05203603265719892, -8.267149239628885482, 73.72656352965896076 ) ) ;
#10618 = DIRECTION ( 'NONE',  ( -1.487365705136564946E-06, 6.376425429333053644E-07, 0.9999999999986904919 ) ) ;
#10619 = EDGE_CURVE ( 'NONE', #32198, #29810, #34592, .T. ) ;
#10620 = CARTESIAN_POINT ( 'NONE',  ( -23.44980356754079054, -18.46889531339634871, 72.91368236442116313 ) ) ;
#10621 = ADVANCED_FACE ( 'NONE', ( #47241 ), #43055, .F. ) ;
#10622 = DIRECTION ( 'NONE',  ( 0.000000000000000000, 0.000000000000000000, 1.000000000000000000 ) ) ;
#10623 = CARTESIAN_POINT ( 'NONE',  ( -10.47299162366406478, -15.63514707757639854, 61.33789045486464886 ) ) ;
#10624 = LINE ( 'NONE', #14042, #40806 ) ;
#10625 = ORIENTED_EDGE ( 'NONE', *, *, #22164, .T. ) ;
#10626 = CARTESIAN_POINT ( 'NONE',  ( -12.17457826531766329, -10.10312750218776046, 64.03474096465798482 ) ) ;
#10627 = CARTESIAN_POINT ( 'NONE',  ( -9.990623107247818879, -14.31192343302863179, 64.57299167182827659 ) ) ;
#10628 = CARTESIAN_POINT ( 'NONE',  ( -46.29409385541305966, -12.76354662275040219, 71.04301729251712061 ) ) ;
#10629 = AXIS2_PLACEMENT_3D ( 'NONE', #37952, #34011, #37705 ) ;
#10630 = DIRECTION ( 'NONE',  ( 0.9687793358424821033, -0.2479245821708677133, 0.000000000000000000 ) ) ;
#10631 = CARTESIAN_POINT ( 'NONE',  ( -16.02453559203015132, -22.12732798260191913, 58.47240968810538675 ) ) ;
#10632 = CARTESIAN_POINT ( 'NONE',  ( -14.25534385650552238, -7.417179338643134834, 52.18511593390279302 ) ) ;
#10633 = AXIS2_PLACEMENT_3D ( 'NONE', #48728, #22633, #14467 ) ;
#10634 = ORIENTED_EDGE ( 'NONE', *, *, #30701, .T. ) ;
#10635 = ORIENTED_EDGE ( 'NONE', *, *, #27015, .T. ) ;
#10636 = CARTESIAN_POINT ( 'NONE',  ( -24.49635653881819408, -12.46679777644911447, 73.35730153580948354 ) ) ;
#10637 = CARTESIAN_POINT ( 'NONE',  ( -9.975182982828622258, -14.68140347846369131, 71.52793889455062981 ) ) ;
#10638 = EDGE_LOOP ( 'NONE', ( #11210, #2864, #34456, #43625, #3175 ) ) ;
#10639 = CARTESIAN_POINT ( 'NONE',  ( -17.42409385541299471, -14.80920654474434883, 62.02966884056656482 ) ) ;
#10640 = DIRECTION ( 'NONE',  ( 1.000000000000000000, 0.000000000000000000, 0.000000000000000000 ) ) ;
#10641 = CARTESIAN_POINT ( 'NONE',  ( -21.79028809537168243, -9.273590339475653366, 63.47681654923867711 ) ) ;
#10642 = CARTESIAN_POINT ( 'NONE',  ( -12.22456126456390280, -19.57467567670336450, 61.81167242413056329 ) ) ;
#10643 = ADVANCED_FACE ( 'NONE', ( #35889 ), #4696, .T. ) ;
#10644 = FACE_BOUND ( 'NONE', #46006, .T. ) ;
#10645 = CARTESIAN_POINT ( 'NONE',  ( -12.13854904415787850, -9.558901172912655397, 57.18961277425697176 ) ) ;
#10646 = EDGE_CURVE ( 'NONE', #8033, #25935, #13157, .T. ) ;
#10647 = DIRECTION ( 'NONE',  ( -1.424565728495322281E-06, 1.060674514755067221E-05, -0.9999999999427338082 ) ) ;
#10648 = CARTESIAN_POINT ( 'NONE',  ( -16.63927444439371683, -21.76668879618412333, 68.88487749788691872 ) ) ;
#10649 = EDGE_CURVE ( 'NONE', #13987, #46068, #36136, .T. ) ;
#10650 = EDGE_CURVE ( 'NONE', #30363, #24642, #14941, .T. ) ;
#10651 = EDGE_CURVE ( 'NONE', #24418, #12172, #48124, .T. ) ;
#10652 = EDGE_LOOP ( 'NONE', ( #21874, #7118 ) ) ;
#10653 = CARTESIAN_POINT ( 'NONE',  ( -13.95487512861695834, -17.97781459419518058, 49.52966884056656482 ) ) ;
#10654 = CARTESIAN_POINT ( 'NONE',  ( -10.59656512619885227, -13.05092609425065220, 68.02360230423869325 ) ) ;
#10655 = CARTESIAN_POINT ( 'NONE',  ( -15.46784385759799285, -9.357632978295836068, 49.97845033065684106 ) ) ;
#10656 = CARTESIAN_POINT ( 'NONE',  ( -13.65248598864501339, -21.23405210337300630, 68.71271080785449215 ) ) ;
#10657 = LINE ( 'NONE', #40218, #16523 ) ;
#10658 = VERTEX_POINT ( 'NONE', #17665 ) ;
#10659 = ORIENTED_EDGE ( 'NONE', *, *, #13550, .T. ) ;
#10660 = CARTESIAN_POINT ( 'NONE',  ( -15.88659385541304303, -7.222650657624104298, 49.61879703869476543 ) ) ;
#10661 = ORIENTED_EDGE ( 'NONE', *, *, #23329, .F. ) ;
#10662 = CARTESIAN_POINT ( 'NONE',  ( -17.38353765754063929, -7.359306650671737060, 67.12015974172000199 ) ) ;
#10663 = CARTESIAN_POINT ( 'NONE',  ( -18.97054410961560578, -7.521390078327941708, 67.08567059339527816 ) ) ;
#10664 = CIRCLE ( 'NONE', #26413, 0.5560000000000009379 ) ;
#10665 = CARTESIAN_POINT ( 'NONE',  ( -24.61980809523442559, -12.87874405397987232, 66.46393279139718402 ) ) ;
#10666 = ADVANCED_FACE ( 'NONE', ( #10771 ), #40807, .T. ) ;
#10667 = CARTESIAN_POINT ( 'NONE',  ( -16.26195973558533936, -21.76306465430365122, 58.57113428431811997 ) ) ;
#10668 = ORIENTED_EDGE ( 'NONE', *, *, #45501, .F. ) ;
#10669 = CARTESIAN_POINT ( 'NONE',  ( -13.53325528467554406, -21.16256411608339150, 65.17124155742401115 ) ) ;
#10670 = DIRECTION ( 'NONE',  ( -5.625773302382611900E-06, -7.100530147430143890E-06, -0.9999999999589666011 ) ) ;
#10671 = ORIENTED_EDGE ( 'NONE', *, *, #42354, .T. ) ;
#10672 = CARTESIAN_POINT ( 'NONE',  ( -11.48484495912356707, -11.01053355528029165, 57.21463035491839122 ) ) ;
#10673 = CARTESIAN_POINT ( 'NONE',  ( -12.32278866559117780, -19.67576434477648917, 61.41150688479135766 ) ) ;
#10674 = ORIENTED_EDGE ( 'NONE', *, *, #14060, .T. ) ;
#10675 = CARTESIAN_POINT ( 'NONE',  ( -19.57546054543010783, -21.94189796748987575, 62.03857704761023939 ) ) ;
#10676 = DIRECTION ( 'NONE',  ( -3.071710424422018052E-17, 6.404604876783311476E-16, 1.000000000000000000 ) ) ;
#10677 = ORIENTED_EDGE ( 'NONE', *, *, #47257, .T. ) ;
#10678 = CARTESIAN_POINT ( 'NONE',  ( -14.05371499411349845, -21.00138273984457982, 72.22607703579409133 ) ) ;
#10679 = CARTESIAN_POINT ( 'NONE',  ( -24.42668993457695592, -13.99045928592870958, 73.40799407547365263 ) ) ;
#10680 =( BOUNDED_SURFACE ( )  B_SPLINE_SURFACE ( 3, 1, ( 
 ( #35701, #31547 ),
 ( #13054, #9642 ),
 ( #16747, #46581 ),
 ( #12827, #13774 ),
 ( #9388, #1502 ),
 ( #27847, #39658 ),
 ( #28085, #35949 ) ),
 .UNSPECIFIED., .T., .F., .F. ) 
 B_SPLINE_SURFACE_WITH_KNOTS ( ( 4, 3, 4 ),
 ( 2, 2 ),
 ( 0.000000000000000000, 0.5000000000000000000, 1.000000000000000000 ),
 ( 0.000000000000000000, 1.000000000000000000 ),
 .UNSPECIFIED. ) 
 GEOMETRIC_REPRESENTATION_ITEM ( )  RATIONAL_B_SPLINE_SURFACE ( (
 ( 1.000000000000000000, 1.000000000000000000),
 ( 0.3333333333333335369, 0.3333333333333330373),
 ( 0.3333333333333335369, 0.3333333333333330373),
 ( 1.000000000000000000, 1.000000000000000000),
 ( 0.3333333333333333703, 0.3333333333333333703),
 ( 0.3333333333333333703, 0.3333333333333333703),
 ( 1.000000000000000000, 1.000000000000000000) ) ) 
 REPRESENTATION_ITEM ( '' )  SURFACE ( )  );
#10681 = DIRECTION ( 'NONE',  ( 0.9687793358424822143, -0.2479245821708672415, 0.000000000000000000 ) ) ;
#10682 = DIRECTION ( 'NONE',  ( -1.190035116827072985E-06, -1.172070119237067893E-06, -0.9999999999986051158 ) ) ;
#10683 = VERTEX_POINT ( 'NONE', #29736 ) ;
#10684 = FACE_OUTER_BOUND ( 'NONE', #31747, .T. ) ;
#10685 = FACE_OUTER_BOUND ( 'NONE', #37962, .T. ) ;
#10686 = CARTESIAN_POINT ( 'NONE',  ( -23.70015231925135168, -18.82353928378165975, 69.47867257277708575 ) ) ;
#10687 = CARTESIAN_POINT ( 'NONE',  ( -10.77549359890341485, -17.15424032507071317, 61.45743111002949632 ) ) ;
#10688 = ORIENTED_EDGE ( 'NONE', *, *, #1837, .F. ) ;
#10689 = CARTESIAN_POINT ( 'NONE',  ( -19.18086540149941399, -19.15397765319887569, 49.52966884056656482 ) ) ;
#10690 = CARTESIAN_POINT ( 'NONE',  ( -21.41863048803932656, -8.999699081277377388, 73.61600897546567523 ) ) ;
#10691 = ORIENTED_EDGE ( 'NONE', *, *, #26112, .T. ) ;
#10692 = DIRECTION ( 'NONE',  ( -0.000000000000000000, -0.000000000000000000, 1.000000000000000000 ) ) ;
#10693 = CARTESIAN_POINT ( 'NONE',  ( -21.43034385759798965, -6.857644439848012752, 49.98602051094139398 ) ) ;
#10694 = LINE ( 'NONE', #25474, #6245 ) ;
#10695 = VERTEX_POINT ( 'NONE', #2658 ) ;
#10696 = CARTESIAN_POINT ( 'NONE',  ( -17.68659385541293716, -7.222650657623975512, 49.61879703869464464 ) ) ;
#10697 = AXIS2_PLACEMENT_3D ( 'NONE', #34265, #8424, #12355 ) ;
#10698 = VERTEX_POINT ( 'NONE', #48196 ) ;
#10699 = EDGE_CURVE ( 'NONE', #37913, #14807, #25319, .T. ) ;
#10700 = ADVANCED_FACE ( 'NONE', ( #32690 ), #21620, .T. ) ;
#10701 = ORIENTED_EDGE ( 'NONE', *, *, #38960, .T. ) ;
#10702 = ORIENTED_EDGE ( 'NONE', *, *, #48245, .F. ) ;
#10703 = CARTESIAN_POINT ( 'NONE',  ( -19.48659385650551457, -9.302874398569244363, 51.68646062012417985 ) ) ;
#10704 = CARTESIAN_POINT ( 'NONE',  ( -50.42609385541305755, -14.90920654474424367, 70.07647058823528141 ) ) ;
#10705 = LINE ( 'NONE', #25722, #28313 ) ;
#10706 = CARTESIAN_POINT ( 'NONE',  ( -13.26948432366006969, -9.109728530933422164, 60.32461385657482822 ) ) ;
#10707 = ORIENTED_EDGE ( 'NONE', *, *, #17494, .F. ) ;
#10708 = ORIENTED_EDGE ( 'NONE', *, *, #46458, .T. ) ;
#10709 = EDGE_CURVE ( 'NONE', #19712, #31360, #18962, .T. ) ;
#10710 = ADVANCED_FACE ( 'NONE', ( #47714 ), #10301, .T. ) ;
#10711 = CARTESIAN_POINT ( 'NONE',  ( -15.07409385650551670, -9.792211528768504536, 50.49490371617623197 ) ) ;
#10712 = CARTESIAN_POINT ( 'NONE',  ( 18.54465614458695200, 0.6407533398237036382, 50.52649563099625851 ) ) ;
#10713 = CARTESIAN_POINT ( 'NONE',  ( 18.57590614458706924, 1.890747609047893185, 50.53028072113869484 ) ) ;
#10714 = CARTESIAN_POINT ( 'NONE',  ( -20.47409385650551528, -9.792211528768504536, 50.49490371617623197 ) ) ;
#10715 = ORIENTED_EDGE ( 'NONE', *, *, #36823, .F. ) ;
#10716 = EDGE_CURVE ( 'NONE', #28899, #15973, #25224, .T. ) ;
#10717 = CARTESIAN_POINT ( 'NONE',  ( -24.37613966482678762, -15.62716692544170094, 69.64193411296469094 ) ) ;
#10718 = CARTESIAN_POINT ( 'NONE',  ( -24.40836459905232303, -14.33371432994024808, 69.93658700684441953 ) ) ;
#10719 =( BOUNDED_CURVE ( )  B_SPLINE_CURVE ( 3, ( #18249, #13822, #32558, #28863 ),
 .UNSPECIFIED., .F., .F. ) 
 B_SPLINE_CURVE_WITH_KNOTS ( ( 4, 4 ),
 ( 0.000000000000000000, 0.4074455897393639559 ),
 .UNSPECIFIED. ) 
 CURVE ( )  GEOMETRIC_REPRESENTATION_ITEM ( )  RATIONAL_B_SPLINE_CURVE ( ( 1.000000000000000000, 0.4567392136813391845, 0.3561768502900329869, 0.6983129098260814072 ) ) 
 REPRESENTATION_ITEM ( '' )  );
#10720 = ORIENTED_EDGE ( 'NONE', *, *, #18036, .T. ) ;
#10721 = VECTOR ( 'NONE', #7108, 1000.000000000000000 ) ;
#10722 = VECTOR ( 'NONE', #19933, 1000.000000000000000 ) ;
#10723 = VERTEX_POINT ( 'NONE', #37101 ) ;
#10724 = CARTESIAN_POINT ( 'NONE',  ( -22.49805058420730219, -9.986866540729424813, 73.78161091687563555 ) ) ;
#10725 = CARTESIAN_POINT ( 'NONE',  ( -20.35208330028754631, -8.450993137587310855, 66.78104082230152017 ) ) ;
#10726 = DIRECTION ( 'NONE',  ( 0.000000000000000000, 0.000000000000000000, 1.000000000000000000 ) ) ;
#10727 = CARTESIAN_POINT ( 'NONE',  ( -12.84615363328625648, -20.17103110633857455, 72.09181604382622766 ) ) ;
#10728 = ORIENTED_EDGE ( 'NONE', *, *, #24352, .F. ) ;
#10729 = CARTESIAN_POINT ( 'NONE',  ( -19.05654430117847653, -8.000564469898289843, 67.08998960197388328 ) ) ;
#10730 = CARTESIAN_POINT ( 'NONE',  ( -15.39389095703113952, -21.97733419268598709, 72.23070866474378704 ) ) ;
#10731 = CARTESIAN_POINT ( 'NONE',  ( -19.38312129636155134, -7.621338365550096583, 60.06754680096511834 ) ) ;
#10732 = FACE_OUTER_BOUND ( 'NONE', #23094, .T. ) ;
#10733 = ORIENTED_EDGE ( 'NONE', *, *, #6613, .F. ) ;
#10734 = CARTESIAN_POINT ( 'NONE',  ( -45.92409385541306222, -14.38986189584960051, 70.50000000000000000 ) ) ;
#10735 = CARTESIAN_POINT ( 'NONE',  ( -10.70566866894273161, -16.94585410378973478, 57.98760548748136756 ) ) ;
#10736 =( BOUNDED_CURVE ( )  B_SPLINE_CURVE ( 3, ( #46003, #11297, #23349, #8104 ),
 .UNSPECIFIED., .F., .F. ) 
 B_SPLINE_CURVE_WITH_KNOTS ( ( 4, 4 ),
 ( 0.5000000000000000000, 0.9074455897393667314 ),
 .UNSPECIFIED. ) 
 CURVE ( )  GEOMETRIC_REPRESENTATION_ITEM ( )  RATIONAL_B_SPLINE_CURVE ( ( 1.000000000000009548, 0.4567392136813334669, 0.3561768502900239941, 0.6983129098260916212 ) ) 
 REPRESENTATION_ITEM ( '' )  );
#10737 = CARTESIAN_POINT ( 'NONE',  ( -21.68499601416157674, -9.192516039336663169, 66.66149992327366647 ) ) ;
#10738 = ORIENTED_EDGE ( 'NONE', *, *, #39278, .F. ) ;
#10739 = FACE_BOUND ( 'NONE', #9386, .T. ) ;
#10740 = ORIENTED_EDGE ( 'NONE', *, *, #38809, .F. ) ;
#10741 = CARTESIAN_POINT ( 'NONE',  ( -10.31413044408767554, -17.03453498993188475, 57.94406477676061229 ) ) ;
#10742 = CARTESIAN_POINT ( 'NONE',  ( -13.70953082315746130, -10.73489715249941057, 53.69233794759168887 ) ) ;
#10743 = CARTESIAN_POINT ( 'NONE',  ( -45.92409385541306222, -14.20920654474410760, 70.50000000000000000 ) ) ;
#10744 = CARTESIAN_POINT ( 'NONE',  ( -21.64297170217681554, -9.150934564753532285, 73.74561934610416358 ) ) ;
#10745 = ORIENTED_EDGE ( 'NONE', *, *, #11726, .T. ) ;
#10746 = CARTESIAN_POINT ( 'NONE',  ( -10.47191904619592684, -13.98145195064897095, 61.14651201797807545 ) ) ;
#10747 = VERTEX_POINT ( 'NONE', #17894 ) ;
#10748 = CARTESIAN_POINT ( 'NONE',  ( -11.22844613476422460, -11.44458948612160043, 64.43409918096024569 ) ) ;
#10749 = CARTESIAN_POINT ( 'NONE',  ( -23.37507359076485969, -18.49521754853151734, 69.36659925232392254 ) ) ;
#10750 = VERTEX_POINT ( 'NONE', #32920 ) ;
#10751 = CARTESIAN_POINT ( 'NONE',  ( -10.17289295492252599, -13.09960488110308319, 71.30804949251027836 ) ) ;
#10752 =( BOUNDED_CURVE ( )  B_SPLINE_CURVE ( 2, ( #8951, #31831, #46853, #13336, #46373, #43653, #35994, #24697, #27892 ),
 .UNSPECIFIED., .F., .F. ) 
 B_SPLINE_CURVE_WITH_KNOTS ( ( 3, 2, 2, 2, 3 ),
 ( 0.4166666666666667407, 0.4270833333333333703, 0.4375000000000000000, 0.4479166666666666852, 0.4583333333333333148 ),
 .UNSPECIFIED. ) 
 CURVE ( )  GEOMETRIC_REPRESENTATION_ITEM ( )  RATIONAL_B_SPLINE_CURVE ( ( 0.9999999999999995559, 0.9238795325112871826, 1.000000000000000000, 0.9238795325112867385, 1.000000000000000000, 0.9238795325112867385, 1.000000000000000000, 0.9238795325112867385, 1.000000000000000000 ) ) 
 REPRESENTATION_ITEM ( '' )  );
#10753 = DIRECTION ( 'NONE',  ( 3.549360974554993999E-17, -6.371834667797928663E-18, -1.000000000000000000 ) ) ;
#10754 = ADVANCED_FACE ( 'NONE', ( #22343 ), #48686, .T. ) ;
#10755 = ORIENTED_EDGE ( 'NONE', *, *, #42325, .T. ) ;
#10756 = ORIENTED_EDGE ( 'NONE', *, *, #42091, .F. ) ;
#10757 = DIRECTION ( 'NONE',  ( -0.1240347345892086200, 1.145860353393066553E-16, -0.9922778767136676281 ) ) ;
#10758 = CARTESIAN_POINT ( 'NONE',  ( -23.22228500509449134, -18.82597476736437869, 69.38552271346109990 ) ) ;
#10759 = CARTESIAN_POINT ( 'NONE',  ( -23.80338573481879294, -11.80731802715296297, 59.76763678108634537 ) ) ;
#10760 = CARTESIAN_POINT ( 'NONE',  ( -20.75775239920833215, -8.146595409969087598, 63.56767435313065562 ) ) ;
#10761 = CARTESIAN_POINT ( 'NONE',  ( -12.34924369011040923, -19.63124204235170112, 61.41295224250168872 ) ) ;
#10762 = CARTESIAN_POINT ( 'NONE',  ( -20.06838235508133650, -8.265300555148282768, 66.93671294127740623 ) ) ;
#10763 = AXIS2_PLACEMENT_3D ( 'NONE', #8143, #26114, #29809 ) ;
#10764 = AXIS2_PLACEMENT_3D ( 'NONE', #24367, #13499, #40753 ) ;
#10765 = VERTEX_POINT ( 'NONE', #41297 ) ;
#10766 = ORIENTED_EDGE ( 'NONE', *, *, #40833, .F. ) ;
#10767 = EDGE_CURVE ( 'NONE', #26011, #37558, #22980, .T. ) ;
#10768 = FACE_OUTER_BOUND ( 'NONE', #41206, .T. ) ;
#10769 = EDGE_CURVE ( 'NONE', #26221, #36791, #20524, .T. ) ;
#10770 = CARTESIAN_POINT ( 'NONE',  ( -19.86506860716628253, -8.248529813971950730, 73.79384751630072969 ) ) ;
#10771 = FACE_OUTER_BOUND ( 'NONE', #14285, .T. ) ;
#10772 = CARTESIAN_POINT ( 'NONE',  ( -11.03124136535102373, -17.66077402989073875, 71.56718193465405875 ) ) ;
#10773 = AXIS2_PLACEMENT_3D ( 'NONE', #40545, #41049, #2875 ) ;
#10774 = CARTESIAN_POINT ( 'NONE',  ( -30.42409385541305156, -6.859206544744110623, 47.99999999999997868 ) ) ;
#10775 = EDGE_CURVE ( 'NONE', #28733, #48574, #28497, .T. ) ;
#10776 = ORIENTED_EDGE ( 'NONE', *, *, #32893, .F. ) ;
#10777 = CARTESIAN_POINT ( 'NONE',  ( -19.09284385650552096, -7.406986770994973490, 48.81910596585309747 ) ) ;
#10778 = EDGE_LOOP ( 'NONE', ( #10325, #20329, #47416, #33601, #25376 ) ) ;
#10779 = CARTESIAN_POINT ( 'NONE',  ( -21.94683311842353746, -20.15404798103656958, 62.42366210617201006 ) ) ;
#10780 = ADVANCED_FACE ( 'NONE', ( #34382 ), #19137, .T. ) ;
#10781 = CARTESIAN_POINT ( 'NONE',  ( -13.19031587015885343, -9.064346445990929979, 49.69364538247001661 ) ) ;
#10782 = CARTESIAN_POINT ( 'NONE',  ( -13.17078218117215549, -9.186392337449538203, 67.39414915108072535 ) ) ;
#10783 = EDGE_LOOP ( 'NONE', ( #47186, #2513, #25542, #47138 ) ) ;
#10784 = CARTESIAN_POINT ( 'NONE',  ( -10.48067290732983281, -16.03043740265091444, 67.97767830707738312 ) ) ;
#10785 = CARTESIAN_POINT ( 'NONE',  ( -14.73514675383382055, -8.346202503743331391, 60.60530971328631722 ) ) ;
#10786 = ORIENTED_EDGE ( 'NONE', *, *, #17968, .F. ) ;
#10787 = CARTESIAN_POINT ( 'NONE',  ( -15.15105612103415034, -21.43000825703723322, 65.10596678909395507 ) ) ;
#10788 = B_SPLINE_CURVE_WITH_KNOTS ( 'NONE', 3,
 ( #12209, #42013, #24034, #38289, #24272, #27950, #27712, #42979, #16120, #27230 ),
 .UNSPECIFIED., .F., .F.,
 ( 4, 2, 2, 2, 4 ),
 ( 0.000000000000000000, 0.2500000000000000000, 0.5000000000000000000, 0.7500000000000000000, 1.000000000000000000 ),
 .UNSPECIFIED. ) ;
#10789 = CARTESIAN_POINT ( 'NONE',  ( -10.49796979654650642, -16.16706115165171198, 64.66338504953419886 ) ) ;
#10790 = ORIENTED_EDGE ( 'NONE', *, *, #23986, .T. ) ;
#10791 = CARTESIAN_POINT ( 'NONE',  ( -11.18189875852979043, -11.63857375077518519, 71.16031116833757153 ) ) ;
#10792 = VECTOR ( 'NONE', #31789, 1000.000000000000000 ) ;
#10793 = VECTOR ( 'NONE', #20372, 1000.000000000000000 ) ;
#10794 = ORIENTED_EDGE ( 'NONE', *, *, #22788, .T. ) ;
#10795 = DIRECTION ( 'NONE',  ( 0.2771212459065066636, -0.9608349572466771127, -4.100231986695786665E-08 ) ) ;
#10796 = CARTESIAN_POINT ( 'NONE',  ( -24.87322977116181022, -14.68525938325893065, 62.87442968679287958 ) ) ;
#10797 = VERTEX_POINT ( 'NONE', #34872 ) ;
#10798 = CARTESIAN_POINT ( 'NONE',  ( -12.79154865046270473, -8.973695691655201756, 67.49287406301634462 ) ) ;
#10799 = CARTESIAN_POINT ( 'NONE',  ( -11.45924070651598470, -10.34566349473087854, 74.53910820911023905 ) ) ;
#10800 = ORIENTED_EDGE ( 'NONE', *, *, #34879, .T. ) ;
#10801 = CYLINDRICAL_SURFACE ( 'NONE', #33083, 0.1500000000000081268 ) ;
#10802 = AXIS2_PLACEMENT_3D ( 'NONE', #12072, #46047, #12303 ) ;
#10803 = EDGE_CURVE ( 'NONE', #32331, #36313, #29152, .T. ) ;
#10804 = CARTESIAN_POINT ( 'NONE',  ( -11.07113446568633108, -18.70063274991032998, 61.38436695725324199 ) ) ;
#10805 = CARTESIAN_POINT ( 'NONE',  ( -23.59327504554355315, -11.39630409041826198, 69.90682860766239060 ) ) ;
#10806 = ORIENTED_EDGE ( 'NONE', *, *, #33872, .F. ) ;
#10807 = CARTESIAN_POINT ( 'NONE',  ( -19.89714791213391365, -21.83689362560225788, 69.05765572360830618 ) ) ;
#10808 = B_SPLINE_CURVE_WITH_KNOTS ( 'NONE', 3,
 ( #27856, #36201, #35712, #16990, #42886, #32519, #39666, #28821, #9650, #9396 ),
 .UNSPECIFIED., .F., .F.,
 ( 4, 2, 2, 2, 4 ),
 ( 0.000000000000000000, 0.2500000000000000000, 0.5000000000000000000, 0.7500000000000000000, 1.000000000000000000 ),
 .UNSPECIFIED. ) ;
#10809 = CARTESIAN_POINT ( 'NONE',  ( -11.71918404020638427, -18.95175453447548009, 71.70158022526054253 ) ) ;
#10810 = EDGE_CURVE ( 'NONE', #21395, #27235, #38416, .T. ) ;
#10811 = ORIENTED_EDGE ( 'NONE', *, *, #45081, .F. ) ;
#10812 = ORIENTED_EDGE ( 'NONE', *, *, #35252, .F. ) ;
#10813 = CARTESIAN_POINT ( 'NONE',  ( -22.75144419618436586, -9.600271701911582412, 73.59505825258622735 ) ) ;
#10814 = CARTESIAN_POINT ( 'NONE',  ( -22.96481576609224717, -19.16891988936071556, 58.89882756593014790 ) ) ;
#10815 = FACE_OUTER_BOUND ( 'NONE', #24904, .T. ) ;
#10816 = CARTESIAN_POINT ( 'NONE',  ( -14.96159385759799143, -7.228003583438117552, 51.38655588711986155 ) ) ;
#10817 = CARTESIAN_POINT ( 'NONE',  ( -24.50530043060364349, -7.885727737951715888, 53.49999999999995026 ) ) ;
#10818 = CARTESIAN_POINT ( 'NONE',  ( -16.92358529718788063, -21.79135155313683114, 68.92233962256314328 ) ) ;
#10819 = CARTESIAN_POINT ( 'NONE',  ( -24.34502386579654498, -17.56683345968398768, 66.12852568699506151 ) ) ;
#10820 = CARTESIAN_POINT ( 'NONE',  ( -16.55143150278462016, -22.20792881918157491, 65.42553161510207360 ) ) ;
#10821 = ORIENTED_EDGE ( 'NONE', *, *, #25838, .T. ) ;
#10822 = CARTESIAN_POINT ( 'NONE',  ( -17.42409385541300182, -14.80920654474440745, 53.27966884056655061 ) ) ;
#10823 = LINE ( 'NONE', #44825, #12481 ) ;
#10824 = ADVANCED_FACE ( 'NONE', ( #34144 ), #45974, .T. ) ;
#10825 = CARTESIAN_POINT ( 'NONE',  ( -13.92409385541305511, -10.10920654474410618, 81.49999999999998579 ) ) ;
#10826 = DIRECTION ( 'NONE',  ( 0.9687793358424821033, -0.2479245821708679909, 0.000000000000000000 ) ) ;
#10827 = ADVANCED_FACE ( 'NONE', ( #11504 ), #8800, .T. ) ;
#10828 = B_SPLINE_CURVE_WITH_KNOTS ( 'NONE', 3,
 ( #38278, #1112, #16111, #38785, #8276, #31152, #5067, #46181, #1344, #23056 ),
 .UNSPECIFIED., .F., .F.,
 ( 4, 2, 2, 2, 4 ),
 ( 0.6272669072782223187, 0.7522669073001169160, 0.8772669073220116243, 1.002266907343906333, 1.127266907365800819 ),
 .UNSPECIFIED. ) ;
#10829 = PRESENTATION_LAYER_ASSIGNMENT (  '', '', ( #43859 ) ) ;
#10830 = ORIENTED_EDGE ( 'NONE', *, *, #10210, .F. ) ;
#10831 = AXIS2_PLACEMENT_3D ( 'NONE', #43583, #10564, #32256 ) ;
#10832 = ADVANCED_FACE ( 'NONE', ( #15670 ), #33910, .T. ) ;
#10833 = ORIENTED_EDGE ( 'NONE', *, *, #27009, .T. ) ;
#10834 = CARTESIAN_POINT ( 'NONE',  ( -27.42409385541305156, -25.10920654474410441, 74.99999999999998579 ) ) ;
#10835 = LINE ( 'NONE', #45319, #20560 ) ;
#10836 = AXIS2_PLACEMENT_3D ( 'NONE', #32942, #37369, #18663 ) ;
#10837 = ADVANCED_FACE ( 'NONE', ( #12233 ), #12468, .T. ) ;
#10838 = ORIENTED_EDGE ( 'NONE', *, *, #9026, .T. ) ;
#10839 = VECTOR ( 'NONE', #4458, 1000.000000000000000 ) ;
#10840 = CARTESIAN_POINT ( 'NONE',  ( -24.48100519043057233, -12.42118325661428457, 73.34201943126451795 ) ) ;
#10841 = CARTESIAN_POINT ( 'NONE',  ( -22.97409385650551528, -9.792211528768504536, 50.49490371617623197 ) ) ;
#10842 = EDGE_LOOP ( 'NONE', ( #6362, #32328, #22768 ) ) ;
#10843 = CARTESIAN_POINT ( 'NONE',  ( -24.25486363958986757, -13.06355980472538469, 63.11792038370487035 ) ) ;
#10844 = DIRECTION ( 'NONE',  ( 0.000000000000000000, 1.000000000000000000, -0.000000000000000000 ) ) ;
#10845 = CARTESIAN_POINT ( 'NONE',  ( -24.76540239943457422, -16.07765717072269140, 66.17829646510101327 ) ) ;
#10846 = ORIENTED_EDGE ( 'NONE', *, *, #36443, .F. ) ;
#10847 = CARTESIAN_POINT ( 'NONE',  ( -24.16181628213775312, -12.90510636975119674, 69.88316126822323326 ) ) ;
#10848 = ORIENTED_EDGE ( 'NONE', *, *, #4240, .T. ) ;
#10849 = DIRECTION ( 'NONE',  ( 6.919810409924334203E-06, 1.067025349499717229E-05, -0.9999999999191309108 ) ) ;
#10850 = CARTESIAN_POINT ( 'NONE',  ( -21.18000425931230168, -20.77541442555289919, 69.20450184740300870 ) ) ;
#10851 = ORIENTED_EDGE ( 'NONE', *, *, #19794, .F. ) ;
#10852 = CARTESIAN_POINT ( 'NONE',  ( -16.23831082583558327, -7.859603177651183437, 60.50028451141000119 ) ) ;
#10853 = CARTESIAN_POINT ( 'NONE',  ( -20.00946503018472811, -8.250368534377352958, 73.72096600125085786 ) ) ;
#10854 = CARTESIAN_POINT ( 'NONE',  ( -20.92409385650551812, -6.426201560718813433, 50.50509628382439331 ) ) ;
#10855 = VECTOR ( 'NONE', #17574, 1000.000000000000000 ) ;
#10856 = DIRECTION ( 'NONE',  ( -3.071710424422018668E-17, 6.404604876783312462E-16, 1.000000000000000000 ) ) ;
#10857 = VECTOR ( 'NONE', #3802, 1000.000000000000000 ) ;
#10858 = EDGE_CURVE ( 'NONE', #11228, #19229, #8528, .T. ) ;
#10859 = CARTESIAN_POINT ( 'NONE',  ( -23.91010245674826251, -17.57297063409389537, 62.75888927877479517 ) ) ;
#10860 = CYLINDRICAL_SURFACE ( 'NONE', #35521, 0.1500000000000042966 ) ;
#10861 = CARTESIAN_POINT ( 'NONE',  ( -15.68503146357154776, -7.977064754671971514, 70.75989839959960648 ) ) ;
#10862 = VERTEX_POINT ( 'NONE', #38569 ) ;
#10863 = CARTESIAN_POINT ( 'NONE',  ( -12.23301264461619553, -10.03852782535897958, 60.84446034103241630 ) ) ;
#10864 = AXIS2_PLACEMENT_3D ( 'NONE', #39213, #36465, #47575 ) ;
#10865 = VECTOR ( 'NONE', #19594, 1000.000000000000114 ) ;
#10866 = CARTESIAN_POINT ( 'NONE',  ( -9.985622318910028383, -14.38165043598653980, 64.50148546807987771 ) ) ;
#10867 = CARTESIAN_POINT ( 'NONE',  ( -22.95648371662476350, -9.819685991319531126, 70.11154895885017879 ) ) ;
#10868 = DIRECTION ( 'NONE',  ( 8.226841968992228303E-06, -2.386003345919280055E-06, -0.9999999999633130132 ) ) ;
#10869 = CARTESIAN_POINT ( 'NONE',  ( -10.81476112650719479, -12.49952415756758661, 60.87023803673543654 ) ) ;
#10870 = CARTESIAN_POINT ( 'NONE',  ( -22.80551657591753312, -9.657165430906786696, 73.58822797253898784 ) ) ;
#10871 = ORIENTED_EDGE ( 'NONE', *, *, #6521, .F. ) ;
#10872 = ORIENTED_EDGE ( 'NONE', *, *, #15998, .T. ) ;
#10873 = CARTESIAN_POINT ( 'NONE',  ( -11.53435529947139315, -18.68938829637487942, 61.16221976381599745 ) ) ;
#10874 = CARTESIAN_POINT ( 'NONE',  ( -17.85728874018076340, -21.84618329174708151, 61.89007996730683203 ) ) ;
#10875 = ORIENTED_EDGE ( 'NONE', *, *, #25648, .F. ) ;
#10877 = CARTESIAN_POINT ( 'NONE',  ( -13.72409385650551528, -6.426201560718813433, 50.50509628382439331 ) ) ;
#10876 = CARTESIAN_POINT ( 'NONE',  ( -15.34293294794334628, -7.655665426595480660, 74.25702532252046240 ) ) ;
#10878 = CARTESIAN_POINT ( 'NONE',  ( -17.42409385541300892, -14.80920654474439679, 47.99999999999994316 ) ) ;
#10879 = AXIS2_PLACEMENT_3D ( 'NONE', #11358, #45345, #4223 ) ;
#10880 = CARTESIAN_POINT ( 'NONE',  ( -20.68825345639836044, -8.112218880830354806, 63.48838406824151548 ) ) ;
#10881 = CARTESIAN_POINT ( 'NONE',  ( -22.27817835350360909, -9.157512823226451104, 59.83675901011532261 ) ) ;
#10882 =( BOUNDED_CURVE ( )  B_SPLINE_CURVE ( 3, ( #13632, #10211, #13143, #5555 ),
 .UNSPECIFIED., .F., .F. ) 
 B_SPLINE_CURVE_WITH_KNOTS ( ( 4, 4 ),
 ( 0.5000000000000000000, 0.9074455897393624015 ),
 .UNSPECIFIED. ) 
 CURVE ( )  GEOMETRIC_REPRESENTATION_ITEM ( )  RATIONAL_B_SPLINE_CURVE ( ( 0.9999999999999924505, 0.4567392136813328563, 0.3561768502900357625, 0.6983129098260931755 ) ) 
 REPRESENTATION_ITEM ( '' )  );
#10883 = CARTESIAN_POINT ( 'NONE',  ( -11.32469277870022850, -18.34471304272907588, 58.10714594244494435 ) ) ;
#10884 = CARTESIAN_POINT ( 'NONE',  ( -24.83280391540558796, -14.02581302221999593, 73.22297261464329665 ) ) ;
#10885 = FACE_OUTER_BOUND ( 'NONE', #27296, .T. ) ;
#10886 = DIRECTION ( 'NONE',  ( -3.071710424422018668E-17, 6.404604876783312462E-16, 1.000000000000000000 ) ) ;
#10887 = ORIENTED_EDGE ( 'NONE', *, *, #12933, .T. ) ;
#10888 = DIRECTION ( 'NONE',  ( 0.5652317888644005084, 0.8249321334856241084, -7.911723905263142424E-08 ) ) ;
#10889 = CARTESIAN_POINT ( 'NONE',  ( -10.23610939720467528, -12.85046776639672039, 67.85337053980535416 ) ) ;
#10890 = EDGE_CURVE ( 'NONE', #26171, #15132, #41800, .T. ) ;
#10891 = CARTESIAN_POINT ( 'NONE',  ( -15.03781870946894905, -19.77948485407324242, 53.88362224778186516 ) ) ;
#10892 = CARTESIAN_POINT ( 'NONE',  ( -20.86784385759799321, -9.357632978295832515, 49.97845033065684106 ) ) ;
#10893 = CARTESIAN_POINT ( 'NONE',  ( -10.71854902139521926, -11.56295204017805567, 71.23860870132143930 ) ) ;
#10894 = CARTESIAN_POINT ( 'NONE',  ( -13.59065431704403615, -21.19813492939682220, 68.64280514999626348 ) ) ;
#10895 = B_SPLINE_CURVE_WITH_KNOTS ( 'NONE', 3,
 ( #17132, #32188, #21818, #32427, #40056, #21101, #21587, #2622, #28726, #25037 ),
 .UNSPECIFIED., .F., .F.,
 ( 4, 2, 2, 2, 4 ),
 ( 0.000000000000000000, 0.2500000000000000000, 0.5000000000000000000, 0.7500000000000000000, 1.000000000000000000 ),
 .UNSPECIFIED. ) ;
#10896 = CARTESIAN_POINT ( 'NONE',  ( -23.75068382698706770, -10.87373689121910658, 73.47537926597675551 ) ) ;
#10897 =( BOUNDED_SURFACE ( )  B_SPLINE_SURFACE ( 3, 1, ( 
 ( #24580, #12977 ),
 ( #8581, #4635 ),
 ( #1416, #24084 ),
 ( #28259, #5130 ),
 ( #42312, #23604 ),
 ( #35630, #9309 ),
 ( #35393, #4892 ) ),
 .UNSPECIFIED., .T., .F., .F. ) 
 B_SPLINE_SURFACE_WITH_KNOTS ( ( 4, 3, 4 ),
 ( 2, 2 ),
 ( 0.000000000000000000, 0.5000000000000000000, 1.000000000000000000 ),
 ( 0.000000000000000000, 1.000000000000000000 ),
 .UNSPECIFIED. ) 
 GEOMETRIC_REPRESENTATION_ITEM ( )  RATIONAL_B_SPLINE_SURFACE ( (
 ( 1.000000000000000000, 1.000000000000000000),
 ( 0.3333333333333335369, 0.3333333333333330373),
 ( 0.3333333333333335369, 0.3333333333333330373),
 ( 1.000000000000000000, 1.000000000000000000),
 ( 0.3333333333333333703, 0.3333333333333333703),
 ( 0.3333333333333333703, 0.3333333333333333703),
 ( 1.000000000000000000, 1.000000000000000000) ) ) 
 REPRESENTATION_ITEM ( '' )  SURFACE ( )  );
#10898 = ORIENTED_EDGE ( 'NONE', *, *, #33515, .T. ) ;
#10899 = VERTEX_POINT ( 'NONE', #38082 ) ;
#10900 = CARTESIAN_POINT ( 'NONE',  ( -13.91784385541304303, -6.860780111191487229, 51.02154966934377711 ) ) ;
#10901 = ADVANCED_FACE ( 'NONE', ( #27013 ), #4362, .F. ) ;
#10902 = VERTEX_POINT ( 'NONE', #30723 ) ;
#10903 = CARTESIAN_POINT ( 'NONE',  ( -16.28536801364495545, -7.851737743193615948, 60.20028506676293034 ) ) ;
#10904 = VECTOR ( 'NONE', #6634, 1000.000000000000114 ) ;
#10905 = CARTESIAN_POINT ( 'NONE',  ( -18.24684318355141599, -9.624075539355217757, 52.02966884056656482 ) ) ;
#10906 = EDGE_CURVE ( 'NONE', #1509, #18890, #11088, .T. ) ;
#10907 = VECTOR ( 'NONE', #37954, 1000.000000000000000 ) ;
#10908 = AXIS2_PLACEMENT_3D ( 'NONE', #42449, #46630, #30647 ) ;
#10909 = AXIS2_PLACEMENT_3D ( 'NONE', #23483, #8223, #23008 ) ;
#10910 = LINE ( 'NONE', #25446, #47337 ) ;
#10911 = DIRECTION ( 'NONE',  ( 0.8244078399817417191, 0.5659962132175737626, 7.627400655798535667E-08 ) ) ;
#10912 = VERTEX_POINT ( 'NONE', #23320 ) ;
#10913 = CARTESIAN_POINT ( 'NONE',  ( -24.36490009086193353, -15.72991820881333069, 73.11376895235396489 ) ) ;
#10914 = CARTESIAN_POINT ( 'NONE',  ( -21.06494968540953749, -21.30903997076690359, 62.15825466738357363 ) ) ;
#10915 = ORIENTED_EDGE ( 'NONE', *, *, #15031, .T. ) ;
#10916 = CARTESIAN_POINT ( 'NONE',  ( -10.37382936219775154, -14.83089353207902228, 74.81251018390588570 ) ) ;
#10917 = EDGE_CURVE ( 'NONE', #31867, #7245, #4604, .T. ) ;
#10918 = CARTESIAN_POINT ( 'NONE',  ( -17.42409385541299471, -14.80920654474435771, 49.52966884056655772 ) ) ;
#10919 = ADVANCED_FACE ( 'NONE', ( #27735 ), #5096, .T. ) ;
#10920 = ORIENTED_EDGE ( 'NONE', *, *, #27935, .T. ) ;
#10921 = CARTESIAN_POINT ( 'NONE',  ( -19.49109506855409180, -21.54969648977046148, 62.28031529404344013 ) ) ;
#10922 = CARTESIAN_POINT ( 'NONE',  ( -27.43465133269545930, -13.44290337829342796, 54.49999999999995026 ) ) ;
#10923 = CARTESIAN_POINT ( 'NONE',  ( -12.94070927391775427, -9.363776855876855265, 67.58762549400667297 ) ) ;
#10924 = EDGE_CURVE ( 'NONE', #20147, #3341, #46700, .T. ) ;
#10925 = EDGE_LOOP ( 'NONE', ( #16243, #5207 ) ) ;
#10926 = CARTESIAN_POINT ( 'NONE',  ( -11.97152748846423265, -19.88606886789912664, 58.08715752149842615 ) ) ;
#10927 = FACE_OUTER_BOUND ( 'NONE', #39345, .T. ) ;
#10928 = DIRECTION ( 'NONE',  ( -3.071710424422018668E-17, 6.404604876783312462E-16, 1.000000000000000000 ) ) ;
#10929 = CARTESIAN_POINT ( 'NONE',  ( -10.98611580423108336, -17.68970554115635352, 67.98233349607527032 ) ) ;
#10930 = ORIENTED_EDGE ( 'NONE', *, *, #17229, .F. ) ;
#10931 = DIRECTION ( 'NONE',  ( -3.071710424422018668E-17, 6.404604876783312462E-16, 1.000000000000000000 ) ) ;
#10932 = DIRECTION ( 'NONE',  ( 2.231660450020913765E-16, 0.9999954153791275058, 0.003028072113822189229 ) ) ;
#10933 = LINE ( 'NONE', #25953, #43584 ) ;
#10934 = CARTESIAN_POINT ( 'NONE',  ( -17.95973986510568920, -21.78880545038086680, 62.17535914954028442 ) ) ;
#10935 = CARTESIAN_POINT ( 'NONE',  ( -20.27409385650551599, -9.792211528768504536, 50.49490371617623197 ) ) ;
#10936 = EDGE_LOOP ( 'NONE', ( #30584, #21715, #25413, #6791, #45309 ) ) ;
#10937 = AXIS2_PLACEMENT_3D ( 'NONE', #23608, #47218, #28507 ) ;
#10938 = CARTESIAN_POINT ( 'NONE',  ( -17.75494382041872399, -22.25186532844304921, 58.60542163939332738 ) ) ;
#10939 = CARTESIAN_POINT ( 'NONE',  ( -21.03659385759798894, -8.995762431863214559, 51.38120296130585274 ) ) ;
#10940 = ORIENTED_EDGE ( 'NONE', *, *, #20553, .T. ) ;
#10941 = CARTESIAN_POINT ( 'NONE',  ( -22.33376602745314798, -19.86903051493498040, 69.18890041286789483 ) ) ;
#10942 =( GEOMETRIC_REPRESENTATION_CONTEXT ( 3 ) GLOBAL_UNCERTAINTY_ASSIGNED_CONTEXT ( ( #46008 ) ) GLOBAL_UNIT_ASSIGNED_CONTEXT ( ( #31734, #46525, #1696 ) ) REPRESENTATION_CONTEXT ( 'NONE', 'WORKASPACE' ) );
#10943 = CARTESIAN_POINT ( 'NONE',  ( -17.42409385541299471, -14.80920654474435771, 49.52966884056655772 ) ) ;
#10944 = CYLINDRICAL_SURFACE ( 'NONE', #14757, 0.1499999999999990508 ) ;
#10945 = VERTEX_POINT ( 'NONE', #31427 ) ;
#10946 = CARTESIAN_POINT ( 'NONE',  ( -23.65624057141237202, -11.51332318074561911, 66.72214514605295221 ) ) ;
#10947 = AXIS2_PLACEMENT_3D ( 'NONE', #29582, #25890, #40903 ) ;
#10948 = VECTOR ( 'NONE', #24638, 1000.000000000000000 ) ;
#10949 = CARTESIAN_POINT ( 'NONE',  ( -18.37632025677473990, -22.19811156716688672, 68.91491069639255329 ) ) ;
#10950 = ORIENTED_EDGE ( 'NONE', *, *, #6938, .T. ) ;
#10951 = ORIENTED_EDGE ( 'NONE', *, *, #34392, .F. ) ;
#10952 = CARTESIAN_POINT ( 'NONE',  ( -15.66159385650551705, -9.295667164867525756, 49.30633214617472504 ) ) ;
#10953 = CIRCLE ( 'NONE', #38460, 5.249999999999998224 ) ;
#10954 = CARTESIAN_POINT ( 'NONE',  ( -18.76558283008973049, -7.480892646508040755, 70.55563411965815135 ) ) ;
#10955 = DIRECTION ( 'NONE',  ( -3.071710424422018668E-17, 6.404604876783312462E-16, 1.000000000000000000 ) ) ;
#10956 = DIRECTION ( 'NONE',  ( 0.2122660683108583690, -0.9772119095896469876, 7.504255179194988334E-08 ) ) ;
#10957 = CARTESIAN_POINT ( 'NONE',  ( -12.84913006811349945, -9.445038364547627907, 74.32482815461490588 ) ) ;
#10958 = ORIENTED_EDGE ( 'NONE', *, *, #4285, .T. ) ;
#10959 = ORIENTED_EDGE ( 'NONE', *, *, #7604, .F. ) ;
#10960 = CARTESIAN_POINT ( 'NONE',  ( -15.80534385650551421, -8.801233750844183135, 48.81488406609782515 ) ) ;
#10961 = EDGE_CURVE ( 'NONE', #18657, #28606, #24781, .T. ) ;
#10962 = FACE_OUTER_BOUND ( 'NONE', #34263, .T. ) ;
#10963 = DIRECTION ( 'NONE',  ( 0.000000000000000000, -0.9999954153791273948, -0.003028072113819836944 ) ) ;
#10964 = CARTESIAN_POINT ( 'NONE',  ( -16.81784385650551528, -9.790100578890868377, 49.79778022625163203 ) ) ;
#10965 = ORIENTED_EDGE ( 'NONE', *, *, #32047, .F. ) ;
#10966 = CARTESIAN_POINT ( 'NONE',  ( -10.00731240618708462, -14.10555136595099945, 61.10316694600977172 ) ) ;
#10967 = CIRCLE ( 'NONE', #38483, 2.000000000000002665 ) ;
#10968 = CARTESIAN_POINT ( 'NONE',  ( -18.28630064832924162, -21.80992411731310909, 72.37691179419678633 ) ) ;
#10969 = LINE ( 'NONE', #36797, #11572 ) ;
#10970 = ORIENTED_EDGE ( 'NONE', *, *, #41608, .T. ) ;
#10971 = CARTESIAN_POINT ( 'NONE',  ( -11.19706266256277694, -11.50303319689152737, 67.63336710488009373 ) ) ;
#10972 = AXIS2_PLACEMENT_3D ( 'NONE', #19919, #1686, #1924 ) ;
#10973 = EDGE_CURVE ( 'NONE', #45300, #10364, #8750, .T. ) ;
#10974 = VERTEX_POINT ( 'NONE', #12718 ) ;
#10975 = CARTESIAN_POINT ( 'NONE',  ( -20.72409385541304161, -9.359200813967568422, 50.49621490985803263 ) ) ;
#10976 = CARTESIAN_POINT ( 'NONE',  ( -19.56314583254387074, -21.47448964078003186, 65.76486235662434865 ) ) ;
#10977 = EDGE_CURVE ( 'NONE', #39895, #38529, #36245, .T. ) ;
#10979 = EDGE_CURVE ( 'NONE', #16043, #26071, #41503, .T. ) ;
#10978 = DIRECTION ( 'NONE',  ( -3.071710424422018668E-17, 6.404604876783312462E-16, 1.000000000000000000 ) ) ;
#10980 = CARTESIAN_POINT ( 'NONE',  ( -9.990623027812100432, -14.31192454061599229, 64.57299275950818185 ) ) ;
#10981 = VERTEX_POINT ( 'NONE', #39542 ) ;
#10982 = AXIS2_PLACEMENT_3D ( 'NONE', #24151, #5444, #28572 ) ;
#10983 = CARTESIAN_POINT ( 'NONE',  ( -24.21176058185717750, -11.73806550877772459, 59.66048465809613077 ) ) ;
#10984 = CARTESIAN_POINT ( 'NONE',  ( -16.06904454444675778, -7.890656075740461795, 63.67011029959335389 ) ) ;
#10985 = CARTESIAN_POINT ( 'NONE',  ( -11.07857831884827604, -11.73724749328988359, 71.23860870961335934 ) ) ;
#10986 = VERTEX_POINT ( 'NONE', #2114 ) ;
#10987 = CARTESIAN_POINT ( 'NONE',  ( -19.49489006281195103, -21.96579734677897378, 62.15650173710307769 ) ) ;
#10988 = CARTESIAN_POINT ( 'NONE',  ( -24.10584571748465521, -12.56049761727124370, 73.39225570139795707 ) ) ;
#10989 = CARTESIAN_POINT ( 'NONE',  ( -18.39722185058254311, -7.818642594244027855, 70.52634850392742294 ) ) ;
#10990 = ORIENTED_EDGE ( 'NONE', *, *, #35784, .T. ) ;
#10991 = FACE_BOUND ( 'NONE', #7718, .T. ) ;
#10992 = ORIENTED_EDGE ( 'NONE', *, *, #37390, .T. ) ;
#10993 = CARTESIAN_POINT ( 'NONE',  ( -18.08661881476592015, -21.83173500943780354, 69.11514892715962333 ) ) ;
#10994 = FACE_OUTER_BOUND ( 'NONE', #44730, .T. ) ;
#10995 = AXIS2_PLACEMENT_3D ( 'NONE', #25108, #32947, #21887 ) ;
#10996 = LINE ( 'NONE', #6811, #44667 ) ;
#10997 = PLANE ( 'NONE',  #30616 ) ;
#10998 = ORIENTED_EDGE ( 'NONE', *, *, #10649, .T. ) ;
#10999 = CARTESIAN_POINT ( 'NONE',  ( -44.62409385541305795, -12.70920654474410760, 70.87000000000000455 ) ) ;
#11000 = VERTEX_POINT ( 'NONE', #20353 ) ;
#11001 = DIRECTION ( 'NONE',  ( -7.623677603559713149E-06, -4.209792907790860808E-06, 0.9999999999620784452 ) ) ;
#11002 = CARTESIAN_POINT ( 'NONE',  ( -15.00366368785993032, -21.85518728482429296, 65.22783942216084085 ) ) ;
#11003 = ORIENTED_EDGE ( 'NONE', *, *, #4473, .F. ) ;
#11004 = FACE_OUTER_BOUND ( 'NONE', #11067, .T. ) ;
#11005 = EDGE_CURVE ( 'NONE', #35282, #19390, #12945, .T. ) ;
#11006 = ORIENTED_EDGE ( 'NONE', *, *, #22044, .F. ) ;
#11007 = ORIENTED_EDGE ( 'NONE', *, *, #5206, .T. ) ;
#11008 = LINE ( 'NONE', #26032, #20306 ) ;
#11010 = CARTESIAN_POINT ( 'NONE',  ( -22.86572475812252847, -14.01004878893095196, 53.49999999999995026 ) ) ;
#11009 = AXIS2_PLACEMENT_3D ( 'NONE', #2498, #33228, #32303 ) ;
#11011 = CARTESIAN_POINT ( 'NONE',  ( -45.92409385541306222, -14.90920654474410867, 70.50000000000000000 ) ) ;
#11012 = CYLINDRICAL_SURFACE ( 'NONE', #12214, 0.1499999999999964972 ) ;
#11013 = CARTESIAN_POINT ( 'NONE',  ( -13.74654679279883851, -11.90422292133819582, 49.52966884056655772 ) ) ;
#11014 = LINE ( 'NONE', #21847, #1166 ) ;
#11015 = CARTESIAN_POINT ( 'NONE',  ( -17.82196845584967448, -7.369831403275952653, 60.28071967613077220 ) ) ;
#11016 = AXIS2_PLACEMENT_3D ( 'NONE', #5087, #16634, #27964 ) ;
#11017 = ORIENTED_EDGE ( 'NONE', *, *, #538, .T. ) ;
#11018 = VERTEX_POINT ( 'NONE', #35112 ) ;
#11019 = CARTESIAN_POINT ( 'NONE',  ( -12.08328018599459597, -10.28419721118101293, 64.22017573579350369 ) ) ;
#11020 = EDGE_CURVE ( 'NONE', #13357, #45579, #18439, .T. ) ;
#11021 = CARTESIAN_POINT ( 'NONE',  ( -24.72409385541305582, -14.80920654474417830, 64.04117647058822627 ) ) ;
#11022 = CARTESIAN_POINT ( 'NONE',  ( -21.84008232946753836, -9.377762178279809291, 63.49153780852771689 ) ) ;
#11023 = VECTOR ( 'NONE', #29854, 1000.000000000000114 ) ;
#11024 = CARTESIAN_POINT ( 'NONE',  ( -10.38078070663892660, -14.50222156296673148, 67.85800126083267969 ) ) ;
#11025 = PLANE ( 'NONE',  #48037 ) ;
#11026 = ORIENTED_EDGE ( 'NONE', *, *, #16294, .T. ) ;
#11027 =( BOUNDED_SURFACE ( )  B_SPLINE_SURFACE ( 3, 1, ( 
 ( #25085, #9594 ),
 ( #10310, #28540 ),
 ( #25326, #32472 ),
 ( #10061, #17441 ),
 ( #24609, #28296 ),
 ( #39611, #17672 ),
 ( #32235, #32928 ) ),
 .UNSPECIFIED., .T., .F., .F. ) 
 B_SPLINE_SURFACE_WITH_KNOTS ( ( 4, 3, 4 ),
 ( 2, 2 ),
 ( 0.000000000000000000, 0.5000000000000000000, 1.000000000000000000 ),
 ( 0.000000000000000000, 1.000000000000000000 ),
 .UNSPECIFIED. ) 
 GEOMETRIC_REPRESENTATION_ITEM ( )  RATIONAL_B_SPLINE_SURFACE ( (
 ( 1.000000000000000000, 1.000000000000000000),
 ( 0.3333333333333335369, 0.3333333333333330373),
 ( 0.3333333333333335369, 0.3333333333333330373),
 ( 1.000000000000000000, 1.000000000000000000),
 ( 0.3333333333333333703, 0.3333333333333333703),
 ( 0.3333333333333333703, 0.3333333333333333703),
 ( 1.000000000000000000, 1.000000000000000000) ) ) 
 REPRESENTATION_ITEM ( '' )  SURFACE ( )  );
#11028 = CARTESIAN_POINT ( 'NONE',  ( -14.64909385650551776, -8.104110260919579645, 48.81699501597546487 ) ) ;
#11029 = EDGE_LOOP ( 'NONE', ( #2892, #37068, #35031, #28582 ) ) ;
#11030 = CARTESIAN_POINT ( 'NONE',  ( -50.42609385541305755, -14.80920654474418008, 64.04117647058822627 ) ) ;
#11031 = FACE_OUTER_BOUND ( 'NONE', #570, .T. ) ;
#11032 = CARTESIAN_POINT ( 'NONE',  ( -21.18000274887674905, -20.77541536365158947, 69.05450184741354747 ) ) ;
#11033 = ORIENTED_EDGE ( 'NONE', *, *, #15705, .F. ) ;
#11034 = DIRECTION ( 'NONE',  ( 1.259531062780516415E-05, -2.755480461857868066E-06, 0.9999999999168828202 ) ) ;
#11035 =( BOUNDED_CURVE ( )  B_SPLINE_CURVE ( 3, ( #12162, #8468, #593, #23495 ),
 .UNSPECIFIED., .F., .F. ) 
 B_SPLINE_CURVE_WITH_KNOTS ( ( 4, 4 ),
 ( 0.5000000000000000000, 0.9074455897393631787 ),
 .UNSPECIFIED. ) 
 CURVE ( )  GEOMETRIC_REPRESENTATION_ITEM ( )  RATIONAL_B_SPLINE_CURVE ( ( 0.9999999999999987788, 0.4567392136813314685, 0.3561768502900308220, 0.6983129098260956180 ) ) 
 REPRESENTATION_ITEM ( '' )  );
#11036 = CARTESIAN_POINT ( 'NONE',  ( -17.77658133828675702, -19.49442885748621990, 52.02966884056656482 ) ) ;
#11037 = CARTESIAN_POINT ( 'NONE',  ( -14.76781046749041870, -8.332642942470114278, 60.61996286262948530 ) ) ;
#11038 = EDGE_CURVE ( 'NONE', #28383, #17957, #33897, .T. ) ;
#11039 = ORIENTED_EDGE ( 'NONE', *, *, #28820, .T. ) ;
#11040 = CARTESIAN_POINT ( 'NONE',  ( -10.12790085937091078, -16.31526762935427755, 71.54726743650820708 ) ) ;
#11041 = ORIENTED_EDGE ( 'NONE', *, *, #42366, .F. ) ;
#11042 = LINE ( 'NONE', #11291, #22837 ) ;
#11043 = AXIS2_PLACEMENT_3D ( 'NONE', #31736, #40805, #21388 ) ;
#11044 =( BOUNDED_SURFACE ( )  B_SPLINE_SURFACE ( 3, 1, ( 
 ( #39725, #9933 ),
 ( #39487, #40217 ),
 ( #25199, #6485 ),
 ( #43435, #2548 ),
 ( #44176, #5766 ),
 ( #20773, #13837 ),
 ( #47607, #6717 ) ),
 .UNSPECIFIED., .T., .F., .F. ) 
 B_SPLINE_SURFACE_WITH_KNOTS ( ( 4, 3, 4 ),
 ( 2, 2 ),
 ( 0.000000000000000000, 0.5000000000000000000, 1.000000000000000000 ),
 ( 0.000000000000000000, 1.000000000000000000 ),
 .UNSPECIFIED. ) 
 GEOMETRIC_REPRESENTATION_ITEM ( )  RATIONAL_B_SPLINE_SURFACE ( (
 ( 1.000000000000000000, 1.000000000000000000),
 ( 0.3333333333333335369, 0.3333333333333330373),
 ( 0.3333333333333335369, 0.3333333333333330373),
 ( 1.000000000000000000, 1.000000000000000000),
 ( 0.3333333333333333703, 0.3333333333333333703),
 ( 0.3333333333333333703, 0.3333333333333333703),
 ( 1.000000000000000000, 1.000000000000000000) ) ) 
 REPRESENTATION_ITEM ( '' )  SURFACE ( )  );
#11045 = EDGE_LOOP ( 'NONE', ( #15555, #23401 ) ) ;
#11046 = CARTESIAN_POINT ( 'NONE',  ( -10.33300584886465856, -17.09388629248971370, 57.88034695574707200 ) ) ;
#11047 = ADVANCED_FACE ( 'NONE', ( #35362 ), #27979, .T. ) ;
#11048 = PRODUCT_DEFINITION_SHAPE ( 'NONE', 'NONE',  #48740 ) ;
#11049 = EDGE_CURVE ( 'NONE', #16961, #23554, #21442, .T. ) ;
#11050 = CARTESIAN_POINT ( 'NONE',  ( -24.30048669258562555, -16.36410883687464946, 59.42332431756339162 ) ) ;
#11051 = EDGE_LOOP ( 'NONE', ( #38108, #37314 ) ) ;
#11052 = CARTESIAN_POINT ( 'NONE',  ( -22.14090652532222236, -20.04928072148792495, 62.51967078134249078 ) ) ;
#11053 = EDGE_CURVE ( 'NONE', #40137, #38583, #30251, .T. ) ;
#11054 = CARTESIAN_POINT ( 'NONE',  ( -20.20880001059865805, -8.386827409449249870, 70.55100337495873930 ) ) ;
#11055 = ORIENTED_EDGE ( 'NONE', *, *, #8543, .F. ) ;
#11056 = DIRECTION ( 'NONE',  ( -5.731567514496413899E-31, -1.020425574103664789E-16, -1.000000000000000000 ) ) ;
#11057 = AXIS2_PLACEMENT_3D ( 'NONE', #30415, #369, #4304 ) ;
#11058 = EDGE_CURVE ( 'NONE', #19923, #20471, #29189, .T. ) ;
#11059 = CARTESIAN_POINT ( 'NONE',  ( -18.11889358109259973, -21.82488563948435711, 65.64532159284070190 ) ) ;
#11060 = CARTESIAN_POINT ( 'NONE',  ( -24.86610167639389246, -14.46236660854407674, 66.29797298380238146 ) ) ;
#11061 = ORIENTED_EDGE ( 'NONE', *, *, #19715, .F. ) ;
#11062 = FACE_OUTER_BOUND ( 'NONE', #34869, .T. ) ;
#11063 = CARTESIAN_POINT ( 'NONE',  ( -23.73563655964320063, -11.66794921907180793, 63.25218274889858350 ) ) ;
#11064 = ADVANCED_FACE ( 'NONE', ( #10962 ), #21567, .T. ) ;
#11066 = EDGE_LOOP ( 'NONE', ( #7558, #45529 ) ) ;
#11065 = CIRCLE ( 'NONE', #32297, 1.250000000000001110 ) ;
#11067 = EDGE_LOOP ( 'NONE', ( #17225, #34239, #24188, #9952, #4708 ) ) ;
#11068 = CARTESIAN_POINT ( 'NONE',  ( -22.39254715322108780, -9.803279359720651343, 73.36672461330924477 ) ) ;
#11069 = CARTESIAN_POINT ( 'NONE',  ( -24.28619334359350290, -16.42731978468327014, 59.13804568661029037 ) ) ;
#11070 = CARTESIAN_POINT ( 'NONE',  ( -27.73618363589703506, -17.95286377743612505, 54.49999999999995026 ) ) ;
#11071 = CARTESIAN_POINT ( 'NONE',  ( -15.69284385759799427, -8.630756214087126565, 51.74842643355248129 ) ) ;
#11072 = CARTESIAN_POINT ( 'NONE',  ( -23.21383278545907558, -10.12064720979650190, 63.11540053722242050 ) ) ;
#11073 = CARTESIAN_POINT ( 'NONE',  ( -16.93761137771266689, -7.374984243389294036, 74.08205518084413654 ) ) ;
#11074 = CARTESIAN_POINT ( 'NONE',  ( -14.74956200268320039, -8.338905876961694830, 63.86149019104595226 ) ) ;
#11075 = ORIENTED_EDGE ( 'NONE', *, *, #19964, .T. ) ;
#11077 = CARTESIAN_POINT ( 'NONE',  ( -12.75497586646876691, -15.33350870067573979, 49.52966884056655772 ) ) ;
#11076 = CIRCLE ( 'NONE', #40175, 3.982850737850970990 ) ;
#11078 = CARTESIAN_POINT ( 'NONE',  ( -14.03871066829747249, -8.172719617054283958, 70.91452941929576070 ) ) ;
#11079 = AXIS2_PLACEMENT_3D ( 'NONE', #48224, #9848, #6147 ) ;
#11080 = LINE ( 'NONE', #26101, #32694 ) ;
#11081 = CARTESIAN_POINT ( 'NONE',  ( -16.51211807517087493, -22.20323055888632169, 65.33290249375183123 ) ) ;
#11082 = ORIENTED_EDGE ( 'NONE', *, *, #8465, .F. ) ;
#11083 = ORIENTED_EDGE ( 'NONE', *, *, #27733, .F. ) ;
#11084 = CARTESIAN_POINT ( 'NONE',  ( -24.72409385541305582, -14.90920654474410512, 56.99999999999998579 ) ) ;
#11085 = LINE ( 'NONE', #37154, #2459 ) ;
#11086 = CARTESIAN_POINT ( 'NONE',  ( -13.28646450387875966, -21.00477226788574114, 61.65612998380957777 ) ) ;
#11087 = CARTESIAN_POINT ( 'NONE',  ( -13.82438241372512699, -21.33197126505688601, 72.04890825305675151 ) ) ;
#11088 = CIRCLE ( 'NONE', #38609, 1.999999999999999556 ) ;
#11089 = ADVANCED_FACE ( 'NONE', ( #14860 ), #24467, .T. ) ;
#11090 = VERTEX_POINT ( 'NONE', #48625 ) ;
#11091 = FACE_OUTER_BOUND ( 'NONE', #5572, .T. ) ;
#11092 = CARTESIAN_POINT ( 'NONE',  ( -12.76547314785493192, -9.517330534081262172, 74.60450883341005124 ) ) ;
#11093 = EDGE_CURVE ( 'NONE', #11700, #7134, #40199, .T. ) ;
#11094 = AXIS2_PLACEMENT_3D ( 'NONE', #24073, #30743, #1655 ) ;
#11095 = EDGE_LOOP ( 'NONE', ( #34194, #31966, #23924, #33253, #36285 ) ) ;
#11096 = PLANE ( 'NONE',  #3232 ) ;
#11097 = B_SPLINE_CURVE_WITH_KNOTS ( 'NONE', 3,
 ( #26664, #22736, #11888, #26415, #12124, #322, #30613, #34032, #558, #41922 ),
 .UNSPECIFIED., .F., .F.,
 ( 4, 2, 2, 2, 4 ),
 ( 0.1272669073657947958, 0.2522669073462836531, 0.3772669073267724826, 0.5022669073072613122, 0.6272669072877501417 ),
 .UNSPECIFIED. ) ;
#11098 = CARTESIAN_POINT ( 'NONE',  ( -24.43235039625237803, -15.64544980915412431, 66.21891754810816622 ) ) ;
#11099 = ORIENTED_EDGE ( 'NONE', *, *, #31025, .F. ) ;
#11100 = CARTESIAN_POINT ( 'NONE',  ( -21.65477688667505518, -9.232350752012335349, 66.66149992610201025 ) ) ;
#11101 = ORIENTED_EDGE ( 'NONE', *, *, #46174, .F. ) ;
#11102 = PLANE ( 'NONE',  #31465 ) ;
#11103 = CARTESIAN_POINT ( 'NONE',  ( -24.40217295060720204, -14.25566147773195524, 69.95275273531336779 ) ) ;
#11104 = ORIENTED_EDGE ( 'NONE', *, *, #26391, .T. ) ;
#11105 = CARTESIAN_POINT ( 'NONE',  ( -10.38360249164154325, -14.43747963625415309, 67.87272197508832505 ) ) ;
#11106 = CARTESIAN_POINT ( 'NONE',  ( -24.72409385541305582, -15.80920654474410725, 65.99999999999998579 ) ) ;
#11107 = EDGE_CURVE ( 'NONE', #3454, #2663, #32989, .T. ) ;
#11108 = CARTESIAN_POINT ( 'NONE',  ( -20.02409385650551599, -6.426201560718813433, 50.50509628382439331 ) ) ;
#11109 = VECTOR ( 'NONE', #26503, 1000.000000000000114 ) ;
#11110 = CARTESIAN_POINT ( 'NONE',  ( -17.64597108892888500, -21.80612737151159664, 58.68936778192047399 ) ) ;
#11111 = ADVANCED_FACE ( 'NONE', ( #22283 ), #47901, .F. ) ;
#11112 = CARTESIAN_POINT ( 'NONE',  ( -24.47535868512742496, -14.65268306083313199, 66.59781357586173556 ) ) ;
#11113 = DIRECTION ( 'NONE',  ( 0.000000000000000000, 0.000000000000000000, 1.000000000000000000 ) ) ;
#11114 = DIRECTION ( 'NONE',  ( -0.2466764125338440639, -0.9690979039805150963, 7.162324212089591066E-08 ) ) ;
#11115 = ORIENTED_EDGE ( 'NONE', *, *, #27340, .F. ) ;
#11116 = VECTOR ( 'NONE', #13787, 1000.000000000000000 ) ;
#11117 = CARTESIAN_POINT ( 'NONE',  ( -16.91093646999636135, -22.24163895736238317, 72.28826323766482176 ) ) ;
#11118 = LINE ( 'NONE', #48050, #40018 ) ;
#11119 = CYLINDRICAL_SURFACE ( 'NONE', #45586, 2.000000000000001776 ) ;
#11120 = LINE ( 'NONE', #23178, #658 ) ;
#11121 = CARTESIAN_POINT ( 'NONE',  ( -16.19813999035177687, -21.75179513556690480, 58.28585572029250983 ) ) ;
#11122 = CARTESIAN_POINT ( 'NONE',  ( -22.81570869814190772, -9.667889350279351035, 73.58137470877635167 ) ) ;
#11123 = ORIENTED_EDGE ( 'NONE', *, *, #18050, .F. ) ;
#11124 = ORIENTED_EDGE ( 'NONE', *, *, #10263, .T. ) ;
#11125 = CARTESIAN_POINT ( 'NONE',  ( -16.90447120769729494, -21.79033274870119641, 72.18159849112339543 ) ) ;
#11126 = CARTESIAN_POINT ( 'NONE',  ( -14.84918562769068018, -8.299994025627823291, 57.04137321387239723 ) ) ;
#11127 = EDGE_LOOP ( 'NONE', ( #43749, #9745, #16519, #46490, #674 ) ) ;
#11128 = DIRECTION ( 'NONE',  ( 6.385196549736874992E-06, -5.147825522337142951E-06, 0.9999999999663644612 ) ) ;
#11129 = CYLINDRICAL_SURFACE ( 'NONE', #13704, 4.686499999999997002 ) ;
#11130 = CARTESIAN_POINT ( 'NONE',  ( -11.86838218109940790, -9.845554053733961197, 64.14419007574942100 ) ) ;
#11131 = FACE_OUTER_BOUND ( 'NONE', #35157, .T. ) ;
#11132 = EDGE_CURVE ( 'NONE', #38153, #46391, #46263, .T. ) ;
#11133 = DIRECTION ( 'NONE',  ( -1.000000000000000000, -2.866981220435666553E-17, -0.000000000000000000 ) ) ;
#11134 = DIRECTION ( 'NONE',  ( 2.117869074558178593E-07, 2.255668799892331646E-07, 0.9999999999999520384 ) ) ;
#11135 = CARTESIAN_POINT ( 'NONE',  ( -24.68275054790482770, -16.48720572190336853, 59.23837039904986312 ) ) ;
#11136 = CARTESIAN_POINT ( 'NONE',  ( -18.75147246090708109, -7.478239630221399814, 70.53101348938672288 ) ) ;
#11137 = VERTEX_POINT ( 'NONE', #6780 ) ;
#11138 = CIRCLE ( 'NONE', #24546, 2.000000000000000444 ) ;
#11139 = CARTESIAN_POINT ( 'NONE',  ( -11.32469211327616065, -18.34471187850051166, 57.95714594245092854 ) ) ;
#11140 = LINE ( 'NONE', #6956, #47845 ) ;
#11141 = B_SPLINE_CURVE_WITH_KNOTS ( 'NONE', 3,
 ( #47108, #9448, #31356, #8724, #31117, #13349, #28402, #1558, #35040, #5758 ),
 .UNSPECIFIED., .F., .F.,
 ( 4, 2, 2, 2, 4 ),
 ( 0.000000000000000000, 0.2500000000000000000, 0.5000000000000000000, 0.7500000000000000000, 1.000000000000000000 ),
 .UNSPECIFIED. ) ;
#11142 = CARTESIAN_POINT ( 'NONE',  ( -35.32409385541306079, -25.10920654474410441, 48.79999999999998295 ) ) ;
#11143 = CARTESIAN_POINT ( 'NONE',  ( -20.81159385759798752, -8.990409506049200417, 49.61344411288074951 ) ) ;
#11144 = CARTESIAN_POINT ( 'NONE',  ( -24.27033198218900978, -13.12649362337911718, 62.83264177274070050 ) ) ;
#11145 = CARTESIAN_POINT ( 'NONE',  ( -13.93897074462874919, -20.93787812888889377, 68.74153005185598886 ) ) ;
#11146 = CARTESIAN_POINT ( 'NONE',  ( -33.95962776134579286, -8.109206544744111511, 50.50000000000000000 ) ) ;
#11147 = VERTEX_POINT ( 'NONE', #25013 ) ;
#11148 = VERTEX_POINT ( 'NONE', #37276 ) ;
#11149 = B_SPLINE_CURVE_WITH_KNOTS ( 'NONE', 1,
 ( #5273, #23505 ),
 .UNSPECIFIED., .F., .F.,
 ( 2, 2 ),
 ( 0.000000000000000000, 1.000000000000000000 ),
 .UNSPECIFIED. ) ;
#11150 = CARTESIAN_POINT ( 'NONE',  ( -14.31159385541304374, -8.990409506049202193, 49.61344411288074951 ) ) ;
#11151 = VECTOR ( 'NONE', #2896, 1000.000000000000000 ) ;
#11152 = EDGE_LOOP ( 'NONE', ( #47329, #14900, #36931, #44090, #25450 ) ) ;
#11153 = CARTESIAN_POINT ( 'NONE',  ( -17.42403923091872642, -7.359153445762296464, 67.12765421629525520 ) ) ;
#11154 = AXIS2_PLACEMENT_3D ( 'NONE', #42197, #38978, #46380 ) ;
#11155 = CARTESIAN_POINT ( 'NONE',  ( -12.81450527785482230, -9.474959380418823685, 74.61923006088066757 ) ) ;
#11156 = ADVANCED_FACE ( 'NONE', ( #2830 ), #21328, .T. ) ;
#11157 = CARTESIAN_POINT ( 'NONE',  ( -50.42609385541305755, -14.90920654474427565, 73.99411764705880046 ) ) ;
#11158 = LINE ( 'NONE', #6732, #17510 ) ;
#11159 = VERTEX_POINT ( 'NONE', #21790 ) ;
#11160 = DIRECTION ( 'NONE',  ( 0.4156784896208475244, 0.1649587623211671294, 0.8944271909999157444 ) ) ;
#11161 = VECTOR ( 'NONE', #11887, 1000.000000000000114 ) ;
#11162 = CARTESIAN_POINT ( 'NONE',  ( -17.55304533075025475, -7.360155577183800979, 63.68910541025692140 ) ) ;
#11163 = ORIENTED_EDGE ( 'NONE', *, *, #4016, .T. ) ;
#11164 = DIRECTION ( 'NONE',  ( -1.642720032068235908E-15, -0.8949343913984794119, 0.4461977533473619473 ) ) ;
#11165 = CARTESIAN_POINT ( 'NONE',  ( -12.21883005507435271, -20.13911453956916375, 64.96700631603125942 ) ) ;
#11166 = EDGE_LOOP ( 'NONE', ( #42160, #38100, #8342, #45215, #31624 ) ) ;
#11167 = DIRECTION ( 'NONE',  ( 3.549360974554993999E-17, -6.371834667797928663E-18, -1.000000000000000000 ) ) ;
#11168 = CARTESIAN_POINT ( 'NONE',  ( -15.02609155194205393, -8.232647636148229253, 57.14999999999994884 ) ) ;
#11169 = DIRECTION ( 'NONE',  ( -0.7224352045700189739, -0.6914386272098739239, 9.340627272150576816E-09 ) ) ;
#11170 = ORIENTED_EDGE ( 'NONE', *, *, #26663, .T. ) ;
#11171 = CARTESIAN_POINT ( 'NONE',  ( -20.19651366439481421, -7.894145410699936249, 73.84379675463323167 ) ) ;
#11172 = EDGE_CURVE ( 'NONE', #24862, #7797, #9744, .T. ) ;
#11173 = DIRECTION ( 'NONE',  ( -0.9979768094191906469, -0.06357898915123129380, 0.000000000000000000 ) ) ;
#11174 = ADVANCED_FACE ( 'NONE', ( #18325 ), #32861, .T. ) ;
#11175 =( BOUNDED_CURVE ( )  B_SPLINE_CURVE ( 2, ( #3861, #38054, #14899, #41036, #19349, #44995, #37819, #18363, #19112 ),
 .UNSPECIFIED., .F., .F. ) 
 B_SPLINE_CURVE_WITH_KNOTS ( ( 3, 2, 2, 2, 3 ),
 ( 0.07474742020699134959, 0.07573079478573833956, 0.07671416936448531565, 0.07769754394323229174, 0.07868091852197928171 ),
 .UNSPECIFIED. ) 
 CURVE ( )  GEOMETRIC_REPRESENTATION_ITEM ( )  RATIONAL_B_SPLINE_CURVE ( ( 0.9999999999988991028, 0.9238795325123876356, 1.000000000000000000, 0.9238795325112867385, 1.000000000000000000, 0.9238795325112867385, 1.000000000000000000, 0.9238795325112550971, 1.000000000000031530 ) ) 
 REPRESENTATION_ITEM ( '' )  );
#11176 = DIRECTION ( 'NONE',  ( -0.5729733056696844073, 0.8195740302071247152, 7.403245352187747277E-08 ) ) ;
#11177 = DIRECTION ( 'NONE',  ( 1.164780374791175599E-15, -0.8949343913984055821, -0.4461977533475099955 ) ) ;
#11178 = ORIENTED_EDGE ( 'NONE', *, *, #12102, .F. ) ;
#11179 = CARTESIAN_POINT ( 'NONE',  ( -9.979935309495182594, -14.51290508331406670, 68.05074287064346095 ) ) ;
#11180 = CARTESIAN_POINT ( 'NONE',  ( -24.47217469393258327, -14.64471774706559515, 62.86296487297660462 ) ) ;
#11181 = CARTESIAN_POINT ( 'NONE',  ( -11.42622172434740158, -18.51434208396348069, 61.42710833180511543 ) ) ;
#11182 = CARTESIAN_POINT ( 'NONE',  ( -17.91840021365262814, -21.79173196354552644, 62.17535923606572368 ) ) ;
#11183 = B_SPLINE_CURVE_WITH_KNOTS ( 'NONE', 3,
 ( #18368, #40538, #18121, #10749, #14172, #25054, #33374, #28978, #33138, #29227 ),
 .UNSPECIFIED., .F., .F.,
 ( 4, 2, 2, 2, 4 ),
 ( 0.000000000000000000, 0.2500000000000000000, 0.5000000000000000000, 0.7500000000000000000, 1.000000000000000000 ),
 .UNSPECIFIED. ) ;
#11184 = ADVANCED_FACE ( 'NONE', ( #17602 ), #18196, .T. ) ;
#11185 = CARTESIAN_POINT ( 'NONE',  ( -18.75534385650551528, -7.417179338643134834, 52.18511593390279302 ) ) ;
#11186 = ORIENTED_EDGE ( 'NONE', *, *, #22491, .T. ) ;
#11187 = VECTOR ( 'NONE', #23700, 1000.000000000000000 ) ;
#11188 = CARTESIAN_POINT ( 'NONE',  ( -17.70014646425873295, -22.25421675543054789, 58.52836462438737897 ) ) ;
#11189 = DIRECTION ( 'NONE',  ( 0.1261685609230672744, 0.9920088176193796459, 5.058037262945178220E-08 ) ) ;
#11190 = ORIENTED_EDGE ( 'NONE', *, *, #16936, .F. ) ;
#11191 = CARTESIAN_POINT ( 'NONE',  ( -11.33876662530985513, -19.10724307639906883, 68.33876836528679632 ) ) ;
#11192 = EDGE_CURVE ( 'NONE', #13199, #23558, #34846, .T. ) ;
#11193 = CARTESIAN_POINT ( 'NONE',  ( -41.17556444364835500, -14.90920654474426499, 72.98823529411762934 ) ) ;
#11194 = DIRECTION ( 'NONE',  ( 1.224646799147353207E-16, 1.000000000000000000, -1.912410701131276611E-32 ) ) ;
#11195 = ORIENTED_EDGE ( 'NONE', *, *, #24428, .T. ) ;
#11196 = CARTESIAN_POINT ( 'NONE',  ( -18.37786432726835883, -21.79469297182707521, 69.10042588711679912 ) ) ;
#11197 =( BOUNDED_CURVE ( )  B_SPLINE_CURVE ( 3, ( #36677, #7174, #36448, #44128 ),
 .UNSPECIFIED., .F., .F. ) 
 B_SPLINE_CURVE_WITH_KNOTS ( ( 4, 4 ),
 ( 4.712388980384689674, 4.921828490624009511 ),
 .UNSPECIFIED. ) 
 CURVE ( )  GEOMETRIC_REPRESENTATION_ITEM ( )  RATIONAL_B_SPLINE_CURVE ( ( 1.000000000000000000, 0.9963479302455154896, 0.9963479302455154896, 1.000000000000000000 ) ) 
 REPRESENTATION_ITEM ( '' )  );
#11198 = B_SPLINE_CURVE_WITH_KNOTS ( 'NONE', 1,
 ( #13831, #32568 ),
 .UNSPECIFIED., .F., .F.,
 ( 2, 2 ),
 ( 0.000000000000000000, 1.000000000000000000 ),
 .UNSPECIFIED. ) ;
#11199 = CARTESIAN_POINT ( 'NONE',  ( -23.44663229712023877, -18.37710346651732962, 73.04902823781205257 ) ) ;
#11200 = ORIENTED_EDGE ( 'NONE', *, *, #30851, .F. ) ;
#11201 = VERTEX_POINT ( 'NONE', #8021 ) ;
#11202 = CARTESIAN_POINT ( 'NONE',  ( -14.81784385650551528, -9.790100578890868377, 49.79778022625163203 ) ) ;
#11203 = CARTESIAN_POINT ( 'NONE',  ( -12.83553897491427342, -8.939779468292423203, 67.53976116287044817 ) ) ;
#11204 = CYLINDRICAL_SURFACE ( 'NONE', #7259, 1.249999999999998668 ) ;
#11205 = CARTESIAN_POINT ( 'NONE',  ( -15.55171241031346696, -7.598245096497682205, 70.79485117658632021 ) ) ;
#11206 = EDGE_CURVE ( 'NONE', #17004, #18610, #37782, .T. ) ;
#11207 = CARTESIAN_POINT ( 'NONE',  ( -13.38575581802539993, -9.030060914960570173, 60.72478133471773987 ) ) ;
#11208 = EDGE_CURVE ( 'NONE', #29545, #20111, #17823, .T. ) ;
#11209 = ORIENTED_EDGE ( 'NONE', *, *, #32345, .T. ) ;
#11210 = ORIENTED_EDGE ( 'NONE', *, *, #3491, .T. ) ;
#11211 = CARTESIAN_POINT ( 'NONE',  ( -13.12522125891144853, -9.020171137055317701, 48.97007792487355005 ) ) ;
#11212 = B_SPLINE_CURVE_WITH_KNOTS ( 'NONE', 1,
 ( #34587, #18849 ),
 .UNSPECIFIED., .F., .F.,
 ( 2, 2 ),
 ( 0.000000000000000000, 1.000000000000000000 ),
 .UNSPECIFIED. ) ;
#11213 = CARTESIAN_POINT ( 'NONE',  ( -21.33694466872984918, -9.004932385753821933, 73.90128753631783809 ) ) ;
#11214 = CARTESIAN_POINT ( 'NONE',  ( -13.76849323099554567, -20.83774554052356009, 65.27156739751333703 ) ) ;
#11215 = ADVANCED_FACE ( 'NONE', ( #19316 ), #23035, .T. ) ;
#11216 = CARTESIAN_POINT ( 'NONE',  ( -14.56784385650551528, -6.428312510596451368, 51.20221977374900035 ) ) ;
#11217 = ORIENTED_EDGE ( 'NONE', *, *, #19995, .T. ) ;
#11218 = CARTESIAN_POINT ( 'NONE',  ( -45.92409385541306222, -13.70421070448077039, 68.00000000000000000 ) ) ;
#11219 = CARTESIAN_POINT ( 'NONE',  ( -12.75497586646876691, -15.33350870067573979, 49.52966884056655772 ) ) ;
#11220 = CARTESIAN_POINT ( 'NONE',  ( -11.21783104652298846, -18.93062367394879431, 64.93202350587574756 ) ) ;
#11221 = VERTEX_POINT ( 'NONE', #11213 ) ;
#11222 = CARTESIAN_POINT ( 'NONE',  ( -24.47217469780904153, -14.64471797168181233, 63.01296487297644688 ) ) ;
#11223 = ORIENTED_EDGE ( 'NONE', *, *, #42209, .T. ) ;
#11224 = CARTESIAN_POINT ( 'NONE',  ( -22.27695970603427966, -9.156476278077038344, 59.97817131676683999 ) ) ;
#11225 = CARTESIAN_POINT ( 'NONE',  ( -24.83668925967022290, -14.06191770065747981, 73.26238150409892569 ) ) ;
#11226 = CARTESIAN_POINT ( 'NONE',  ( -24.39669641284641699, -17.43334540211986550, 69.52065623779036230 ) ) ;
#11227 = CARTESIAN_POINT ( 'NONE',  ( -9.991237185789255904, -14.30336124839046263, 64.49465555223780200 ) ) ;
#11228 = VERTEX_POINT ( 'NONE', #41734 ) ;
#11229 = CARTESIAN_POINT ( 'NONE',  ( -10.83541799943766293, -17.32598710976732903, 61.04254427365582103 ) ) ;
#11230 = CARTESIAN_POINT ( 'NONE',  ( -22.78151503426583702, -19.98625364524674097, 72.75905110386234753 ) ) ;
#11231 = DIRECTION ( 'NONE',  ( -8.419732596317119940E-06, 4.907637675873463559E-06, 0.9999999999525115424 ) ) ;
#11232 = VERTEX_POINT ( 'NONE', #30905 ) ;
#11233 = CARTESIAN_POINT ( 'NONE',  ( -10.37394849890712401, -14.76283852923608286, 71.61310637325181006 ) ) ;
#11234 = DIRECTION ( 'NONE',  ( -3.071710424422018668E-17, 6.404604876783312462E-16, 1.000000000000000000 ) ) ;
#11235 = CARTESIAN_POINT ( 'NONE',  ( -10.73038759976291878, -11.53849795754883623, 71.28199172907763170 ) ) ;
#11236 = FACE_BOUND ( 'NONE', #26065, .T. ) ;
#11238 = EDGE_LOOP ( 'NONE', ( #22031, #7072, #15647, #44775, #43956 ) ) ;
#11237 = EDGE_CURVE ( 'NONE', #27788, #30260, #18833, .T. ) ;
#11239 = DIRECTION ( 'NONE',  ( -8.262539633966638414E-06, 9.998826072665628149E-07, 0.9999999999653652605 ) ) ;
#11240 = DIRECTION ( 'NONE',  ( 0.9687793358424821033, -0.2479245821708677133, 0.000000000000000000 ) ) ;
#11241 = CARTESIAN_POINT ( 'NONE',  ( -24.42122136640115571, -14.60445272614867562, 63.01296493458807646 ) ) ;
#11242 = EDGE_CURVE ( 'NONE', #2922, #10698, #19820, .T. ) ;
#11243 = CARTESIAN_POINT ( 'NONE',  ( -15.95707318215220205, -7.504986700048139170, 63.85506303619484214 ) ) ;
#11244 = ORIENTED_EDGE ( 'NONE', *, *, #347, .F. ) ;
#11245 = DIRECTION ( 'NONE',  ( -1.000000000000000000, -2.866981220435666553E-17, -0.000000000000000000 ) ) ;
#11246 = EDGE_LOOP ( 'NONE', ( #18284, #28091, #5391, #37052, #48149 ) ) ;
#11247 = CARTESIAN_POINT ( 'NONE',  ( -22.78678303852979425, -9.565966637465477262, 53.49999999999994316 ) ) ;
#11248 = CARTESIAN_POINT ( 'NONE',  ( -16.17583575424048092, -10.27959207348368764, 49.52966884056655772 ) ) ;
#11249 = CARTESIAN_POINT ( 'NONE',  ( -14.54749350918765671, -8.372447261038937327, 64.07506791522041567 ) ) ;
#11250 = ORIENTED_EDGE ( 'NONE', *, *, #31095, .T. ) ;
#11251 = CARTESIAN_POINT ( 'NONE',  ( -21.48052744822966531, -21.05892743585564375, 72.71101825924023387 ) ) ;
#11252 = CARTESIAN_POINT ( 'NONE',  ( -11.00662809167565470, -17.60509476157276865, 68.32395370577452809 ) ) ;
#11253 = ORIENTED_EDGE ( 'NONE', *, *, #21753, .T. ) ;
#11254 = ORIENTED_EDGE ( 'NONE', *, *, #3076, .F. ) ;
#11255 = ORIENTED_EDGE ( 'NONE', *, *, #28655, .T. ) ;
#11256 = CARTESIAN_POINT ( 'NONE',  ( -15.39388989008627995, -21.97733388496078177, 72.23070757706680922 ) ) ;
#11257 = CARTESIAN_POINT ( 'NONE',  ( -24.39403702774331606, -17.44049340399234893, 69.52844358061491903 ) ) ;
#11258 = CARTESIAN_POINT ( 'NONE',  ( -20.24919536711601964, -8.341303680600599790, 63.46688622775676691 ) ) ;
#11259 = CARTESIAN_POINT ( 'NONE',  ( -24.23307633429531194, -12.98099662095383344, 66.30806553712001516 ) ) ;
#11260 = EDGE_CURVE ( 'NONE', #36681, #14637, #5625, .T. ) ;
#11261 = DIRECTION ( 'NONE',  ( -3.413470714839332458E-33, 1.190614954331866791E-16, -1.000000000000000000 ) ) ;
#11262 = CARTESIAN_POINT ( 'NONE',  ( -13.52409385541304410, -9.359200813967568422, 50.49621490985803263 ) ) ;
#11263 = EDGE_CURVE ( 'NONE', #36043, #39613, #21663, .T. ) ;
#11264 = VERTEX_POINT ( 'NONE', #19564 ) ;
#11265 = ORIENTED_EDGE ( 'NONE', *, *, #38935, .F. ) ;
#11266 = CARTESIAN_POINT ( 'NONE',  ( -17.56717618076180187, -7.360494862701306928, 63.73552352176282909 ) ) ;
#11267 = EDGE_CURVE ( 'NONE', #700, #44129, #2588, .T. ) ;
#11268 = ADVANCED_FACE ( 'NONE', ( #15120 ), #30178, .T. ) ;
#11269 = ADVANCED_FACE ( 'NONE', ( #24242 ), #28168, .T. ) ;
#11270 = CARTESIAN_POINT ( 'NONE',  ( -22.48987839669337419, -20.27190899980916328, 65.81147567037690749 ) ) ;
#11271 = CARTESIAN_POINT ( 'NONE',  ( -21.84008380685302342, -9.377763380601791710, 63.19153780853375935 ) ) ;
#11272 = SHAPE_REPRESENTATION ( 'Attachment Screw', ( #29031 ), #23534 ) ;
#11273 = DIRECTION ( 'NONE',  ( -0.3478314405900310158, -0.9375570856950865561, 0.000000000000000000 ) ) ;
#11274 = ORIENTED_EDGE ( 'NONE', *, *, #28985, .F. ) ;
#11275 = CARTESIAN_POINT ( 'NONE',  ( -16.28034385650551741, -6.424090610841176385, 49.80797279389977916 ) ) ;
#11276 = ORIENTED_EDGE ( 'NONE', *, *, #26052, .F. ) ;
#11277 = CARTESIAN_POINT ( 'NONE',  ( -16.07504252742545603, -21.67928465087502232, 58.51415545652290717 ) ) ;
#11278 = CARTESIAN_POINT ( 'NONE',  ( -11.61908885153752813, -23.53148341178916425, 53.49999999999995026 ) ) ;
#11279 = AXIS2_PLACEMENT_3D ( 'NONE', #32111, #32364, #24248 ) ;
#11280 = DIRECTION ( 'NONE',  ( -3.071710424422018668E-17, 6.404604876783312462E-16, 1.000000000000000000 ) ) ;
#11281 = ORIENTED_EDGE ( 'NONE', *, *, #39533, .F. ) ;
#11282 = CARTESIAN_POINT ( 'NONE',  ( -23.37999588001404661, -18.58199455739222827, 69.57899840282863124 ) ) ;
#11283 = DIRECTION ( 'NONE',  ( 1.209056813000714825E-06, 5.657077699801570473E-07, 0.9999999999991090460 ) ) ;
#11284 = CARTESIAN_POINT ( 'NONE',  ( -21.59308387932192730, -9.186008246182964854, 66.67652394132250038 ) ) ;
#11285 = EDGE_CURVE ( 'NONE', #25938, #8282, #30164, .T. ) ;
#11286 = ORIENTED_EDGE ( 'NONE', *, *, #28789, .T. ) ;
#11287 = CARTESIAN_POINT ( 'NONE',  ( -10.37462439815953275, -14.89569326811688832, 74.94778901494476031 ) ) ;
#11288 = PLANE ( 'NONE',  #37724 ) ;
#11289 = CARTESIAN_POINT ( 'NONE',  ( -23.88368001943721453, -17.64091657838220328, 66.35845829618112646 ) ) ;
#11290 = ORIENTED_EDGE ( 'NONE', *, *, #34879, .F. ) ;
#11291 = CARTESIAN_POINT ( 'NONE',  ( -46.29409385541305966, -14.20920654474410760, 71.05212771298751306 ) ) ;
#11292 = VERTEX_POINT ( 'NONE', #28417 ) ;
#11293 = CARTESIAN_POINT ( 'NONE',  ( -9.975020038748654727, -14.69173609724344054, 71.47782692972722884 ) ) ;
#11294 = CARTESIAN_POINT ( 'NONE',  ( -24.87307799990805535, -14.67875618097862045, 62.83579567226647811 ) ) ;
#11295 = ORIENTED_EDGE ( 'NONE', *, *, #15829, .T. ) ;
#11296 = CARTESIAN_POINT ( 'NONE',  ( -45.85858821786293049, -14.20920654474410760, 69.94787228701220272 ) ) ;
#11297 = CARTESIAN_POINT ( 'NONE',  ( -11.08849928128054430, -11.70861240866882547, 74.65019981390956616 ) ) ;
#11298 = FACE_OUTER_BOUND ( 'NONE', #21036, .T. ) ;
#11299 = EDGE_CURVE ( 'NONE', #3450, #5029, #38324, .T. ) ;
#11300 = ORIENTED_EDGE ( 'NONE', *, *, #13897, .F. ) ;
#11301 = FACE_OUTER_BOUND ( 'NONE', #14392, .T. ) ;
#11302 = CARTESIAN_POINT ( 'NONE',  ( -38.65852941833841783, -25.10920654474410441, 78.99999999999998579 ) ) ;
#11303 = CARTESIAN_POINT ( 'NONE',  ( -10.93882922636242583, -17.44414199431199819, 68.09721938813615338 ) ) ;
#11304 = EDGE_LOOP ( 'NONE', ( #37409, #20821 ) ) ;
#11305 = CARTESIAN_POINT ( 'NONE',  ( -17.33262245845742910, -7.759502110702281463, 67.30567542699309058 ) ) ;
#11306 = B_SPLINE_CURVE_WITH_KNOTS ( 'NONE', 1,
 ( #35550, #46406 ),
 .UNSPECIFIED., .F., .F.,
 ( 2, 2 ),
 ( 0.000000000000000000, 1.000000000000000000 ),
 .UNSPECIFIED. ) ;
#11307 = CARTESIAN_POINT ( 'NONE',  ( -23.59327504554355315, -11.39630409041826020, 69.90682860766239060 ) ) ;
#11308 = DIRECTION ( 'NONE',  ( -0.9118114225829224706, -0.4106092176842892627, -5.589476761700638069E-08 ) ) ;
#11309 = AXIS2_PLACEMENT_3D ( 'NONE', #12618, #17011, #31578 ) ;
#11310 = ORIENTED_EDGE ( 'NONE', *, *, #9953, .T. ) ;
#11311 = ORIENTED_EDGE ( 'NONE', *, *, #7922, .F. ) ;
#11312 = DIRECTION ( 'NONE',  ( -2.866981220435666553E-17, 1.000000000000000000, 1.190614954331866791E-16 ) ) ;
#11313 = CARTESIAN_POINT ( 'NONE',  ( -23.46647660864419294, -19.16733412182131246, 62.39760931945144051 ) ) ;
#11314 = ORIENTED_EDGE ( 'NONE', *, *, #5429, .F. ) ;
#11315 = CARTESIAN_POINT ( 'NONE',  ( -13.83659385759798965, -8.995762431863214559, 51.38120296130585274 ) ) ;
#11316 = CARTESIAN_POINT ( 'NONE',  ( -24.82750207115152463, -13.97654542584719373, 73.30766806548945169 ) ) ;
#11317 =( BOUNDED_CURVE ( )  B_SPLINE_CURVE ( 3, ( #39437, #12839, #42662, #39184 ),
 .UNSPECIFIED., .F., .F. ) 
 B_SPLINE_CURVE_WITH_KNOTS ( ( 4, 4 ),
 ( 0.5000000000000000000, 0.9074455897393687298 ),
 .UNSPECIFIED. ) 
 CURVE ( )  GEOMETRIC_REPRESENTATION_ITEM ( )  RATIONAL_B_SPLINE_CURVE ( ( 1.000000000000003775, 0.4567392136813261949, 0.3561768502900253264, 0.6983129098261054990 ) ) 
 REPRESENTATION_ITEM ( '' )  );
#11318 = CARTESIAN_POINT ( 'NONE',  ( -11.55673057814116333, -10.21815940138198009, 71.01247170384147012 ) ) ;
#11319 = FACE_OUTER_BOUND ( 'NONE', #9021, .T. ) ;
#11320 = ORIENTED_EDGE ( 'NONE', *, *, #3638, .F. ) ;
#11321 = CARTESIAN_POINT ( 'NONE',  ( -10.44202790750644461, -14.30845231023897846, 64.38803863533676974 ) ) ;
#11322 = EDGE_CURVE ( 'NONE', #29174, #44867, #26066, .T. ) ;
#11323 = EDGE_CURVE ( 'NONE', #39442, #38153, #31146, .T. ) ;
#11324 = CARTESIAN_POINT ( 'NONE',  ( -18.59601872632196518, -7.856991649524070809, 73.85536540707786912 ) ) ;
#11325 = CARTESIAN_POINT ( 'NONE',  ( -10.52215087187021325, -13.37195826583270808, 74.67817647370830514 ) ) ;
#11326 =( BOUNDED_CURVE ( )  B_SPLINE_CURVE ( 3, ( #20144, #42573, #27774, #16678 ),
 .UNSPECIFIED., .F., .F. ) 
 B_SPLINE_CURVE_WITH_KNOTS ( ( 4, 4 ),
 ( 0.000000000000000000, 0.4074455897393671755 ),
 .UNSPECIFIED. ) 
 CURVE ( )  GEOMETRIC_REPRESENTATION_ITEM ( )  RATIONAL_B_SPLINE_CURVE ( ( 1.000000000000000000, 0.4567392136813245296, 0.3561768502900275468, 0.6983129098261091627 ) ) 
 REPRESENTATION_ITEM ( '' )  );
#11327 = ORIENTED_EDGE ( 'NONE', *, *, #17446, .F. ) ;
#11328 = EDGE_CURVE ( 'NONE', #12343, #2068, #46827, .T. ) ;
#11329 = EDGE_CURVE ( 'NONE', #15253, #897, #26412, .T. ) ;
#11330 = ORIENTED_EDGE ( 'NONE', *, *, #17222, .T. ) ;
#11331 = DIRECTION ( 'NONE',  ( -1.000000000000000000, 4.164305804376849172E-17, -1.614929280266638808E-16 ) ) ;
#11332 = CARTESIAN_POINT ( 'NONE',  ( -15.38564177817468526, -21.97495498498005162, 72.15237147290109476 ) ) ;
#11333 = CARTESIAN_POINT ( 'NONE',  ( -17.03575403388767384, -5.365376231199011414, 53.49999999999995026 ) ) ;
#11334 = ORIENTED_EDGE ( 'NONE', *, *, #7016, .F. ) ;
#11335 = CARTESIAN_POINT ( 'NONE',  ( -23.57564663096156821, -11.46866237256667986, 66.43716952005193832 ) ) ;
#11336 =( BOUNDED_SURFACE ( )  B_SPLINE_SURFACE ( 3, 1, ( 
 ( #8757, #23774 ),
 ( #5054, #46661 ),
 ( #5293, #20064 ),
 ( #20309, #12907 ),
 ( #35316, #27931 ),
 ( #32372, #32123 ),
 ( #36744, #40465 ) ),
 .UNSPECIFIED., .T., .F., .F. ) 
 B_SPLINE_SURFACE_WITH_KNOTS ( ( 4, 3, 4 ),
 ( 2, 2 ),
 ( 0.000000000000000000, 0.5000000000000000000, 1.000000000000000000 ),
 ( 0.000000000000000000, 1.000000000000000000 ),
 .UNSPECIFIED. ) 
 GEOMETRIC_REPRESENTATION_ITEM ( )  RATIONAL_B_SPLINE_SURFACE ( (
 ( 1.000000000000000000, 1.000000000000000000),
 ( 0.3333333333333335369, 0.3333333333333330373),
 ( 0.3333333333333335369, 0.3333333333333330373),
 ( 1.000000000000000000, 1.000000000000000000),
 ( 0.3333333333333333703, 0.3333333333333333703),
 ( 0.3333333333333333703, 0.3333333333333333703),
 ( 1.000000000000000000, 1.000000000000000000) ) ) 
 REPRESENTATION_ITEM ( '' )  SURFACE ( )  );
#11337 = LINE ( 'NONE', #3956, #7625 ) ;
#11338 = ADVANCED_FACE ( 'NONE', ( #20549 ), #12888, .T. ) ;
#11339 = VECTOR ( 'NONE', #19785, 1000.000000000000227 ) ;
#11340 = EDGE_LOOP ( 'NONE', ( #7885, #37907, #927, #6981, #29060, #37389, #38132, #9719, #16973, #38195, #36495, #34333, #14893 ) ) ;
#11341 = CARTESIAN_POINT ( 'NONE',  ( -21.84103824432629892, -20.31425616591354455, 62.37872033649042436 ) ) ;
#11342 = ORIENTED_EDGE ( 'NONE', *, *, #11260, .T. ) ;
#11343 = DIRECTION ( 'NONE',  ( 0.000000000000000000, 0.000000000000000000, 1.000000000000000000 ) ) ;
#11344 = EDGE_LOOP ( 'NONE', ( #31185, #39297 ) ) ;
#11345 = CARTESIAN_POINT ( 'NONE',  ( -19.23170823189057543, -21.62663761134119156, 62.40992444795293892 ) ) ;
#11346 = CARTESIAN_POINT ( 'NONE',  ( -20.52762626839951210, -8.534807245883811788, 63.61121513079540080 ) ) ;
#11347 = EDGE_LOOP ( 'NONE', ( #12364, #45299, #12674, #47214, #518, #47023, #32631, #17701, #30466, #47662, #23667, #39583, #7818, #39768, #19267, #41057, #27028, #17735, #12271, #40946, #38357, #16032, #11290, #5091, #26523, #43842, #18648, #1954, #31164, #22376, #19183, #20849, #43870, #44846, #18536, #36133, #46459, #6769, #8076, #28217, #39623, #38848, #6903, #38216, #4438, #18117, #13510, #20618, #22835, #33322, #22468, #47682, #21117, #14741, #32858, #37658, #42711, #13604, #28342, #48723, #31110, #7130, #35901, #24282, #43375, #41083, #13797, #36528, #39078, #14797, #11715, #19158, #41317, #33837, #39532, #29566, #22328, #22654, #11460, #43517, #18641, #25306, #26906, #5707, #18968, #38995, #35087, #19639, #32418, #18105, #37364, #43875, #23100, #18269, #21307, #13028, #14360, #31270, #44724, #12510, #23264, #40155, #35351, #4417, #792, #4288, #45852, #24121, #15379, #44267, #14051, #46134, #21419, #35076, #24764, #27018, #37253, #47770, #5046, #13338, #37194, #5515, #41044, #33870, #4053, #5442, #11736, #22799, #33057, #35998, #23423, #44239, #37323, #10273, #1832, #36601, #22595, #722, #6701, #41494, #18796, #15347, #42825, #13295, #26454, #37395, #9062, #24399, #547, #9581, #23598, #18759, #40705, #44778, #38571, #34877, #34040, #42443, #22827, #13579, #17526, #42207, #25667, #20363, #26098 ) ) ;
#11348 = CARTESIAN_POINT ( 'NONE',  ( -17.22281210278579167, -7.361840297529252730, 70.60540404266352255 ) ) ;
#11349 = DIRECTION ( 'NONE',  ( -2.866981220435666553E-17, 1.000000000000000000, 1.190614954331866791E-16 ) ) ;
#11350 = CARTESIAN_POINT ( 'NONE',  ( -21.14909385650551599, -8.104110260919577868, 48.81699501597546487 ) ) ;
#11351 = CARTESIAN_POINT ( 'NONE',  ( -21.35069750557218526, -21.14061989791981944, 69.19416854129514149 ) ) ;
#11352 = CARTESIAN_POINT ( 'NONE',  ( -24.20836943865575464, -17.88934756284849215, 62.66016244028183024 ) ) ;
#11353 = CARTESIAN_POINT ( 'NONE',  ( -10.51883074965326870, -17.60604944894409130, 68.25868426185122928 ) ) ;
#11354 = VERTEX_POINT ( 'NONE', #42943 ) ;
#11355 = CARTESIAN_POINT ( 'NONE',  ( -16.19589554557147792, -7.461143648330228473, 60.35028476078848314 ) ) ;
#11356 = CARTESIAN_POINT ( 'NONE',  ( -10.38752013045322009, -14.36951432065623635, 64.67331771650336236 ) ) ;
#11357 = CARTESIAN_POINT ( 'NONE',  ( -18.24855905490383279, -21.76054561525072373, 65.57205495431095699 ) ) ;
#11358 = CARTESIAN_POINT ( 'NONE',  ( -17.42409385541305511, -14.80920654474410725, 47.99999999999998579 ) ) ;
#11359 = DIRECTION ( 'NONE',  ( 0.6380325334150260819, -0.7700094066334536302, 0.000000000000000000 ) ) ;
#11360 = CARTESIAN_POINT ( 'NONE',  ( -14.98297878932515381, -10.79466886532025605, 49.52966884056655772 ) ) ;
#11361 = VERTEX_POINT ( 'NONE', #8742 ) ;
#11362 = VERTEX_POINT ( 'NONE', #38760 ) ;
#11363 = CARTESIAN_POINT ( 'NONE',  ( -11.15620858584903807, -11.58171791265060691, 67.91864592172348125 ) ) ;
#11364 = CARTESIAN_POINT ( 'NONE',  ( -14.95042625923249702, -8.260719279109913771, 57.14999999999994884 ) ) ;
#11365 = VERTEX_POINT ( 'NONE', #46650 ) ;
#11366 = CARTESIAN_POINT ( 'NONE',  ( -21.01123855637963089, -20.87838213191899683, 65.58453944497207999 ) ) ;
#11367 = CARTESIAN_POINT ( 'NONE',  ( -23.34481533081060434, -18.63641918517796370, 69.44371984263474928 ) ) ;
#11368 = CARTESIAN_POINT ( 'NONE',  ( -14.45223855097109578, -8.412213402796462347, 70.82137677761178907 ) ) ;
#11369 = DIRECTION ( 'NONE',  ( 9.063790940987422061E-17, 0.3090169943749398462, 0.9510565162951560847 ) ) ;
#11370 = CARTESIAN_POINT ( 'NONE',  ( -11.13733870171179596, -11.61806121328042174, 67.90392505421056057 ) ) ;
#11371 = DIRECTION ( 'NONE',  ( 0.6607190350373968180, 0.7506333037770515082, 0.000000000000000000 ) ) ;
#11372 = VECTOR ( 'NONE', #18762, 1000.000000000000000 ) ;
#11373 = FACE_OUTER_BOUND ( 'NONE', #24291, .T. ) ;
#11374 = CARTESIAN_POINT ( 'NONE',  ( -45.92409385541306222, -13.70421070448076861, 70.50000000000000000 ) ) ;
#11375 = EDGE_CURVE ( 'NONE', #44310, #40803, #32496, .T. ) ;
#11376 = CARTESIAN_POINT ( 'NONE',  ( -20.33143355559478138, -8.386436920021669295, 67.07544311258112657 ) ) ;
#11377 = CARTESIAN_POINT ( 'NONE',  ( -15.63656756482722443, -8.039962711168056941, 74.30815578088962070 ) ) ;
#11378 = CARTESIAN_POINT ( 'NONE',  ( -18.89533436007378597, -9.769568524266553311, 49.52966884056655772 ) ) ;
#11379 = CARTESIAN_POINT ( 'NONE',  ( -9.424093855413055110, -27.10920654474410796, 56.99999999999997868 ) ) ;
#11380 = FACE_OUTER_BOUND ( 'NONE', #38894, .T. ) ;
#11381 = CARTESIAN_POINT ( 'NONE',  ( -10.63726236355470078, -16.73075914568876144, 57.77940687674663423 ) ) ;
#11382 = ORIENTED_EDGE ( 'NONE', *, *, #11511, .F. ) ;
#11383 = ORIENTED_EDGE ( 'NONE', *, *, #28446, .F. ) ;
#11384 = CARTESIAN_POINT ( 'NONE',  ( -15.77409385541304232, -6.859212275519751323, 50.50378509014259265 ) ) ;
#11385 = EDGE_CURVE ( 'NONE', #33983, #46443, #24958, .T. ) ;
#11386 = ORIENTED_EDGE ( 'NONE', *, *, #38662, .F. ) ;
#11387 = CARTESIAN_POINT ( 'NONE',  ( -23.53769205375521167, -19.06701183966639945, 65.98535978091517507 ) ) ;
#11388 = ADVANCED_FACE ( 'NONE', ( #21744 ), #39978, .T. ) ;
#11389 = FACE_OUTER_BOUND ( 'NONE', #34804, .T. ) ;
#11390 = EDGE_CURVE ( 'NONE', #46448, #32393, #1348, .T. ) ;
#11391 = CARTESIAN_POINT ( 'NONE',  ( -13.60238289842206072, -8.884932333444998775, 57.26967755503795132 ) ) ;
#11392 = CARTESIAN_POINT ( 'NONE',  ( -17.77594409791816688, -7.367433943401969998, 60.26556080592736464 ) ) ;
#11393 = VERTEX_POINT ( 'NONE', #40689 ) ;
#11394 = CARTESIAN_POINT ( 'NONE',  ( -23.11979735578276163, -10.00689463417326053, 66.73520565964795992 ) ) ;
#11395 = CYLINDRICAL_SURFACE ( 'NONE', #34377, 0.1500000000000059897 ) ;
#11396 = EDGE_LOOP ( 'NONE', ( #40627, #44077, #12011, #19609, #1024 ) ) ;
#11397 = CARTESIAN_POINT ( 'NONE',  ( -19.01159385759799036, -8.990409506049200417, 49.61344411288074951 ) ) ;
#11398 = DIRECTION ( 'NONE',  ( 0.000000000000000000, 0.000000000000000000, 1.000000000000000000 ) ) ;
#11399 = ORIENTED_EDGE ( 'NONE', *, *, #34830, .F. ) ;
#11400 = CARTESIAN_POINT ( 'NONE',  ( -11.14868235907462335, -10.79371162966233832, 57.37049761327430275 ) ) ;
#11401 = CARTESIAN_POINT ( 'NONE',  ( -21.51080377022508472, -17.10312989180209087, 49.52966884056655772 ) ) ;
#11402 = VERTEX_POINT ( 'NONE', #33046 ) ;
#11403 = CARTESIAN_POINT ( 'NONE',  ( -22.53655473247544805, -20.22829521909097394, 65.88917159596024931 ) ) ;
#11404 = CIRCLE ( 'NONE', #28700, 5.249999999999998224 ) ;
#11405 = PLANE ( 'NONE',  #8462 ) ;
#11406 = CARTESIAN_POINT ( 'NONE',  ( -11.90843004312087494, -10.41235542147202153, 74.73885506873732254 ) ) ;
#11407 = CARTESIAN_POINT ( 'NONE',  ( -10.55151165865014384, -17.68520938540437371, 68.28217272534745064 ) ) ;
#11408 = ORIENTED_EDGE ( 'NONE', *, *, #39997, .F. ) ;
#11409 = CARTESIAN_POINT ( 'NONE',  ( -11.71918404020638427, -18.95175453447547653, 71.70158022526054253 ) ) ;
#11410 = DIRECTION ( 'NONE',  ( 2.181982678098338148E-16, 0.000000000000000000, -1.000000000000000000 ) ) ;
#11411 = CARTESIAN_POINT ( 'NONE',  ( -20.49170831689750472, -8.461258797198503601, 63.59649424907593129 ) ) ;
#11412 = CARTESIAN_POINT ( 'NONE',  ( -23.37999588001404661, -18.58199455739222827, 69.57899840282863124 ) ) ;
#11413 = CARTESIAN_POINT ( 'NONE',  ( -16.14669044099090556, -7.469368122434191903, 60.33881929519913712 ) ) ;
#11414 = CARTESIAN_POINT ( 'NONE',  ( -50.42609385541305755, -14.90920654474416907, 63.03529411764704804 ) ) ;
#11415 = CARTESIAN_POINT ( 'NONE',  ( -18.69909385650551670, -8.114302828567740988, 52.18300498402516041 ) ) ;
#11416 = ORIENTED_EDGE ( 'NONE', *, *, #32121, .F. ) ;
#11417 = DIRECTION ( 'NONE',  ( -0.3478314405900307382, -0.9375570856950865561, 0.000000000000000000 ) ) ;
#11418 = CARTESIAN_POINT ( 'NONE',  ( -14.79551189520038967, -8.264331297124348552, 64.20467431377564083 ) ) ;
#11419 = VERTEX_POINT ( 'NONE', #10905 ) ;
#11420 = CARTESIAN_POINT ( 'NONE',  ( -18.39027086422678536, -7.876143750135766730, 74.06737643580208896 ) ) ;
#11421 = CARTESIAN_POINT ( 'NONE',  ( -22.52510384832546109, -10.01533137145497676, 73.78161092902590212 ) ) ;
#11422 = CARTESIAN_POINT ( 'NONE',  ( -18.46801905451614090, -7.836623195388690455, 74.12592262855558545 ) ) ;
#11423 = ADVANCED_FACE ( 'NONE', ( #43933 ), #17554, .T. ) ;
#11424 = VERTEX_POINT ( 'NONE', #48090 ) ;
#11425 = DIRECTION ( 'NONE',  ( -5.551115123125782702E-17, -1.232595164407830946E-32, -1.000000000000000000 ) ) ;
#11426 = CARTESIAN_POINT ( 'NONE',  ( -18.39951368268757648, -22.19516171751901368, 69.00010101991060196 ) ) ;
#11427 = EDGE_LOOP ( 'NONE', ( #47016, #14907, #13913, #12891 ) ) ;
#11428 = CARTESIAN_POINT ( 'NONE',  ( -13.69284385650552061, -7.406986770994973490, 48.81910596585309747 ) ) ;
#11429 = B_SPLINE_CURVE_WITH_KNOTS ( 'NONE', 3,
 ( #25061, #32680, #48424, #14653, #13708, #6344, #43780, #29475, #29719, #47700 ),
 .UNSPECIFIED., .F., .F.,
 ( 4, 2, 2, 2, 4 ),
 ( 0.000000000000000000, 0.2500000000000000000, 0.5000000000000000000, 0.7500000000000000000, 1.000000000000000000 ),
 .UNSPECIFIED. ) ;
#11430 = CARTESIAN_POINT ( 'NONE',  ( -14.39270346209745988, -8.498217395175695188, 70.95787461648006911 ) ) ;
#11431 = CARTESIAN_POINT ( 'NONE',  ( -10.89013669529741790, -17.45722423822778779, 68.10281702760276801 ) ) ;
#11432 = CARTESIAN_POINT ( 'NONE',  ( -15.48563737764182591, -8.027819004131977465, 70.49500973495348433 ) ) ;
#11433 = DIRECTION ( 'NONE',  ( -1.000000000000000000, 0.000000000000000000, 0.000000000000000000 ) ) ;
#11434 = VERTEX_POINT ( 'NONE', #44646 ) ;
#11435 = EDGE_LOOP ( 'NONE', ( #637, #30964, #29585, #15767, #32272 ) ) ;
#11436 = CIRCLE ( 'NONE', #6729, 2.000000000000003109 ) ;
#11437 = CARTESIAN_POINT ( 'NONE',  ( -14.96159385650551776, -9.295667164867525756, 49.30633214617472504 ) ) ;
#11438 = ADVANCED_FACE ( 'NONE', ( #32360 ), #28290, .T. ) ;
#11439 = DIRECTION ( 'NONE',  ( -3.071710424422018668E-17, 6.404604876783312462E-16, 1.000000000000000000 ) ) ;
#11440 = CARTESIAN_POINT ( 'NONE',  ( -11.68672710392437608, -10.05669134056747005, 67.68392285705759548 ) ) ;
#11441 = ADVANCED_FACE ( 'NONE', ( #2779 ), #36164, .T. ) ;
#11442 =( BOUNDED_CURVE ( )  B_SPLINE_CURVE ( 3, ( #28875, #5761, #32349, #9699 ),
 .UNSPECIFIED., .F., .F. ) 
 B_SPLINE_CURVE_WITH_KNOTS ( ( 4, 4 ),
 ( 1.570796326794896780, 1.780235837034217505 ),
 .UNSPECIFIED. ) 
 CURVE ( )  GEOMETRIC_REPRESENTATION_ITEM ( )  RATIONAL_B_SPLINE_CURVE ( ( 1.000000000000000000, 0.9963479302455154896, 0.9963479302455154896, 1.000000000000000000 ) ) 
 REPRESENTATION_ITEM ( '' )  );
#11443 = CARTESIAN_POINT ( 'NONE',  ( -15.97409385650551705, -9.792211528768504536, 50.49490371617623197 ) ) ;
#11444 = B_SPLINE_CURVE_WITH_KNOTS ( 'NONE', 3,
 ( #47370, #43183, #27911, #42934, #47114, #38990, #39485, #17545, #28409, #13835 ),
 .UNSPECIFIED., .F., .F.,
 ( 4, 2, 2, 2, 4 ),
 ( 0.1272669073658669048, 0.2522669073463478795, 0.3772669073268288820, 0.5022669073073098289, 0.6272669072877907759 ),
 .UNSPECIFIED. ) ;
#11445 = ADVANCED_FACE ( 'NONE', ( #11389 ), #2814, .T. ) ;
#11446 = CARTESIAN_POINT ( 'NONE',  ( -16.13263948075386978, -7.878200451182638453, 63.68483172840383588 ) ) ;
#11447 = CARTESIAN_POINT ( 'NONE',  ( -11.93522140360746242, -14.45952210441258678, 54.07175714974879099 ) ) ;
#11448 = CYLINDRICAL_SURFACE ( 'NONE', #26802, 5.249999999999998224 ) ;
#11449 = CARTESIAN_POINT ( 'NONE',  ( -11.56806251476610115, -18.73522173559940995, 65.03234934376791898 ) ) ;
#11450 = EDGE_CURVE ( 'NONE', #24111, #18890, #39422, .T. ) ;
#11451 = VERTEX_POINT ( 'NONE', #8425 ) ;
#11452 =( BOUNDED_SURFACE ( )  B_SPLINE_SURFACE ( 3, 1, ( 
 ( #6588, #21609 ),
 ( #32905, #14180 ),
 ( #29234, #44273 ),
 ( #10526, #25532 ),
 ( #21842, #36836 ),
 ( #18131, #3122 ),
 ( #23078, #26765 ) ),
 .UNSPECIFIED., .T., .F., .F. ) 
 B_SPLINE_SURFACE_WITH_KNOTS ( ( 4, 3, 4 ),
 ( 2, 2 ),
 ( 0.000000000000000000, 0.5000000000000000000, 1.000000000000000000 ),
 ( 0.000000000000000000, 1.000000000000000000 ),
 .UNSPECIFIED. ) 
 GEOMETRIC_REPRESENTATION_ITEM ( )  RATIONAL_B_SPLINE_SURFACE ( (
 ( 1.000000000000000000, 1.000000000000000000),
 ( 0.3333333333333335369, 0.3333333333333330373),
 ( 0.3333333333333335369, 0.3333333333333330373),
 ( 1.000000000000000000, 1.000000000000000000),
 ( 0.3333333333333333703, 0.3333333333333333703),
 ( 0.3333333333333333703, 0.3333333333333333703),
 ( 1.000000000000000000, 1.000000000000000000) ) ) 
 REPRESENTATION_ITEM ( '' )  SURFACE ( )  );
#11453 = DIRECTION ( 'NONE',  ( 0.000000000000000000, 1.000000000000000000, -0.000000000000000000 ) ) ;
#11454 =( BOUNDED_CURVE ( )  B_SPLINE_CURVE ( 3, ( #46718, #42297, #23832, #38834 ),
 .UNSPECIFIED., .F., .F. ) 
 B_SPLINE_CURVE_WITH_KNOTS ( ( 4, 4 ),
 ( 0.5000000000000000000, 0.9074455897393605142 ),
 .UNSPECIFIED. ) 
 CURVE ( )  GEOMETRIC_REPRESENTATION_ITEM ( )  RATIONAL_B_SPLINE_CURVE ( ( 0.9999999999999941158, 0.4567392136813325232, 0.3561768502900345412, 0.6983129098260937306 ) ) 
 REPRESENTATION_ITEM ( '' )  );
#11455 = ORIENTED_EDGE ( 'NONE', *, *, #432, .T. ) ;
#11456 = CARTESIAN_POINT ( 'NONE',  ( -13.01353397724842154, -8.804979801064929390, 64.09441804368185558 ) ) ;
#11457 = CARTESIAN_POINT ( 'NONE',  ( -10.11824970337647223, -16.26811690260224452, 71.56254994910038647 ) ) ;
#11458 = CARTESIAN_POINT ( 'NONE',  ( -12.52591642561268515, -9.195683996340104471, 74.50418400381258266 ) ) ;
#11459 = CARTESIAN_POINT ( 'NONE',  ( -18.16972350937645686, -22.22180848762789296, 65.54520937023384874 ) ) ;
#11460 = ORIENTED_EDGE ( 'NONE', *, *, #27395, .T. ) ;
#11461 = CARTESIAN_POINT ( 'NONE',  ( -13.28405640107581220, -24.63958226071216728, 54.49999999999995026 ) ) ;
#11462 = FACE_OUTER_BOUND ( 'NONE', #6721, .T. ) ;
#11463 = CARTESIAN_POINT ( 'NONE',  ( -20.10157833785231674, -8.341446982617696904, 70.26602821964115719 ) ) ;
#11464 = CARTESIAN_POINT ( 'NONE',  ( -24.31456749111805848, -16.04512898536875198, 66.07941623514170715 ) ) ;
#11465 = VERTEX_POINT ( 'NONE', #11155 ) ;
#11466 = CARTESIAN_POINT ( 'NONE',  ( -10.52422430310768320, -17.61911375464911700, 68.21226508126260057 ) ) ;
#11467 = CARTESIAN_POINT ( 'NONE',  ( -46.48018488037470064, -16.43194983366065642, 70.50000000000000000 ) ) ;
#11469 =( BOUNDED_CURVE ( )  B_SPLINE_CURVE ( 3, ( #21634, #13501, #28544, #35665 ),
 .UNSPECIFIED., .F., .F. ) 
 B_SPLINE_CURVE_WITH_KNOTS ( ( 4, 4 ),
 ( 0.000000000000000000, 0.4074455897393634562 ),
 .UNSPECIFIED. ) 
 CURVE ( )  GEOMETRIC_REPRESENTATION_ITEM ( )  RATIONAL_B_SPLINE_CURVE ( ( 1.000000000000000000, 0.4567392136813352432, 0.3561768502900315436, 0.6983129098260888457 ) ) 
 REPRESENTATION_ITEM ( '' )  );
#11468 = CARTESIAN_POINT ( 'NONE',  ( -10.73412848974934874, -11.53077067998621175, 71.20365450754333381 ) ) ;
#11470 = AXIS2_PLACEMENT_3D ( 'NONE', #3381, #25547, #21621 ) ;
#11471 = FACE_BOUND ( 'NONE', #30499, .T. ) ;
#11472 = APPLICATION_PROTOCOL_DEFINITION ( 'draft international standard', 'automotive_design', 1998, #28121 ) ;
#11473 = ORIENTED_EDGE ( 'NONE', *, *, #27484, .T. ) ;
#11474 = CARTESIAN_POINT ( 'NONE',  ( -13.17849012079414095, -20.93114571188291961, 58.23924207018498578 ) ) ;
#11475 = CARTESIAN_POINT ( 'NONE',  ( -20.49775566701509177, -11.27142682889164327, 49.52966884056655772 ) ) ;
#11476 = CARTESIAN_POINT ( 'NONE',  ( -24.42218830102925509, -14.64588410380239480, 62.71296487252168816 ) ) ;
#11477 = CARTESIAN_POINT ( 'NONE',  ( -21.08681864223905578, -8.776014225774568800, 73.75695571861821520 ) ) ;
#11478 = ORIENTED_EDGE ( 'NONE', *, *, #21006, .T. ) ;
#11479 = CARTESIAN_POINT ( 'NONE',  ( -10.11857101092534528, -16.26968670661729632, 71.70396332877544410 ) ) ;
#11480 = VERTEX_POINT ( 'NONE', #4484 ) ;
#11481 = CARTESIAN_POINT ( 'NONE',  ( -22.10679845867080928, -14.99777973644470919, 49.52966884056655772 ) ) ;
#11482 = CARTESIAN_POINT ( 'NONE',  ( -16.99415041099795332, -7.769321291326151346, 70.37547239324983650 ) ) ;
#11483 = EDGE_CURVE ( 'NONE', #17387, #2275, #17216, .T. ) ;
#11484 = CARTESIAN_POINT ( 'NONE',  ( -14.35020019311386719, -8.022098033332648370, 63.90323595109556720 ) ) ;
#11485 = ORIENTED_EDGE ( 'NONE', *, *, #15293, .F. ) ;
#11486 = CARTESIAN_POINT ( 'NONE',  ( -13.53684336123755472, -20.63065685511644887, 58.15535990049952630 ) ) ;
#11487 = B_SPLINE_CURVE_WITH_KNOTS ( 'NONE', 3,
 ( #7691, #777, #22705, #41652, #30828, #37697, #3735, #11861, #34490, #3988 ),
 .UNSPECIFIED., .F., .F.,
 ( 4, 2, 2, 2, 4 ),
 ( 0.1272669073658512784, 0.2522669073463361111, 0.3772669073268208884, 0.5022669073073057211, 0.6272669072877905538 ),
 .UNSPECIFIED. ) ;
#11488 = ORIENTED_EDGE ( 'NONE', *, *, #12947, .T. ) ;
#11489 = EDGE_LOOP ( 'NONE', ( #24579, #12220, #37965, #3311, #26362 ) ) ;
#11490 = EDGE_LOOP ( 'NONE', ( #46242, #11931, #27717, #15087, #25262 ) ) ;
#11491 = LINE ( 'NONE', #41285, #555 ) ;
#11492 = CYLINDRICAL_SURFACE ( 'NONE', #7657, 0.1499999999999949984 ) ;
#11493 = CARTESIAN_POINT ( 'NONE',  ( -19.30706890485013005, -22.01740903849647069, 58.64011989901568711 ) ) ;
#11494 = CARTESIAN_POINT ( 'NONE',  ( -20.49170831689750827, -8.461258797198503601, 63.59649424907591708 ) ) ;
#11495 = CARTESIAN_POINT ( 'NONE',  ( -16.92409385541305511, -14.80920654474410547, 48.99999999999997868 ) ) ;
#11496 = CARTESIAN_POINT ( 'NONE',  ( -16.19814381282456495, -21.75179583453235210, 58.58585572026735377 ) ) ;
#11497 = EDGE_CURVE ( 'NONE', #36884, #21817, #48570, .T. ) ;
#11498 = CARTESIAN_POINT ( 'NONE',  ( -20.10534385541302882, -7.595227055684739881, 51.75156210489597441 ) ) ;
#11499 = ORIENTED_EDGE ( 'NONE', *, *, #10651, .F. ) ;
#11500 = VERTEX_POINT ( 'NONE', #319 ) ;
#11501 = CARTESIAN_POINT ( 'NONE',  ( -11.98246295270348050, -15.60836430055780610, 53.49999999999995026 ) ) ;
#11502 = CARTESIAN_POINT ( 'NONE',  ( -13.87531073599090448, -8.258727944021641676, 74.39943442283376385 ) ) ;
#11503 = B_SPLINE_CURVE_WITH_KNOTS ( 'NONE', 1,
 ( #7823, #30713 ),
 .UNSPECIFIED., .F., .F.,
 ( 2, 2 ),
 ( 0.000000000000000000, 1.000000000000000000 ),
 .UNSPECIFIED. ) ;
#11504 = FACE_OUTER_BOUND ( 'NONE', #9873, .T. ) ;
#11505 = DIRECTION ( 'NONE',  ( 1.000000000000000000, -4.164305804376849172E-17, 1.614929280266638808E-16 ) ) ;
#11506 = ORIENTED_EDGE ( 'NONE', *, *, #48681, .T. ) ;
#11507 = CARTESIAN_POINT ( 'NONE',  ( -16.89909385650551599, -8.114302828567740988, 52.18300498402516041 ) ) ;
#11508 = VECTOR ( 'NONE', #30802, 1000.000000000000000 ) ;
#11509 = AXIS2_PLACEMENT_3D ( 'NONE', #6657, #40869, #22406 ) ;
#11510 = ORIENTED_EDGE ( 'NONE', *, *, #15800, .T. ) ;
#11511 = EDGE_CURVE ( 'NONE', #4743, #33825, #9559, .T. ) ;
#11512 = CARTESIAN_POINT ( 'NONE',  ( -20.03282965983824226, -21.84088468745754597, 53.89198173725360874 ) ) ;
#11513 = CARTESIAN_POINT ( 'NONE',  ( -50.42609385541305755, -14.80920654474411613, 58.00588235294116402 ) ) ;
#11514 = CARTESIAN_POINT ( 'NONE',  ( -10.43949455435184603, -13.84896052950683298, 57.46297163929641982 ) ) ;
#11515 = EDGE_CURVE ( 'NONE', #22937, #1590, #37467, .T. ) ;
#11516 = B_SPLINE_CURVE_WITH_KNOTS ( 'NONE', 3,
 ( #26556, #7617, #14228, #3168, #15209, #10566, #41579, #6868, #11054, #37123 ),
 .UNSPECIFIED., .F., .F.,
 ( 4, 2, 2, 2, 4 ),
 ( 0.000000000000000000, 0.2500000000000000000, 0.5000000000000000000, 0.7500000000000000000, 1.000000000000000000 ),
 .UNSPECIFIED. ) ;
#11517 = EDGE_LOOP ( 'NONE', ( #23031, #31405, #43274, #27289 ) ) ;
#11518 = CARTESIAN_POINT ( 'NONE',  ( -20.35888297561835003, -7.961606991444354797, 70.45111537669373547 ) ) ;
#11519 = CARTESIAN_POINT ( 'NONE',  ( -14.68149645524703928, -8.368787582623010479, 60.39284412189408613 ) ) ;
#11520 = ORIENTED_EDGE ( 'NONE', *, *, #7541, .F. ) ;
#11521 = CARTESIAN_POINT ( 'NONE',  ( -10.43429035678604500, -13.88957849880590700, 57.44825060447983844 ) ) ;
#11522 = EDGE_CURVE ( 'NONE', #17919, #38294, #29869, .T. ) ;
#11523 = CARTESIAN_POINT ( 'NONE',  ( -10.41921500249975807, -15.63170790598816140, 64.92260423241262401 ) ) ;
#11524 = CARTESIAN_POINT ( 'NONE',  ( -24.29205067375949056, -17.69794899492463713, 66.13012485676826202 ) ) ;
#11525 = EDGE_LOOP ( 'NONE', ( #2385, #9017, #27037, #23304, #5445 ) ) ;
#11526 = DIRECTION ( 'NONE',  ( -3.913797937844888413E-06, -1.965591629113562018E-06, -0.9999999999904092274 ) ) ;
#11527 = EDGE_CURVE ( 'NONE', #18661, #18610, #44902, .T. ) ;
#11528 = ORIENTED_EDGE ( 'NONE', *, *, #8919, .F. ) ;
#11529 = DIRECTION ( 'NONE',  ( 0.04287186434519785205, 0.9990805789562556827, -2.806673972535358096E-09 ) ) ;
#11530 = CARTESIAN_POINT ( 'NONE',  ( -24.72694788909437236, -16.28301151488813403, 62.70833397083087846 ) ) ;
#11531 = ORIENTED_EDGE ( 'NONE', *, *, #48522, .T. ) ;
#11532 = ADVANCED_FACE ( 'NONE', ( #26656 ), #77, .T. ) ;
#11533 = EDGE_CURVE ( 'NONE', #9803, #22122, #26411, .T. ) ;
#11534 = DIRECTION ( 'NONE',  ( 0.2189141945955470070, -0.9757441136919980940, 0.000000000000000000 ) ) ;
#11535 = CARTESIAN_POINT ( 'NONE',  ( -24.14679772577363437, -12.68507108172156883, 70.05770892828130059 ) ) ;
#11536 = CARTESIAN_POINT ( 'NONE',  ( -18.54310121003094736, -22.17474206275902660, 72.39236802054413999 ) ) ;
#11537 = ORIENTED_EDGE ( 'NONE', *, *, #39795, .T. ) ;
#11538 = CARTESIAN_POINT ( 'NONE',  ( -22.23348325011687976, -19.89560912233985590, 66.00421727876722855 ) ) ;
#11539 = CARTESIAN_POINT ( 'NONE',  ( -11.46189391869686958, -11.14137219122531697, 57.22405587208396582 ) ) ;
#11540 = ORIENTED_EDGE ( 'NONE', *, *, #18323, .T. ) ;
#11541 = FACE_OUTER_BOUND ( 'NONE', #25483, .T. ) ;
#11542 = AXIS2_PLACEMENT_3D ( 'NONE', #23135, #45549, #27057 ) ;
#11543 = CARTESIAN_POINT ( 'NONE',  ( -21.47456293661849713, -9.038556783377254433, 70.41660404402310292 ) ) ;
#11544 = ORIENTED_EDGE ( 'NONE', *, *, #11522, .T. ) ;
#11545 = VERTEX_POINT ( 'NONE', #22731 ) ;
#11546 = CARTESIAN_POINT ( 'NONE',  ( -22.80992488001626128, -10.33718742043409122, 66.55798901525795941 ) ) ;
#11547 = CARTESIAN_POINT ( 'NONE',  ( -10.69964535969413433, -11.60199994243103028, 71.26577769276515539 ) ) ;
#11548 = CARTESIAN_POINT ( 'NONE',  ( -36.42409385541304800, -8.109206544743658540, 50.50000000000030553 ) ) ;
#11549 = DIRECTION ( 'NONE',  ( -1.000000000000000000, 0.000000000000000000, 0.000000000000000000 ) ) ;
#11550 =( BOUNDED_CURVE ( )  B_SPLINE_CURVE ( 3, ( #12160, #1073, #16072, #4522 ),
 .UNSPECIFIED., .F., .F. ) 
 B_SPLINE_CURVE_WITH_KNOTS ( ( 4, 4 ),
 ( 1.675516081914546707, 1.780235837034217505 ),
 .UNSPECIFIED. ) 
 CURVE ( )  GEOMETRIC_REPRESENTATION_ITEM ( )  RATIONAL_B_SPLINE_CURVE ( ( 1.000000000000000000, 0.9990863565030491111, 0.9990863565030491111, 1.000000000000000000 ) ) 
 REPRESENTATION_ITEM ( '' )  );
#11551 = AXIS2_PLACEMENT_3D ( 'NONE', #16683, #28269, #31723 ) ;
#11552 = CARTESIAN_POINT ( 'NONE',  ( -21.73659385650551812, -6.915538690918074494, 49.31353937987644542 ) ) ;
#11553 = FACE_OUTER_BOUND ( 'NONE', #18846, .T. ) ;
#11554 = DIRECTION ( 'NONE',  ( -0.8604039311673230550, -0.5096126717731922495, 7.110477544621476444E-08 ) ) ;
#11555 = LINE ( 'NONE', #28023, #34983 ) ;
#11556 = CARTESIAN_POINT ( 'NONE',  ( -9.975266540682891758, -14.95048458752718545, 74.93632366797223199 ) ) ;
#11557 = ORIENTED_EDGE ( 'NONE', *, *, #28985, .T. ) ;
#11558 = CARTESIAN_POINT ( 'NONE',  ( -10.43125849979191955, -13.91324152291312366, 57.74825034919034294 ) ) ;
#11559 =( LENGTH_UNIT ( ) NAMED_UNIT ( * ) SI_UNIT ( .MILLI., .METRE. ) );
#11560 = CARTESIAN_POINT ( 'NONE',  ( -10.03807673793979838, -13.83450552870046479, 57.55550895888026020 ) ) ;
#11561 = DIRECTION ( 'NONE',  ( 0.9687793358424819923, -0.2479245821708680464, 0.000000000000000000 ) ) ;
#11562 = EDGE_LOOP ( 'NONE', ( #21592, #38526, #10930, #37191, #12292 ) ) ;
#11563 = EDGE_LOOP ( 'NONE', ( #43050, #28849, #21285, #26323 ) ) ;
#11564 = EDGE_CURVE ( 'NONE', #33331, #1365, #17898, .T. ) ;
#11565 = DIRECTION ( 'NONE',  ( -3.071710424422018668E-17, 6.404604876783312462E-16, 1.000000000000000000 ) ) ;
#11566 = CARTESIAN_POINT ( 'NONE',  ( -10.64823572114831585, -13.04561703115311566, 71.31901764264975441 ) ) ;
#11567 = DIRECTION ( 'NONE',  ( 3.071710424422018668E-17, -6.404604876783312462E-16, -1.000000000000000000 ) ) ;
#11568 = DIRECTION ( 'NONE',  ( -5.731567514496413899E-31, -1.020425574103664789E-16, -1.000000000000000000 ) ) ;
#11569 = ORIENTED_EDGE ( 'NONE', *, *, #15248, .T. ) ;
#11570 = CARTESIAN_POINT ( 'NONE',  ( -11.54484398236026799, -18.70636738123116061, 61.48530584391141929 ) ) ;
#11571 = AXIS2_PLACEMENT_3D ( 'NONE', #16631, #46688, #42987 ) ;
#11572 = VECTOR ( 'NONE', #32238, 1000.000000000000000 ) ;
#11573 = FACE_OUTER_BOUND ( 'NONE', #40374, .T. ) ;
#11574 = ORIENTED_EDGE ( 'NONE', *, *, #759, .T. ) ;
#11575 = CARTESIAN_POINT ( 'NONE',  ( -10.78898398081525301, -17.19290454168847404, 61.44271037915215317 ) ) ;
#11576 = CIRCLE ( 'NONE', #3705, 2.000000000000001332 ) ;
#11577 = FACE_OUTER_BOUND ( 'NONE', #20392, .T. ) ;
#11578 = CARTESIAN_POINT ( 'NONE',  ( -23.00454255336054743, -10.50046069577333441, 59.88731295783226471 ) ) ;
#11579 = ORIENTED_EDGE ( 'NONE', *, *, #45578, .T. ) ;
#11580 = CARTESIAN_POINT ( 'NONE',  ( -17.53144728931050977, -7.808750373270764378, 67.09209771269890155 ) ) ;
#11581 = EDGE_CURVE ( 'NONE', #6378, #4829, #39556, .T. ) ;
#11582 = ORIENTED_EDGE ( 'NONE', *, *, #40147, .T. ) ;
#11583 = CARTESIAN_POINT ( 'NONE',  ( -15.02405691534179688, -8.340062653448301333, 75.49999999999994316 ) ) ;
#11584 = CARTESIAN_POINT ( 'NONE',  ( -27.42409385541305511, -15.80920654474410725, 48.99999999999997868 ) ) ;
#11585 = ORIENTED_EDGE ( 'NONE', *, *, #216, .T. ) ;
#11586 = CARTESIAN_POINT ( 'NONE',  ( -17.59331746331979929, -7.761237803891376075, 63.55057029381061540 ) ) ;
#11587 = EDGE_CURVE ( 'NONE', #32492, #5613, #23095, .T. ) ;
#11588 = ADVANCED_FACE ( 'NONE', ( #20226 ), #23709, .T. ) ;
#11589 = CARTESIAN_POINT ( 'NONE',  ( -24.28579947082789303, -13.18942387424446316, 62.84736316175410309 ) ) ;
#11590 = CARTESIAN_POINT ( 'NONE',  ( -19.23659385650551457, -6.915538690918075382, 49.31353937987644542 ) ) ;
#11591 = DIRECTION ( 'NONE',  ( 0.6105870317843965500, 0.7919491628991826015, -6.540688078241514573E-08 ) ) ;
#11592 =( BOUNDED_CURVE ( )  B_SPLINE_CURVE ( 3, ( #14545, #14317, #6961, #43680 ),
 .UNSPECIFIED., .F., .F. ) 
 B_SPLINE_CURVE_WITH_KNOTS ( ( 4, 4 ),
 ( 0.5000000000000000000, 0.9074455897393657322 ),
 .UNSPECIFIED. ) 
 CURVE ( )  GEOMETRIC_REPRESENTATION_ITEM ( )  RATIONAL_B_SPLINE_CURVE ( ( 1.000000000000009326, 0.4567392136813359649, 0.3561768502900252154, 0.6983129098260869583 ) ) 
 REPRESENTATION_ITEM ( '' )  );
#11593 = CARTESIAN_POINT ( 'NONE',  ( -14.25068859620041017, -8.513811488652077486, 70.72957628655862550 ) ) ;
#11594 = DIRECTION ( 'NONE',  ( 1.000000000000000000, 2.866981220435666553E-17, 0.000000000000000000 ) ) ;
#11595 = ORIENTED_EDGE ( 'NONE', *, *, #29115, .F. ) ;
#11596 = CARTESIAN_POINT ( 'NONE',  ( -10.43689247203059267, -14.38509032613565530, 64.67338506919912788 ) ) ;
#11597 = CARTESIAN_POINT ( 'NONE',  ( -13.21599742097365038, -20.46930908964682416, 58.46138952334620598 ) ) ;
#11598 = EDGE_CURVE ( 'NONE', #44533, #3166, #4737, .T. ) ;
#11599 = CARTESIAN_POINT ( 'NONE',  ( -24.72409385541305582, -14.80920654474421028, 67.05882352941175384 ) ) ;
#11600 = CARTESIAN_POINT ( 'NONE',  ( -10.70566838141854404, -16.94585318031169763, 57.83760548748448116 ) ) ;
#11601 = CARTESIAN_POINT ( 'NONE',  ( -22.84886471163500588, -9.702775354051940582, 73.59665661135821324 ) ) ;
#11602 = EDGE_LOOP ( 'NONE', ( #462, #7937, #2165, #38914, #17821 ) ) ;
#11603 = ORIENTED_EDGE ( 'NONE', *, *, #21811, .T. ) ;
#11604 = CARTESIAN_POINT ( 'NONE',  ( -21.40186815114211782, -9.048699395220948460, 73.88512259465339582 ) ) ;
#11605 = CARTESIAN_POINT ( 'NONE',  ( -13.42648243792925378, -12.34047032955235679, 49.52966884056655772 ) ) ;
#11606 = ORIENTED_EDGE ( 'NONE', *, *, #48142, .F. ) ;
#11607 = CARTESIAN_POINT ( 'NONE',  ( -24.11267623503602664, -17.03798637408549155, 73.17776260608479788 ) ) ;
#11608 = DIRECTION ( 'NONE',  ( -1.000000000000000000, 4.164305804376849172E-17, -1.614929280266638808E-16 ) ) ;
#11609 = CARTESIAN_POINT ( 'NONE',  ( -11.65817609178158065, -18.77836167696750636, 64.93810149108783492 ) ) ;
#11610 = CARTESIAN_POINT ( 'NONE',  ( -17.20139249542113191, -7.812750000685961815, 70.49035839633111777 ) ) ;
#11611 = CARTESIAN_POINT ( 'NONE',  ( -23.59416455813390101, -18.98475620612148518, 65.96242875894608915 ) ) ;
#11612 =( BOUNDED_CURVE ( )  B_SPLINE_CURVE ( 3, ( #22938, #26128, #26614, #41140 ),
 .UNSPECIFIED., .F., .F. ) 
 B_SPLINE_CURVE_WITH_KNOTS ( ( 4, 4 ),
 ( 0.5000000000000000000, 0.9074455897393642889 ),
 .UNSPECIFIED. ) 
 CURVE ( )  GEOMETRIC_REPRESENTATION_ITEM ( )  RATIONAL_B_SPLINE_CURVE ( ( 1.000000000000009104, 0.4567392136813325232, 0.3561768502900241051, 0.6983129098260936196 ) ) 
 REPRESENTATION_ITEM ( '' )  );
#11613 = AXIS2_PLACEMENT_3D ( 'NONE', #18171, #21875, #13977 ) ;
#11614 = LINE ( 'NONE', #23434, #45243 ) ;
#11615 = AXIS2_PLACEMENT_3D ( 'NONE', #14685, #33177, #22870 ) ;
#11616 = CARTESIAN_POINT ( 'NONE',  ( -19.24190894175819366, -7.584296403803404196, 63.54593838833191910 ) ) ;
#11617 = EDGE_CURVE ( 'NONE', #30363, #24642, #37812, .T. ) ;
#11618 = DIRECTION ( 'NONE',  ( -3.071710424422018668E-17, 6.404604876783312462E-16, 1.000000000000000000 ) ) ;
#11619 = CARTESIAN_POINT ( 'NONE',  ( -16.36834455927873222, -22.18410795223847387, 61.94063518049016182 ) ) ;
#11620 = AXIS2_PLACEMENT_3D ( 'NONE', #44312, #18924, #25577 ) ;
#11621 = LINE ( 'NONE', #41663, #45270 ) ;
#11622 = CARTESIAN_POINT ( 'NONE',  ( -10.46944733747312917, -15.96661384539355133, 67.99239968927004441 ) ) ;
#11623 = CARTESIAN_POINT ( 'NONE',  ( -50.42409385541305511, -15.80920654474410725, 65.99999999999998579 ) ) ;
#11624 = VECTOR ( 'NONE', #20027, 1000.000000000000000 ) ;
#11625 = ORIENTED_EDGE ( 'NONE', *, *, #41319, .T. ) ;
#11626 = ORIENTED_EDGE ( 'NONE', *, *, #33440, .T. ) ;
#11627 = FILL_AREA_STYLE_COLOUR ( '', #36740 ) ;
#11628 = EDGE_LOOP ( 'NONE', ( #25185, #26338, #44454, #13420, #43539 ) ) ;
#11629 = CARTESIAN_POINT ( 'NONE',  ( -23.08659385541299969, -7.222650657624049231, 49.61879703869472280 ) ) ;
#11630 = CARTESIAN_POINT ( 'NONE',  ( -12.85799447202792045, -15.86467737382985632, 49.52966884056655772 ) ) ;
#11631 = DIRECTION ( 'NONE',  ( -5.731567514496413899E-31, -1.020425574103664789E-16, -1.000000000000000000 ) ) ;
#11632 = FACE_OUTER_BOUND ( 'NONE', #48423, .T. ) ;
#11633 = ORIENTED_EDGE ( 'NONE', *, *, #27277, .F. ) ;
#11634 = CARTESIAN_POINT ( 'NONE',  ( -13.41301606045583128, -21.08813317394188758, 65.17284274790917209 ) ) ;
#11635 = VECTOR ( 'NONE', #14750, 999.9999999999998863 ) ;
#11636 = CARTESIAN_POINT ( 'NONE',  ( -17.56018945634354722, -7.360327109558735259, 63.67244293056884175 ) ) ;
#11637 = VERTEX_POINT ( 'NONE', #34765 ) ;
#11638 = CARTESIAN_POINT ( 'NONE',  ( -10.63004074901718532, -12.92571453866564823, 67.75304464120749515 ) ) ;
#11639 = CARTESIAN_POINT ( 'NONE',  ( -20.69509153224808173, -8.115601224564374050, 63.49616927690831858 ) ) ;
#11640 = CIRCLE ( 'NONE', #686, 7.500000000000002665 ) ;
#11641 = CIRCLE ( 'NONE', #17910, 2.000000000000001332 ) ;
#11642 = ORIENTED_EDGE ( 'NONE', *, *, #40833, .T. ) ;
#11643 = CARTESIAN_POINT ( 'NONE',  ( -10.37095245282503342, -14.72771709220537240, 68.06620091705121922 ) ) ;
#11644 = DIRECTION ( 'NONE',  ( -0.2479245821708705444, -0.9687793358424813261, 9.885672099568325381E-17 ) ) ;
#11645 = CARTESIAN_POINT ( 'NONE',  ( -12.12786991918758339, -13.32596279628197600, 54.07175714974879099 ) ) ;
#11646 = ORIENTED_EDGE ( 'NONE', *, *, #46819, .F. ) ;
#11647 = CARTESIAN_POINT ( 'NONE',  ( -19.64493811714022087, -21.44926310044305851, 69.04555521092800063 ) ) ;
#11648 = EDGE_CURVE ( 'NONE', #10296, #26347, #6676, .T. ) ;
#11649 = CARTESIAN_POINT ( 'NONE',  ( -23.04402284766838349, -19.06632961612601918, 59.16938527523783620 ) ) ;
#11650 = B_SPLINE_CURVE_WITH_KNOTS ( 'NONE', 3,
 ( #10531, #39835, #13943, #44041, #13713, #47954, #28756, #35643, #46981, #1926 ),
 .UNSPECIFIED., .F., .F.,
 ( 4, 2, 2, 2, 4 ),
 ( 0.000000000000000000, 0.2500000000000000000, 0.5000000000000000000, 0.7500000000000000000, 1.000000000000000000 ),
 .UNSPECIFIED. ) ;
#11651 = AXIS2_PLACEMENT_3D ( 'NONE', #33009, #14291, #10868 ) ;
#11652 = CARTESIAN_POINT ( 'NONE',  ( -45.55409385541306477, -14.20920654474410760, 71.05212771298751306 ) ) ;
#11653 = DIRECTION ( 'NONE',  ( -0.9757441136919988711, -0.2189141945955433433, 0.000000000000000000 ) ) ;
#11654 = ORIENTED_EDGE ( 'NONE', *, *, #11242, .T. ) ;
#11655 = CARTESIAN_POINT ( 'NONE',  ( -24.69852180232685157, -16.41745880042978101, 59.30827708941524889 ) ) ;
#11656 = CARTESIAN_POINT ( 'NONE',  ( -10.99582178678916833, -11.91441492378913480, 74.85840195586327184 ) ) ;
#11657 = FACE_OUTER_BOUND ( 'NONE', #19495, .T. ) ;
#11658 = FACE_OUTER_BOUND ( 'NONE', #38400, .T. ) ;
#11659 = CARTESIAN_POINT ( 'NONE',  ( -23.91468471116454708, -11.15204413962362828, 70.09221953707209707 ) ) ;
#11660 = EDGE_CURVE ( 'NONE', #17355, #16961, #14714, .T. ) ;
#11661 = EDGE_CURVE ( 'NONE', #23333, #47654, #31740, .T. ) ;
#11662 = CARTESIAN_POINT ( 'NONE',  ( -22.17130234749883044, -20.55096496926394778, 58.87947491310501391 ) ) ;
#11663 = CARTESIAN_POINT ( 'NONE',  ( -18.47409385650551528, -9.792211528768504536, 50.49490371617623197 ) ) ;
#11665 = EDGE_CURVE ( 'NONE', #42290, #48213, #12707, .T. ) ;
#11664 = EDGE_LOOP ( 'NONE', ( #1195, #9184 ) ) ;
#11666 = LINE ( 'NONE', #34546, #18028 ) ;
#11667 = CARTESIAN_POINT ( 'NONE',  ( -20.38066051823377478, -10.47086428435309280, 49.52966884056655772 ) ) ;
#11668 = EDGE_LOOP ( 'NONE', ( #2166, #41367, #23327, #47134, #26423 ) ) ;
#11669 = DIRECTION ( 'NONE',  ( 1.000000000000000000, 0.000000000000000000, 1.927470528863119295E-16 ) ) ;
#11670 = EDGE_CURVE ( 'NONE', #13690, #28383, #6415, .T. ) ;
#11671 = LINE ( 'NONE', #15839, #34440 ) ;
#11672 = VERTEX_POINT ( 'NONE', #20486 ) ;
#11673 = CARTESIAN_POINT ( 'NONE',  ( -18.32857756213031664, -22.20418371868804996, 68.93019407337365578 ) ) ;
#11674 = CARTESIAN_POINT ( 'NONE',  ( -19.93798644100873574, -21.82225466599480157, 69.08482476138111394 ) ) ;
#11675 = CARTESIAN_POINT ( 'NONE',  ( -50.42609385541305755, -14.80920654474420139, 66.95294117647057419 ) ) ;
#11676 = ADVANCED_FACE ( 'NONE', ( #46820 ), #24423, .T. ) ;
#11677 = ORIENTED_EDGE ( 'NONE', *, *, #12140, .F. ) ;
#11678 = CARTESIAN_POINT ( 'NONE',  ( -13.18659385650551918, -9.302874398569244363, 51.68646062012417985 ) ) ;
#11679 = AXIS2_PLACEMENT_3D ( 'NONE', #34598, #15634, #26745 ) ;
#11680 = DIRECTION ( 'NONE',  ( 0.000000000000000000, 0.000000000000000000, 1.000000000000000000 ) ) ;
#11681 = AXIS2_PLACEMENT_3D ( 'NONE', #45740, #22578, #37834 ) ;
#11682 = CARTESIAN_POINT ( 'NONE',  ( -24.80663772805713307, -15.80987445113336776, 69.72581619873751890 ) ) ;
#11683 = CARTESIAN_POINT ( 'NONE',  ( -15.74783386771837890, -7.961078896070159061, 70.62461975990308360 ) ) ;
#11684 = CARTESIAN_POINT ( 'NONE',  ( -13.56513943501515840, -8.968887331962283938, 57.25502341335112533 ) ) ;
#11685 = TOROIDAL_SURFACE ( 'NONE', #17948, 1.999999999999999112, 1.249999999999999334 ) ;
#11686 = AXIS2_PLACEMENT_3D ( 'NONE', #19345, #23296, #11975 ) ;
#11687 = VERTEX_POINT ( 'NONE', #28356 ) ;
#11688 = ORIENTED_EDGE ( 'NONE', *, *, #35447, .F. ) ;
#11689 = CARTESIAN_POINT ( 'NONE',  ( -15.63659385650551670, -6.915538690918075382, 49.31353937987644542 ) ) ;
#11690 = CARTESIAN_POINT ( 'NONE',  ( -20.31649760022732565, -7.943510736669368910, 70.43595667626200907 ) ) ;
#11691 = CIRCLE ( 'NONE', #28976, 3.951441697420869481 ) ;
#11692 =( LENGTH_UNIT ( ) NAMED_UNIT ( * ) SI_UNIT ( .MILLI., .METRE. ) );
#11693 = CARTESIAN_POINT ( 'NONE',  ( -16.53659385650551528, -6.915538690918075382, 49.31353937987644542 ) ) ;
#11694 = B_SPLINE_CURVE_WITH_KNOTS ( 'NONE', 3,
 ( #22743, #4748, #15075, #19772, #11897, #15810, #4496, #11165, #30864, #26917 ),
 .UNSPECIFIED., .F., .F.,
 ( 4, 2, 2, 2, 4 ),
 ( 0.6272669072876895235, 0.7522669073072305590, 0.8772669073267717055, 1.002266907346312852, 1.127266907365853887 ),
 .UNSPECIFIED. ) ;
#11695 = CARTESIAN_POINT ( 'NONE',  ( -17.42409385541299471, -14.80920654474435771, 49.52966884056655772 ) ) ;
#11696 = CARTESIAN_POINT ( 'NONE',  ( -20.78299823145727387, -8.610459808214880439, 59.85597358678664648 ) ) ;
#11697 = CARTESIAN_POINT ( 'NONE',  ( -24.42401644153718721, -14.84212863923847081, 59.24300237020570137 ) ) ;
#11698 = DIRECTION ( 'NONE',  ( 0.000000000000000000, 1.000000000000000000, 0.000000000000000000 ) ) ;
#11699 = EDGE_CURVE ( 'NONE', #35489, #41576, #26847, .T. ) ;
#11700 = VERTEX_POINT ( 'NONE', #6429 ) ;
#11701 = CARTESIAN_POINT ( 'NONE',  ( -23.00382349513648350, -19.03821702553108253, 62.58236827718467765 ) ) ;
#11702 = ORIENTED_EDGE ( 'NONE', *, *, #8206, .F. ) ;
#11703 = CARTESIAN_POINT ( 'NONE',  ( -21.94242186726961208, -9.397052521110282441, 60.00699132926281010 ) ) ;
#11704 = CARTESIAN_POINT ( 'NONE',  ( -18.50931870666621037, -21.77518001355031529, 72.28510940651260341 ) ) ;
#11705 = CARTESIAN_POINT ( 'NONE',  ( -18.60148480518915548, -7.908490531605076868, 74.12447901480395274 ) ) ;
#11706 = DIRECTION ( 'NONE',  ( 0.6380325334150297456, -0.7700094066334507437, 1.806162864933161516E-16 ) ) ;
#11707 = EDGE_CURVE ( 'NONE', #32753, #14163, #253, .T. ) ;
#11708 = ORIENTED_EDGE ( 'NONE', *, *, #14758, .T. ) ;
#11709 = B_SPLINE_CURVE_WITH_KNOTS ( 'NONE', 1,
 ( #22051, #22531 ),
 .UNSPECIFIED., .F., .F.,
 ( 2, 2 ),
 ( 0.000000000000000000, 1.000000000000000000 ),
 .UNSPECIFIED. ) ;
#11710 = DIRECTION ( 'NONE',  ( 0.3224496555704363665, 0.8691421305882583992, -0.3749909018349775192 ) ) ;
#11711 = VECTOR ( 'NONE', #44206, 1000.000000000000114 ) ;
#11712 = CARTESIAN_POINT ( 'NONE',  ( -24.68759284454203851, -16.46579109868681812, 59.22358191938879202 ) ) ;
#11713 = FACE_OUTER_BOUND ( 'NONE', #44786, .T. ) ;
#11714 = CARTESIAN_POINT ( 'NONE',  ( -24.49266415654671292, -17.16299127166918126, 73.02189535998635961 ) ) ;
#11715 = ORIENTED_EDGE ( 'NONE', *, *, #43313, .T. ) ;
#11716 = CARTESIAN_POINT ( 'NONE',  ( -19.50843993236927432, -21.96177808838975665, 62.11008241541560437 ) ) ;
#11717 = DIRECTION ( 'NONE',  ( -1.000000000000000000, -1.665334536937734564E-16, -1.927470528863183637E-16 ) ) ;
#11718 = AXIS2_PLACEMENT_3D ( 'NONE', #25410, #2518, #48287 ) ;
#11719 = CARTESIAN_POINT ( 'NONE',  ( -23.48344415125163565, -18.41350569598871090, 73.04896097104848707 ) ) ;
#11720 = CARTESIAN_POINT ( 'NONE',  ( -12.79725882921341373, -20.12850138265567068, 72.10653676770067477 ) ) ;
#11721 = APPLICATION_PROTOCOL_DEFINITION ( 'draft international standard', 'automotive_design', 1998, #4536 ) ;
#11722 = ORIENTED_EDGE ( 'NONE', *, *, #22600, .T. ) ;
#11723 = CARTESIAN_POINT ( 'NONE',  ( -17.79084007069931417, -7.768752218527304798, 60.38060768310334225 ) ) ;
#11724 = CARTESIAN_POINT ( 'NONE',  ( -18.34656657831649085, -21.80233790260681204, 65.34532039249234003 ) ) ;
#11725 = CARTESIAN_POINT ( 'NONE',  ( -23.04635137988585214, -19.07596084359022726, 65.96822594231640835 ) ) ;
#11726 = EDGE_CURVE ( 'NONE', #35202, #313, #34221, .T. ) ;
#11727 = CARTESIAN_POINT ( 'NONE',  ( -21.31115985637654120, -8.927249709250721921, 73.88656608925673197 ) ) ;
#11728 = ORIENTED_EDGE ( 'NONE', *, *, #405, .T. ) ;
#11729 = DIRECTION ( 'NONE',  ( 1.927470528863184130E-16, 1.434740771370715221E-29, -1.000000000000000000 ) ) ;
#11730 = VECTOR ( 'NONE', #1414, 1000.000000000000000 ) ;
#11731 = EDGE_CURVE ( 'NONE', #45977, #18743, #5939, .T. ) ;
#11732 = VERTEX_POINT ( 'NONE', #39668 ) ;
#11733 = CARTESIAN_POINT ( 'NONE',  ( -19.00548271871079464, -7.528979306145422434, 67.05071780787497460 ) ) ;
#11734 = CARTESIAN_POINT ( 'NONE',  ( -19.81920524125959560, -24.16823983354497685, 54.50428052266512680 ) ) ;
#11735 = CARTESIAN_POINT ( 'NONE',  ( -11.93195840498443516, -10.38844327383712773, 70.98365212470247343 ) ) ;
#11736 = ORIENTED_EDGE ( 'NONE', *, *, #452, .T. ) ;
#11737 = EDGE_CURVE ( 'NONE', #17592, #38583, #15472, .T. ) ;
#11738 = CARTESIAN_POINT ( 'NONE',  ( -10.95381465013825206, -17.48043978162002077, 68.39721944380028162 ) ) ;
#11739 = ORIENTED_EDGE ( 'NONE', *, *, #17645, .F. ) ;
#11740 = ORIENTED_EDGE ( 'NONE', *, *, #36457, .T. ) ;
#11741 = VERTEX_POINT ( 'NONE', #21203 ) ;
#11742 = CARTESIAN_POINT ( 'NONE',  ( -15.14815771252334820, -21.49015593068176244, 72.19008430323151515 ) ) ;
#11743 = CARTESIAN_POINT ( 'NONE',  ( -28.42409385541305511, -6.359206544744109735, 47.99999999999997868 ) ) ;
#11744 = CARTESIAN_POINT ( 'NONE',  ( -21.21846785720043727, -20.69168585734932719, 69.06952566980361041 ) ) ;
#11746 = ADVANCED_FACE ( 'NONE', ( #36203 ), #2485, .T. ) ;
#11745 = DIRECTION ( 'NONE',  ( -3.071710424422018668E-17, 6.404604876783312462E-16, 1.000000000000000000 ) ) ;
#11747 =( BOUNDED_CURVE ( )  B_SPLINE_CURVE ( 3, ( #32389, #28683, #36301, #25241 ),
 .UNSPECIFIED., .F., .F. ) 
 B_SPLINE_CURVE_WITH_KNOTS ( ( 4, 4 ),
 ( 0.9074455897393632897, 1.000000000000000000 ),
 .UNSPECIFIED. ) 
 CURVE ( )  GEOMETRIC_REPRESENTATION_ITEM ( )  RATIONAL_B_SPLINE_CURVE ( ( 0.6983129098260791867, 0.7760317562606862118, 0.8765941196519931866, 1.000000000000000000 ) ) 
 REPRESENTATION_ITEM ( '' )  );
#11748 = CARTESIAN_POINT ( 'NONE',  ( -10.39923015370485260, -17.29004932004441031, 61.35017275334070064 ) ) ;
#11749 = CARTESIAN_POINT ( 'NONE',  ( -14.16804751454036726, -8.612086832270765768, 74.21571240128525915 ) ) ;
#11750 = CARTESIAN_POINT ( 'NONE',  ( -10.51251092892767325, -16.19956264364908449, 71.44750414188726495 ) ) ;
#11751 = ORIENTED_EDGE ( 'NONE', *, *, #13012, .F. ) ;
#11752 = ORIENTED_EDGE ( 'NONE', *, *, #5206, .F. ) ;
#11753 = CARTESIAN_POINT ( 'NONE',  ( -12.03835690272354597, -15.98895779851376631, 53.69233794759168887 ) ) ;
#11754 = CARTESIAN_POINT ( 'NONE',  ( -22.51947191901838963, -20.24425718459050572, 65.80398109777289051 ) ) ;
#11755 = VECTOR ( 'NONE', #15213, 1000.000000000000114 ) ;
#11756 = CARTESIAN_POINT ( 'NONE',  ( -10.50673402251998390, -15.88996810048886488, 68.20597793203801018 ) ) ;
#11757 = CARTESIAN_POINT ( 'NONE',  ( -23.69928304873747038, -18.82488403301566038, 69.33726028187463442 ) ) ;
#11758 = ORIENTED_EDGE ( 'NONE', *, *, #23410, .T. ) ;
#11759 =( BOUNDED_SURFACE ( )  B_SPLINE_SURFACE ( 3, 1, ( 
 ( #35968, #47789 ),
 ( #6671, #24907 ),
 ( #6189, #43878 ),
 ( #7172, #32990 ),
 ( #48032, #33976 ),
 ( #44356, #14270 ),
 ( #26607, #18221 ) ),
 .UNSPECIFIED., .T., .F., .F. ) 
 B_SPLINE_SURFACE_WITH_KNOTS ( ( 4, 3, 4 ),
 ( 2, 2 ),
 ( 0.000000000000000000, 0.5000000000000000000, 1.000000000000000000 ),
 ( 0.000000000000000000, 1.000000000000000000 ),
 .UNSPECIFIED. ) 
 GEOMETRIC_REPRESENTATION_ITEM ( )  RATIONAL_B_SPLINE_SURFACE ( (
 ( 1.000000000000000000, 1.000000000000000000),
 ( 0.3333333333333335369, 0.3333333333333330373),
 ( 0.3333333333333335369, 0.3333333333333330373),
 ( 1.000000000000000000, 1.000000000000000000),
 ( 0.3333333333333333703, 0.3333333333333333703),
 ( 0.3333333333333333703, 0.3333333333333333703),
 ( 1.000000000000000000, 1.000000000000000000) ) ) 
 REPRESENTATION_ITEM ( '' )  SURFACE ( )  );
#11760 = CARTESIAN_POINT ( 'NONE',  ( -16.84284385650551741, -8.811426318492348031, 52.18089403414752070 ) ) ;
#11761 =( BOUNDED_CURVE ( )  B_SPLINE_CURVE ( 3, ( #45325, #25865, #14500, #34214 ),
 .UNSPECIFIED., .F., .F. ) 
 B_SPLINE_CURVE_WITH_KNOTS ( ( 4, 4 ),
 ( 0.5000000000000000000, 0.9074455897393687298 ),
 .UNSPECIFIED. ) 
 CURVE ( )  GEOMETRIC_REPRESENTATION_ITEM ( )  RATIONAL_B_SPLINE_CURVE ( ( 1.000000000000004219, 0.4567392136813255288, 0.3561768502900249378, 0.6983129098261068313 ) ) 
 REPRESENTATION_ITEM ( '' )  );
#11762 = VECTOR ( 'NONE', #15652, 1000.000000000000000 ) ;
#11763 = AXIS2_PLACEMENT_3D ( 'NONE', #46793, #28328, #9623 ) ;
#11764 = VERTEX_POINT ( 'NONE', #17722 ) ;
#11765 = CARTESIAN_POINT ( 'NONE',  ( -16.12973315643056793, -21.68894210253334975, 58.56969077390900225 ) ) ;
#11766 = CARTESIAN_POINT ( 'NONE',  ( -12.10487669921564446, -20.02548830339394925, 61.44032727821130635 ) ) ;
#11767 = CARTESIAN_POINT ( 'NONE',  ( -15.26068139326780226, -21.46662260714567694, 68.57592932306751266 ) ) ;
#11768 = AXIS2_PLACEMENT_3D ( 'NONE', #2276, #20752, #5970 ) ;
#11769 = EDGE_CURVE ( 'NONE', #33284, #36353, #7984, .T. ) ;
#11770 = ORIENTED_EDGE ( 'NONE', *, *, #38313, .T. ) ;
#11771 = DIRECTION ( 'NONE',  ( -3.071710424422018668E-17, 6.404604876783312462E-16, 1.000000000000000000 ) ) ;
#11772 =( BOUNDED_CURVE ( )  B_SPLINE_CURVE ( 3, ( #46169, #22804, #8499, #41751 ),
 .UNSPECIFIED., .F., .F. ) 
 B_SPLINE_CURVE_WITH_KNOTS ( ( 4, 4 ),
 ( 0.4074455897393650661, 0.5000000000000000000 ),
 .UNSPECIFIED. ) 
 CURVE ( )  GEOMETRIC_REPRESENTATION_ITEM ( )  RATIONAL_B_SPLINE_CURVE ( ( 0.6983129098260983936, 0.7760317562607078612, 0.8765941196520097289, 1.000000000000007772 ) ) 
 REPRESENTATION_ITEM ( '' )  );
#11773 = CARTESIAN_POINT ( 'NONE',  ( -10.64854695470030599, -12.86019059820356780, 64.55364013863997741 ) ) ;
#11774 = CARTESIAN_POINT ( 'NONE',  ( -17.79490377976783932, -14.65920654474411045, 47.99999999999998579 ) ) ;
#11775 = ORIENTED_EDGE ( 'NONE', *, *, #30232, .F. ) ;
#11776 = CARTESIAN_POINT ( 'NONE',  ( -15.55171133418867235, -7.598245370416885969, 70.79485226425863686 ) ) ;
#11777 = CARTESIAN_POINT ( 'NONE',  ( -18.36828968083242231, -10.20659317963780843, 52.02966884056656482 ) ) ;
#11778 = DIRECTION ( 'NONE',  ( -0.8603395911234869020, -0.5097212845717467022, 0.000000000000000000 ) ) ;
#11779 = VERTEX_POINT ( 'NONE', #13780 ) ;
#11780 = FACE_OUTER_BOUND ( 'NONE', #32019, .T. ) ;
#11781 = ORIENTED_EDGE ( 'NONE', *, *, #36272, .T. ) ;
#11782 = CARTESIAN_POINT ( 'NONE',  ( -18.18338144371267617, -21.81849904615365432, 65.63060065626805795 ) ) ;
#11783 = CARTESIAN_POINT ( 'NONE',  ( -23.84607668508775902, -11.89174505508500523, 63.04398307482357922 ) ) ;
#11784 = ORIENTED_EDGE ( 'NONE', *, *, #3328, .T. ) ;
#11785 = CARTESIAN_POINT ( 'NONE',  ( -24.38756562526642213, -15.91227465074931935, 66.34852784166324113 ) ) ;
#11786 = CARTESIAN_POINT ( 'NONE',  ( -18.24929096724884658, -21.81104555038653103, 68.82986815895560540 ) ) ;
#11787 = CARTESIAN_POINT ( 'NONE',  ( -10.96069643151774109, -18.51437482595545347, 57.92219192461608657 ) ) ;
#11788 = ADVANCED_FACE ( 'NONE', ( #44114 ), #21916, .T. ) ;
#11789 = AXIS2_PLACEMENT_3D ( 'NONE', #16349, #31384, #7239 ) ;
#11790 = ORIENTED_EDGE ( 'NONE', *, *, #29379, .T. ) ;
#11791 = DIRECTION ( 'NONE',  ( -0.8705373987491421550, 0.4921022631314296847, -4.758021987662797425E-08 ) ) ;
#11792 = EDGE_CURVE ( 'NONE', #5421, #37170, #6062, .T. ) ;
#11793 = CARTESIAN_POINT ( 'NONE',  ( -16.27008412796014625, -7.904986034540439022, 60.20028479263386600 ) ) ;
#11794 = CARTESIAN_POINT ( 'NONE',  ( -11.42427419758796603, -11.20335516203438075, 57.31789115431045190 ) ) ;
#11795 = ORIENTED_EDGE ( 'NONE', *, *, #34420, .T. ) ;
#11796 = CARTESIAN_POINT ( 'NONE',  ( -17.13503149044196761, -7.764836982087094164, 70.77563787455143540 ) ) ;
#11797 = AXIS2_PLACEMENT_3D ( 'NONE', #26519, #30472, #44763 ) ;
#11798 = EDGE_CURVE ( 'NONE', #19293, #32931, #31440, .T. ) ;
#11799 = CARTESIAN_POINT ( 'NONE',  ( -23.29054614595685635, -19.40156175341775580, 59.04557170734604199 ) ) ;
#11800 = ORIENTED_EDGE ( 'NONE', *, *, #48385, .F. ) ;
#11801 = VERTEX_POINT ( 'NONE', #40618 ) ;
#11802 = DIRECTION ( 'NONE',  ( 1.224646799147353207E-16, 1.000000000000000000, -1.912410701131276611E-32 ) ) ;
#11803 = FACE_OUTER_BOUND ( 'NONE', #24406, .T. ) ;
#11804 = CARTESIAN_POINT ( 'NONE',  ( -23.42532394183187705, -19.22384306421519184, 62.46911594462533657 ) ) ;
#11805 = EDGE_CURVE ( 'NONE', #20388, #40396, #15820, .T. ) ;
#11806 = CARTESIAN_POINT ( 'NONE',  ( -20.94909385650551670, -8.104110260919577868, 48.81699501597546487 ) ) ;
#11807 = DIRECTION ( 'NONE',  ( 3.071710424422018668E-17, -6.404604876783312462E-16, -1.000000000000000000 ) ) ;
#11808 = CARTESIAN_POINT ( 'NONE',  ( -11.55573855159262386, -10.21941529800896653, 71.15388400389697665 ) ) ;
#11809 = CARTESIAN_POINT ( 'NONE',  ( -23.88368001943721453, -17.64091657838220328, 66.35845829618112646 ) ) ;
#11810 = DIRECTION ( 'NONE',  ( 1.224646799147353207E-16, 1.000000000000000000, -1.912410701131276611E-32 ) ) ;
#11811 = ORIENTED_EDGE ( 'NONE', *, *, #32166, .T. ) ;
#11812 = FACE_OUTER_BOUND ( 'NONE', #37002, .T. ) ;
#11813 = CARTESIAN_POINT ( 'NONE',  ( -15.58636089855801110, -7.589425593079765164, 70.75989837095031021 ) ) ;
#11814 = CARTESIAN_POINT ( 'NONE',  ( -15.09544305450467760, -21.46351983957133669, 65.40596681500470311 ) ) ;
#11815 = EDGE_CURVE ( 'NONE', #13312, #15919, #33968, .T. ) ;
#11816 = EDGE_LOOP ( 'NONE', ( #27106, #44018, #23822, #30270, #33391 ) ) ;
#11817 = EDGE_CURVE ( 'NONE', #20357, #29883, #7881, .T. ) ;
#11818 = ORIENTED_EDGE ( 'NONE', *, *, #35791, .T. ) ;
#11819 = EDGE_CURVE ( 'NONE', #8067, #44791, #41919, .T. ) ;
#11820 = CARTESIAN_POINT ( 'NONE',  ( -19.87969377733951859, -21.36436553174173270, 69.19822862580041090 ) ) ;
#11821 = CYLINDRICAL_SURFACE ( 'NONE', #42592, 0.1500000000000009104 ) ;
#11822 = AXIS2_PLACEMENT_3D ( 'NONE', #20378, #10267, #6320 ) ;
#11823 = CARTESIAN_POINT ( 'NONE',  ( -24.72409385541305582, -14.80920654474411613, 58.90588235294116970 ) ) ;
#11824 = CARTESIAN_POINT ( 'NONE',  ( -15.09909385541304516, -8.105421454601382081, 49.25000573077640809 ) ) ;
#11825 = ADVANCED_FACE ( 'NONE', ( #26108 ), #45083, .T. ) ;
#11826 = ORIENTED_EDGE ( 'NONE', *, *, #10601, .T. ) ;
#11827 = AXIS2_PLACEMENT_3D ( 'NONE', #8733, #15850, #23261 ) ;
#11828 = CARTESIAN_POINT ( 'NONE',  ( -13.11378388673462148, -9.291622923581300597, 70.95998485332185624 ) ) ;
#11829 = LINE ( 'NONE', #37661, #8419 ) ;
#11830 = ORIENTED_EDGE ( 'NONE', *, *, #2708, .T. ) ;
#11831 = CIRCLE ( 'NONE', #29121, 6.999999999999999112 ) ;
#11832 = DIRECTION ( 'NONE',  ( 0.000000000000000000, 0.000000000000000000, 1.000000000000000000 ) ) ;
#11833 = CARTESIAN_POINT ( 'NONE',  ( -14.01837044221388595, -8.636059239884618322, 74.48482605064899076 ) ) ;
#11834 = ORIENTED_EDGE ( 'NONE', *, *, #6759, .F. ) ;
#11835 = DIRECTION ( 'NONE',  ( 1.224646799147353207E-16, 1.000000000000000000, -1.912410701131276611E-32 ) ) ;
#11836 = ORIENTED_EDGE ( 'NONE', *, *, #34768, .F. ) ;
#11837 = CARTESIAN_POINT ( 'NONE',  ( -24.72409385541305582, -14.90920654474419038, 65.04705882352939739 ) ) ;
#11838 = DIRECTION ( 'NONE',  ( -6.059369603295153624E-06, 3.309764060044371102E-06, 0.9999999999761648439 ) ) ;
#11839 = VERTEX_POINT ( 'NONE', #3948 ) ;
#11840 = CARTESIAN_POINT ( 'NONE',  ( -24.43112999227502513, -15.58634490091466951, 73.00303748142292193 ) ) ;
#11841 = CARTESIAN_POINT ( 'NONE',  ( -10.13784000599894597, -13.25541019000276499, 74.79322239981686948 ) ) ;
#11842 = CLOSED_SHELL ( 'NONE', ( #14405, #27267, #11947, #1056, #10901, #47344, #43346, #26441, #5877, #10313, #29245, #28891, #24227, #7452, #26996, #48492, #8860, #39497, #1467, #41355, #31308, #8267, #17385, #36199, #41468, #44530, #40702, #10621, #42822, #9575, #1377, #43250, #9713, #45573, #28078, #8950, #3781, #27630, #18459, #14956, #18440, #46651, #33775, #3536, #2112, #17095, #10552, #38064, #38343, #8251, #24487, #11156, #25373, #21876, #37241, #16412, #948, #30034, #6349, #10087, #41112, #8579, #41596, #41675, #7168, #1350, #20948, #62, #21700, #7900, #5053, #16438, #34418, #11089, #2334, #6329, #667, #22105, #27508, #31787, #17796, #35593, #47613, #9013, #34960 ) ) ;
#11843 = CARTESIAN_POINT ( 'NONE',  ( -16.03034385650551386, -9.794322478646142471, 51.19202720610083190 ) ) ;
#11844 = B_SPLINE_CURVE_WITH_KNOTS ( 'NONE', 3,
 ( #8279, #37554, #30934, #48655, #14897, #18864, #29957, #33875, #26499, #38284 ),
 .UNSPECIFIED., .F., .F.,
 ( 4, 2, 2, 2, 4 ),
 ( 0.000000000000000000, 0.2500000000000000000, 0.5000000000000000000, 0.7500000000000000000, 1.000000000000000000 ),
 .UNSPECIFIED. ) ;
#11845 = CARTESIAN_POINT ( 'NONE',  ( -17.82745659574447927, -7.820727410278355940, 60.08060779106381233 ) ) ;
#11846 =( BOUNDED_CURVE ( )  B_SPLINE_CURVE ( 3, ( #10853, #44364, #10617, #40641 ),
 .UNSPECIFIED., .F., .F. ) 
 B_SPLINE_CURVE_WITH_KNOTS ( ( 4, 4 ),
 ( 0.4074455897393681747, 0.5000000000000000000 ),
 .UNSPECIFIED. ) 
 CURVE ( )  GEOMETRIC_REPRESENTATION_ITEM ( )  RATIONAL_B_SPLINE_CURVE ( ( 0.6983129098260796308, 0.7760317562606730002, 0.8765941196519756451, 0.9999999999999783507 ) ) 
 REPRESENTATION_ITEM ( '' )  );
#11847 = CARTESIAN_POINT ( 'NONE',  ( -22.27236978094073550, -9.152572242100493582, 59.82897054759915534 ) ) ;
#11848 = CARTESIAN_POINT ( 'NONE',  ( -13.35550429318260512, -8.568184490765622385, 57.15463139269148485 ) ) ;
#11849 = ORIENTED_EDGE ( 'NONE', *, *, #23132, .T. ) ;
#11850 = CARTESIAN_POINT ( 'NONE',  ( -13.55325570056783491, -20.70509005021970594, 57.93161203092463296 ) ) ;
#11851 = CYLINDRICAL_SURFACE ( 'NONE', #36002, 1.249999999999999334 ) ;
#11852 = EDGE_CURVE ( 'NONE', #8811, #1752, #10835, .T. ) ;
#11853 = CARTESIAN_POINT ( 'NONE',  ( -45.92409385541306222, -17.80920654474411435, 69.25000000000000000 ) ) ;
#11854 = CARTESIAN_POINT ( 'NONE',  ( -16.02413508665766528, -7.899451961642459885, 63.96451206367848386 ) ) ;
#11855 = ORIENTED_EDGE ( 'NONE', *, *, #18721, .T. ) ;
#11856 = EDGE_LOOP ( 'NONE', ( #4351, #47648, #39779, #3643, #12852 ) ) ;
#11857 = EDGE_CURVE ( 'NONE', #19458, #14528, #27182, .T. ) ;
#11858 = CARTESIAN_POINT ( 'NONE',  ( -18.53202070066404517, -7.846807721809618386, 73.84064401782792686 ) ) ;
#11859 = CARTESIAN_POINT ( 'NONE',  ( -23.94755663202570517, -8.431048274511610430, 54.44843099904676365 ) ) ;
#11860 = VERTEX_POINT ( 'NONE', #18960 ) ;
#11861 = CARTESIAN_POINT ( 'NONE',  ( -21.04510527405784970, -21.32003654990205987, 62.31460175905966992 ) ) ;
#11862 = CARTESIAN_POINT ( 'NONE',  ( -15.22116837037893866, -21.50650591823945845, 68.59065000974109694 ) ) ;
#11863 = CARTESIAN_POINT ( 'NONE',  ( -22.04909385759799179, -8.112991634885936776, 51.74999426922421719 ) ) ;
#11864 = CARTESIAN_POINT ( 'NONE',  ( -17.27965087796144061, -7.810258999111470146, 70.50652427083761609 ) ) ;
#11865 = CARTESIAN_POINT ( 'NONE',  ( -14.22586362203780652, -8.080537296073694975, 67.30329176109222544 ) ) ;
#11866 = CARTESIAN_POINT ( 'NONE',  ( -11.26201241829012822, -11.37794026804562009, 68.03353368067536167 ) ) ;
#11867 = VECTOR ( 'NONE', #448, 1000.000000000000114 ) ;
#11868 = DIRECTION ( 'NONE',  ( -3.071710424422018668E-17, 6.404604876783312462E-16, 1.000000000000000000 ) ) ;
#11869 = CARTESIAN_POINT ( 'NONE',  ( -10.02759501504927186, -15.70053000738341709, 61.13765413890485689 ) ) ;
#11870 = CYLINDRICAL_SURFACE ( 'NONE', #1474, 5.249999999999998224 ) ;
#11871 = AXIS2_PLACEMENT_3D ( 'NONE', #43987, #36784, #29924 ) ;
#11872 = CARTESIAN_POINT ( 'NONE',  ( -16.45566506110110438, -21.79267588865899086, 62.04095995016087528 ) ) ;
#11873 = FACE_OUTER_BOUND ( 'NONE', #29538, .T. ) ;
#11874 = CARTESIAN_POINT ( 'NONE',  ( -12.71689648175658149, -19.99233235212643223, 71.91726715478147014 ) ) ;
#11875 = CARTESIAN_POINT ( 'NONE',  ( -23.82284107231174630, -10.99348899561931781, 73.61839243124092036 ) ) ;
#11877 = ORIENTED_EDGE ( 'NONE', *, *, #34087, .F. ) ;
#11876 = EDGE_CURVE ( 'NONE', #47620, #36414, #7157, .T. ) ;
#11878 = ORIENTED_EDGE ( 'NONE', *, *, #16958, .T. ) ;
#11879 = CARTESIAN_POINT ( 'NONE',  ( -20.16542227925740249, -21.73660035250202327, 72.44832829956453679 ) ) ;
#11880 = ORIENTED_EDGE ( 'NONE', *, *, #3403, .F. ) ;
#11881 = EDGE_CURVE ( 'NONE', #1976, #31856, #7223, .T. ) ;
#11882 = EDGE_CURVE ( 'NONE', #24162, #15992, #24225, .T. ) ;
#11883 = ADVANCED_FACE ( 'NONE', ( #33707 ), #26709, .T. ) ;
#11884 = CARTESIAN_POINT ( 'NONE',  ( -21.35673258969865174, -10.96416394607318701, 54.07175714974879099 ) ) ;
#11885 = B_SPLINE_CURVE_WITH_KNOTS ( 'NONE', 1,
 ( #5066, #11971 ),
 .UNSPECIFIED., .F., .F.,
 ( 2, 2 ),
 ( 0.000000000000000000, 1.000000000000000000 ),
 .UNSPECIFIED. ) ;
#11886 = AXIS2_PLACEMENT_3D ( 'NONE', #18899, #13956, #44053 ) ;
#11887 = DIRECTION ( 'NONE',  ( -0.5497669574358330369, 0.8353180786453389128, 7.898837271846008747E-08 ) ) ;
#11888 = CARTESIAN_POINT ( 'NONE',  ( -16.07923611736888603, -22.13698717359939039, 58.42552246658256365 ) ) ;
#11889 = ORIENTED_EDGE ( 'NONE', *, *, #4368, .T. ) ;
#11890 = VECTOR ( 'NONE', #41582, 1000.000000000000227 ) ;
#11891 = CARTESIAN_POINT ( 'NONE',  ( -13.76968405657925487, -21.30219918833402204, 72.11263056552699879 ) ) ;
#11892 = DIRECTION ( 'NONE',  ( 3.413470714839332458E-33, -1.190614954331866791E-16, 1.000000000000000000 ) ) ;
#11893 = ORIENTED_EDGE ( 'NONE', *, *, #1997, .T. ) ;
#11894 =( BOUNDED_SURFACE ( )  B_SPLINE_SURFACE ( 3, 1, ( 
 ( #25469, #28918 ),
 ( #21051, #2335 ),
 ( #21772, #40258 ),
 ( #13152, #47639 ),
 ( #39522, #17814 ),
 ( #24989, #6522 ),
 ( #13874, #2580 ) ),
 .UNSPECIFIED., .T., .F., .F. ) 
 B_SPLINE_SURFACE_WITH_KNOTS ( ( 4, 3, 4 ),
 ( 2, 2 ),
 ( 0.000000000000000000, 0.5000000000000000000, 1.000000000000000000 ),
 ( 0.000000000000000000, 1.000000000000000000 ),
 .UNSPECIFIED. ) 
 GEOMETRIC_REPRESENTATION_ITEM ( )  RATIONAL_B_SPLINE_SURFACE ( (
 ( 1.000000000000000000, 1.000000000000000000),
 ( 0.3333333333333335369, 0.3333333333333330373),
 ( 0.3333333333333335369, 0.3333333333333330373),
 ( 1.000000000000000000, 1.000000000000000000),
 ( 0.3333333333333333703, 0.3333333333333333703),
 ( 0.3333333333333333703, 0.3333333333333333703),
 ( 1.000000000000000000, 1.000000000000000000) ) ) 
 REPRESENTATION_ITEM ( '' )  SURFACE ( )  );
#11895 = CARTESIAN_POINT ( 'NONE',  ( -10.82281284296662527, -12.48008513829669575, 57.62857332801928578 ) ) ;
#11896 = AXIS2_PLACEMENT_3D ( 'NONE', #48152, #6063, #47439 ) ;
#11897 = CARTESIAN_POINT ( 'NONE',  ( -12.25935330346987051, -20.17854375260402477, 64.98862157977991671 ) ) ;
#11898 = ORIENTED_EDGE ( 'NONE', *, *, #9751, .T. ) ;
#11899 = B_SPLINE_CURVE_WITH_KNOTS ( 'NONE', 1,
 ( #40714, #26195 ),
 .UNSPECIFIED., .F., .F.,
 ( 2, 2 ),
 ( 0.000000000000000000, 1.000000000000000000 ),
 .UNSPECIFIED. ) ;
#11900 = CARTESIAN_POINT ( 'NONE',  ( -11.11596100489605199, -10.84561087226838794, 57.40891979410004353 ) ) ;
#11901 = CARTESIAN_POINT ( 'NONE',  ( -17.11809369177854379, -21.86054179209348192, 68.85127668957714775 ) ) ;
#11902 = CARTESIAN_POINT ( 'NONE',  ( -23.42532328873747005, -19.22384396101403681, 62.46911485589509994 ) ) ;
#11903 = ORIENTED_EDGE ( 'NONE', *, *, #36367, .F. ) ;
#11904 = DIRECTION ( 'NONE',  ( -3.071710424422018668E-17, 6.404604876783312462E-16, 1.000000000000000000 ) ) ;
#11905 = EDGE_CURVE ( 'NONE', #3501, #27387, #21392, .T. ) ;
#11906 = DIRECTION ( 'NONE',  ( -3.413470714839332458E-33, 1.190614954331866791E-16, -1.000000000000000000 ) ) ;
#11907 = B_SPLINE_CURVE_WITH_KNOTS ( 'NONE', 3,
 ( #12650, #24233, #31853, #38751, #1312, #45911, #12168, #38247, #39239, #5519 ),
 .UNSPECIFIED., .F., .F.,
 ( 4, 2, 2, 2, 4 ),
 ( 0.1272669073658447836, 0.2522669073463343903, 0.3772669073268239970, 0.5022669073073136037, 0.6272669072878032104 ),
 .UNSPECIFIED. ) ;
#11908 = CARTESIAN_POINT ( 'NONE',  ( -41.28806444364835215, -14.80920654474410725, 72.08823529411763786 ) ) ;
#11909 = DIRECTION ( 'NONE',  ( 0.000000000000000000, 0.000000000000000000, -1.000000000000000000 ) ) ;
#11910 = VERTEX_POINT ( 'NONE', #23643 ) ;
#11911 = CARTESIAN_POINT ( 'NONE',  ( -24.38391064099431915, -14.06024038319858960, 73.42271507915008044 ) ) ;
#11913 =( BOUNDED_CURVE ( )  B_SPLINE_CURVE ( 3, ( #20796, #5295, #9957, #12675 ),
 .UNSPECIFIED., .F., .F. ) 
 B_SPLINE_CURVE_WITH_KNOTS ( ( 4, 4 ),
 ( 0.9074455897393701731, 1.000000000000000000 ),
 .UNSPECIFIED. ) 
 CURVE ( )  GEOMETRIC_REPRESENTATION_ITEM ( )  RATIONAL_B_SPLINE_CURVE ( ( 0.6983129098261042778, 0.7760317562607079722, 0.8765941196520065093, 1.000000000000000000 ) ) 
 REPRESENTATION_ITEM ( '' )  );
#11912 = LINE ( 'NONE', #4508, #11339 ) ;
#11914 = CARTESIAN_POINT ( 'NONE',  ( -23.92296941035127844, -11.16669991615614066, 70.08549063249201083 ) ) ;
#11915 = CARTESIAN_POINT ( 'NONE',  ( -8.424093855413063991, -8.109206544744111511, 49.24999999999999289 ) ) ;
#11916 = CARTESIAN_POINT ( 'NONE',  ( -20.72409385650551883, -6.426201560718812544, 50.50509628382439331 ) ) ;
#11917 = VECTOR ( 'NONE', #8046, 1000.000000000000000 ) ;
#11918 = ORIENTED_EDGE ( 'NONE', *, *, #47095, .T. ) ;
#11919 = EDGE_CURVE ( 'NONE', #32734, #41576, #3246, .T. ) ;
#11920 = CARTESIAN_POINT ( 'NONE',  ( -21.57995947450667984, -9.113990939708573435, 70.14604673427196246 ) ) ;
#11921 = CARTESIAN_POINT ( 'NONE',  ( -15.75283589881223278, -7.548994832054173543, 67.32502661251716347 ) ) ;
#11922 = ORIENTED_EDGE ( 'NONE', *, *, #44238, .T. ) ;
#11923 = CARTESIAN_POINT ( 'NONE',  ( -24.38756562526642213, -15.91227465074931935, 66.34852784166324113 ) ) ;
#11924 = CARTESIAN_POINT ( 'NONE',  ( -12.78399838166839686, -20.05042309268234391, 68.40945562133974533 ) ) ;
#11925 = CARTESIAN_POINT ( 'NONE',  ( -18.62860737289870983, -7.457144689169211027, 74.09710349057253609 ) ) ;
#11926 = ORIENTED_EDGE ( 'NONE', *, *, #216, .F. ) ;
#11927 = DIRECTION ( 'NONE',  ( -0.6380325334150243055, 0.7700094066334552956, 2.346882832748419528E-17 ) ) ;
#11928 = CYLINDRICAL_SURFACE ( 'NONE', #41446, 0.1500000000000022704 ) ;
#11929 = VECTOR ( 'NONE', #23036, 1000.000000000000114 ) ;
#11930 = CARTESIAN_POINT ( 'NONE',  ( -14.86627107493491984, -7.811969877679347363, 56.96504568426624360 ) ) ;
#11931 = ORIENTED_EDGE ( 'NONE', *, *, #38775, .T. ) ;
#11932 = CARTESIAN_POINT ( 'NONE',  ( -14.59284385650551563, -7.406986770994973490, 48.81910596585309747 ) ) ;
#11933 = VECTOR ( 'NONE', #11669, 1000.000000000000000 ) ;
#11934 = DIRECTION ( 'NONE',  ( 1.000000000000000000, 0.000000000000000000, 0.000000000000000000 ) ) ;
#11935 = CARTESIAN_POINT ( 'NONE',  ( -17.42409385541300892, -14.80920654474439502, 77.49999999999994316 ) ) ;
#11936 = DIRECTION ( 'NONE',  ( 0.9687793358424821033, -0.2479245821708677133, 0.000000000000000000 ) ) ;
#11937 = CARTESIAN_POINT ( 'NONE',  ( -13.51671022627207286, -9.001178471081288990, 57.04255703468526661 ) ) ;
#11938 = ORIENTED_EDGE ( 'NONE', *, *, #45775, .T. ) ;
#11939 = VERTEX_POINT ( 'NONE', #5405 ) ;
#11940 = CARTESIAN_POINT ( 'NONE',  ( -22.69284385541304161, -8.630756214087126565, 51.74842643355248129 ) ) ;
#11941 = EDGE_CURVE ( 'NONE', #17754, #1223, #34761, .T. ) ;
#11942 = EDGE_CURVE ( 'NONE', #22030, #17855, #4251, .T. ) ;
#11943 = CARTESIAN_POINT ( 'NONE',  ( -19.11145865927416310, -7.964113456900453691, 63.43089235103783352 ) ) ;
#11944 = CARTESIAN_POINT ( 'NONE',  ( -10.45452924831652375, -14.15584214187167511, 60.91821260770957025 ) ) ;
#11945 = AXIS2_PLACEMENT_3D ( 'NONE', #8488, #8748, #15360 ) ;
#11946 = SURFACE_STYLE_FILL_AREA ( #45437 ) ;
#11947 = ADVANCED_FACE ( 'NONE', ( #24114 ), #20426, .F. ) ;
#11948 = ADVANCED_FACE ( 'NONE', ( #9344 ), #28038, .T. ) ;
#11949 = CARTESIAN_POINT ( 'NONE',  ( -18.06139463723319949, -21.83834701327926808, 58.56120650458878174 ) ) ;
#11950 = DIRECTION ( 'NONE',  ( 0.8604039311673230550, 0.5096126717731923605, -7.110477545283408869E-08 ) ) ;
#11951 = AXIS2_PLACEMENT_3D ( 'NONE', #46843, #20507, #43407 ) ;
#11952 = ADVANCED_FACE ( 'NONE', ( #24362 ), #981, .T. ) ;
#11953 = CARTESIAN_POINT ( 'NONE',  ( -19.81804402429900236, -8.174913897241847138, 73.60608030023824710 ) ) ;
#11954 = CARTESIAN_POINT ( 'NONE',  ( -14.97188219925329378, -8.199429090594037461, 56.99999999999994316 ) ) ;
#11955 = VERTEX_POINT ( 'NONE', #20665 ) ;
#11956 = DIRECTION ( 'NONE',  ( 1.259531062780516415E-05, -2.755480461857868066E-06, 0.9999999999168828202 ) ) ;
#11957 = ORIENTED_EDGE ( 'NONE', *, *, #46088, .F. ) ;
#11958 = CARTESIAN_POINT ( 'NONE',  ( -23.46260449798628045, -11.17067817067885649, 73.51193301756617871 ) ) ;
#11959 = CARTESIAN_POINT ( 'NONE',  ( -15.05225219112592860, -21.44840536712413126, 65.11156449207337005 ) ) ;
#11960 = CARTESIAN_POINT ( 'NONE',  ( -18.71757194967216975, -7.929750632967406787, 70.37068030597254165 ) ) ;
#11961 = CARTESIAN_POINT ( 'NONE',  ( -10.66160605790631344, -13.00123564105898666, 68.03832347539896830 ) ) ;
#11962 = ADVANCED_FACE ( 'NONE', ( #35660 ), #1940, .T. ) ;
#11963 = AXIS2_PLACEMENT_3D ( 'NONE', #37650, #40866, #11561 ) ;
#11964 = ORIENTED_EDGE ( 'NONE', *, *, #39878, .F. ) ;
#11965 = CARTESIAN_POINT ( 'NONE',  ( -17.58740562021222686, -21.86528886929834670, 62.01968736857112674 ) ) ;
#11966 = CARTESIAN_POINT ( 'NONE',  ( -24.69662841158067579, -16.42583212380900903, 59.22994102966119101 ) ) ;
#11967 = LINE ( 'NONE', #4563, #48626 ) ;
#11968 = CARTESIAN_POINT ( 'NONE',  ( -7.924093855413059551, -6.859206544744110623, 47.99999999999998579 ) ) ;
#11969 = ORIENTED_EDGE ( 'NONE', *, *, #9497, .T. ) ;
#11970 = DIRECTION ( 'NONE',  ( -0.9294853595766568999, -0.3688590060343556187, 0.000000000000000000 ) ) ;
#11971 = CARTESIAN_POINT ( 'NONE',  ( -23.25757785049868787, -10.17517560731475967, 63.18690593950643120 ) ) ;
#11972 = CARTESIAN_POINT ( 'NONE',  ( -24.19391819315973180, -11.69922608242822726, 59.63235732785043552 ) ) ;
#11973 = APPLICATION_PROTOCOL_DEFINITION ( 'draft international standard', 'automotive_design', 1998, #33787 ) ;
#11974 = VERTEX_POINT ( 'NONE', #45808 ) ;
#11975 = DIRECTION ( 'NONE',  ( 1.053901171194056067E-05, -6.708308827411335869E-06, 0.9999999999219638669 ) ) ;
#11976 = CARTESIAN_POINT ( 'NONE',  ( -14.42409385541304090, -9.359200813967568422, 50.49621490985801842 ) ) ;
#11977 = CARTESIAN_POINT ( 'NONE',  ( -20.35208330028754631, -8.450993137587310855, 66.78104082230152017 ) ) ;
#11978 = CYLINDRICAL_SURFACE ( 'NONE', #31375, 1.050000000000002265 ) ;
#11979 = VERTEX_POINT ( 'NONE', #1207 ) ;
#11980 = CARTESIAN_POINT ( 'NONE',  ( -46.47622156840087371, -14.20920654474410760, 70.13000000000000966 ) ) ;
#11981 = ORIENTED_EDGE ( 'NONE', *, *, #39347, .F. ) ;
#11982 = LINE ( 'NONE', #34607, #40773 ) ;
#11983 = DIRECTION ( 'NONE',  ( -5.731567514496413899E-31, -1.020425574103664789E-16, -1.000000000000000000 ) ) ;
#11984 = ORIENTED_EDGE ( 'NONE', *, *, #25558, .F. ) ;
#11985 = CARTESIAN_POINT ( 'NONE',  ( -20.16518531629159838, -8.309878794262091972, 66.78104051650225870 ) ) ;
#11986 = ORIENTED_EDGE ( 'NONE', *, *, #45007, .T. ) ;
#11987 = ORIENTED_EDGE ( 'NONE', *, *, #39342, .F. ) ;
#11988 = ORIENTED_EDGE ( 'NONE', *, *, #35107, .T. ) ;
#11989 = DIRECTION ( 'NONE',  ( 2.331190576225089612E-06, -8.511884079520847478E-06, 0.9999999999610567070 ) ) ;
#11990 = CARTESIAN_POINT ( 'NONE',  ( -21.94915715192368921, -8.890837417924517538, 66.76875849712446609 ) ) ;
#11991 = LINE ( 'NONE', #660, #27921 ) ;
#11992 = CARTESIAN_POINT ( 'NONE',  ( -10.38655970317176802, -17.25373507390027328, 61.35754318564477927 ) ) ;
#11993 = CARTESIAN_POINT ( 'NONE',  ( -13.65684165595416921, -8.849801312179289781, 56.98439896120441261 ) ) ;
#11994 = CARTESIAN_POINT ( 'NONE',  ( -22.78262153964987036, -19.98509753430224833, 72.90046450679021461 ) ) ;
#11995 = ORIENTED_EDGE ( 'NONE', *, *, #4299, .T. ) ;
#11996 = ORIENTED_EDGE ( 'NONE', *, *, #10619, .F. ) ;
#11997 = CARTESIAN_POINT ( 'NONE',  ( -17.52853272358826686, -7.759682304905023642, 63.83584969886392457 ) ) ;
#11998 = ADVANCED_FACE ( 'NONE', ( #12537 ), #27563, .T. ) ;
#11999 = CARTESIAN_POINT ( 'NONE',  ( -10.00073915290244564, -14.17087342314384735, 64.57459177551746166 ) ) ;
#12000 = DIRECTION ( 'NONE',  ( 3.071710424422018668E-17, -6.404604876783312462E-16, -1.000000000000000000 ) ) ;
#12001 = CARTESIAN_POINT ( 'NONE',  ( -20.78299823145727387, -8.610459808214880439, 59.85597358678664648 ) ) ;
#12002 = VERTEX_POINT ( 'NONE', #2178 ) ;
#12003 = CARTESIAN_POINT ( 'NONE',  ( -16.78659385650551883, -9.302874398569244363, 51.68646062012417985 ) ) ;
#12005 = ORIENTED_EDGE ( 'NONE', *, *, #32649, .F. ) ;
#12004 = ADVANCED_FACE ( 'NONE', ( #17182 ), #36384, .T. ) ;
#12006 = DIRECTION ( 'NONE',  ( 0.7971031148784507581, -0.6038432116460915600, 6.916509187980650173E-08 ) ) ;
#12007 = CARTESIAN_POINT ( 'NONE',  ( -15.44183219577975130, -21.52267352039123338, 68.76696128071972680 ) ) ;
#12008 = ADVANCED_FACE ( 'NONE', ( #6846 ), #11027, .T. ) ;
#12009 = LINE ( 'NONE', #42774, #8745 ) ;
#12010 = EDGE_CURVE ( 'NONE', #48202, #6672, #18341, .T. ) ;
#12011 = ORIENTED_EDGE ( 'NONE', *, *, #19343, .F. ) ;
#12012 = DIRECTION ( 'NONE',  ( 0.000000000000000000, 0.000000000000000000, -1.000000000000000000 ) ) ;
#12013 = B_SPLINE_CURVE_WITH_KNOTS ( 'NONE', 3,
 ( #48495, #18449, #37153, #14729, #36431, #48021, #18696, #44112, #14257, #33215 ),
 .UNSPECIFIED., .F., .F.,
 ( 4, 2, 2, 2, 4 ),
 ( 0.1272669073658215244, 0.2522669073463236211, 0.3772669073268256623, 0.5022669073073278145, 0.6272669072878298557 ),
 .UNSPECIFIED. ) ;
#12014 = CARTESIAN_POINT ( 'NONE',  ( -11.67943375510494697, -18.89645239624664441, 68.50217487844219022 ) ) ;
#12015 = CARTESIAN_POINT ( 'NONE',  ( -12.10481839165579565, -9.592984239578061789, 57.13289628414671739 ) ) ;
#12016 = VERTEX_POINT ( 'NONE', #47251 ) ;
#12017 = CARTESIAN_POINT ( 'NONE',  ( -22.53429313110963861, -9.952421254863265787, 73.78161091678163075 ) ) ;
#12018 = CARTESIAN_POINT ( 'NONE',  ( -38.65852941833841783, -25.10920654474410441, 76.99999999999998579 ) ) ;
#12019 = LINE ( 'NONE', #27513, #18175 ) ;
#12020 = EDGE_LOOP ( 'NONE', ( #29780, #42985, #21889, #1425, #1004 ) ) ;
#12021 = FACE_OUTER_BOUND ( 'NONE', #30793, .T. ) ;
#12022 = ORIENTED_EDGE ( 'NONE', *, *, #44073, .T. ) ;
#12023 = LINE ( 'NONE', #8572, #651 ) ;
#12024 = CARTESIAN_POINT ( 'NONE',  ( -14.91112529534803066, -8.221969756899694559, 57.13527940342243028 ) ) ;
#12025 = ORIENTED_EDGE ( 'NONE', *, *, #37190, .F. ) ;
#12026 = DIRECTION ( 'NONE',  ( -0.9918916210775228226, -0.1270866320121812332, 6.503929234589264523E-08 ) ) ;
#12027 = LINE ( 'NONE', #27039, #24778 ) ;
#12028 = CARTESIAN_POINT ( 'NONE',  ( -17.42409385541299471, -14.80920654474434883, 62.02966884056656482 ) ) ;
#12029 = ORIENTED_EDGE ( 'NONE', *, *, #1712, .F. ) ;
#12030 = CARTESIAN_POINT ( 'NONE',  ( -11.28210193903344560, -11.34791643573311859, 64.15441847699383970 ) ) ;
#12031 =( BOUNDED_SURFACE ( )  B_SPLINE_SURFACE ( 3, 1, ( 
 ( #27276, #42304 ),
 ( #19893, #16170 ),
 ( #46238, #12497 ),
 ( #13685, #16901 ),
 ( #39568, #29218 ),
 ( #28967, #21356 ),
 ( #25043, #24800 ) ),
 .UNSPECIFIED., .T., .F., .F. ) 
 B_SPLINE_SURFACE_WITH_KNOTS ( ( 4, 3, 4 ),
 ( 2, 2 ),
 ( 0.000000000000000000, 0.5000000000000000000, 1.000000000000000000 ),
 ( 0.000000000000000000, 1.000000000000000000 ),
 .UNSPECIFIED. ) 
 GEOMETRIC_REPRESENTATION_ITEM ( )  RATIONAL_B_SPLINE_SURFACE ( (
 ( 1.000000000000000000, 1.000000000000000000),
 ( 0.3333333333333335369, 0.3333333333333330373),
 ( 0.3333333333333335369, 0.3333333333333330373),
 ( 1.000000000000000000, 1.000000000000000000),
 ( 0.3333333333333333703, 0.3333333333333333703),
 ( 0.3333333333333333703, 0.3333333333333333703),
 ( 1.000000000000000000, 1.000000000000000000) ) ) 
 REPRESENTATION_ITEM ( '' )  SURFACE ( )  );
#12032 = CARTESIAN_POINT ( 'NONE',  ( -16.41803040986462037, -7.880257286500736313, 60.31101663054752748 ) ) ;
#12033 = CARTESIAN_POINT ( 'NONE',  ( -11.96084830514426400, -9.743959610980004626, 60.74413522332266524 ) ) ;
#12034 = VERTEX_POINT ( 'NONE', #13243 ) ;
#12035 = CARTESIAN_POINT ( 'NONE',  ( -12.86353962931362283, -9.432586330540292607, 74.33395128836551180 ) ) ;
#12036 = LINE ( 'NONE', #3419, #17250 ) ;
#12037 = ORIENTED_EDGE ( 'NONE', *, *, #17868, .F. ) ;
#12038 = ORIENTED_EDGE ( 'NONE', *, *, #21938, .T. ) ;
#12039 = CARTESIAN_POINT ( 'NONE',  ( -24.84793640206982701, -14.18443463346696909, 69.83770693398628282 ) ) ;
#12040 = CARTESIAN_POINT ( 'NONE',  ( -10.71315705494743753, -11.57408983106119216, 71.18837245568840899 ) ) ;
#12041 = CARTESIAN_POINT ( 'NONE',  ( -41.92997620835424044, -14.90920654474420104, 66.95294117647057419 ) ) ;
#12042 = CARTESIAN_POINT ( 'NONE',  ( -12.82409385759799036, -9.359200813967568422, 50.49621490985803263 ) ) ;
#12043 = CARTESIAN_POINT ( 'NONE',  ( -12.40380818233537141, -19.68739593843253033, 61.69678633575567517 ) ) ;
#12044 = ADVANCED_FACE ( 'NONE', ( #21149 ), #13495, .T. ) ;
#12045 = DIRECTION ( 'NONE',  ( 6.023555219429074381E-06, -1.003033500007733605E-05, 0.9999999999315545285 ) ) ;
#12046 = DIRECTION ( 'NONE',  ( 0.000000000000000000, 0.000000000000000000, -1.000000000000000000 ) ) ;
#12047 =( BOUNDED_CURVE ( )  B_SPLINE_CURVE ( 3, ( #40084, #14186, #5870, #29241 ),
 .UNSPECIFIED., .F., .F. ) 
 B_SPLINE_CURVE_WITH_KNOTS ( ( 4, 4 ),
 ( 0.000000000000000000, 0.4074455897393628456 ),
 .UNSPECIFIED. ) 
 CURVE ( )  GEOMETRIC_REPRESENTATION_ITEM ( )  RATIONAL_B_SPLINE_CURVE ( ( 1.000000000000000000, 0.4567392136813396841, 0.3561768502900331534, 0.6983129098260804080 ) ) 
 REPRESENTATION_ITEM ( '' )  );
#12048 = DIRECTION ( 'NONE',  ( 0.9904243694481096316, 0.1380563957348939774, 6.973877024228147881E-08 ) ) ;
#12049 = ORIENTED_EDGE ( 'NONE', *, *, #32047, .T. ) ;
#12050 = EDGE_LOOP ( 'NONE', ( #197, #37974, #31577, #2250, #48097 ) ) ;
#12051 = CARTESIAN_POINT ( 'NONE',  ( -10.40651916427681023, -14.13340035957373075, 61.21821274675264846 ) ) ;
#12052 =( NAMED_UNIT ( * ) SI_UNIT ( $, .STERADIAN. ) SOLID_ANGLE_UNIT ( ) );
#12053 = VECTOR ( 'NONE', #40468, 1000.000000000000000 ) ;
#12054 = CARTESIAN_POINT ( 'NONE',  ( -10.02995815481606634, -13.89786978184575794, 57.63320425522585566 ) ) ;
#12055 = ORIENTED_EDGE ( 'NONE', *, *, #2685, .T. ) ;
#12056 =( BOUNDED_CURVE ( )  B_SPLINE_CURVE ( 3, ( #35610, #1887, #10257, #21091 ),
 .UNSPECIFIED., .F., .F. ) 
 B_SPLINE_CURVE_WITH_KNOTS ( ( 4, 4 ),
 ( 0.5000000000000000000, 0.9074455897393668424 ),
 .UNSPECIFIED. ) 
 CURVE ( )  GEOMETRIC_REPRESENTATION_ITEM ( )  RATIONAL_B_SPLINE_CURVE ( ( 1.000000000000003109, 0.4567392136813368531, 0.3561768502900296562, 0.6983129098260851819 ) ) 
 REPRESENTATION_ITEM ( '' )  );
#12057 = ORIENTED_EDGE ( 'NONE', *, *, #24511, .F. ) ;
#12058 = FACE_OUTER_BOUND ( 'NONE', #40317, .T. ) ;
#12059 = CARTESIAN_POINT ( 'NONE',  ( -17.59331746709300148, -7.761237804004919916, 63.70057029381062819 ) ) ;
#12060 = EDGE_CURVE ( 'NONE', #1531, #21712, #31890, .T. ) ;
#12061 = CARTESIAN_POINT ( 'NONE',  ( -14.98986966776551988, -21.85036012251616810, 65.29870846104924453 ) ) ;
#12062 = CARTESIAN_POINT ( 'NONE',  ( -22.94085434386056832, -9.802298134861713308, 70.19673941016031904 ) ) ;
#12063 = ADVANCED_FACE ( 'NONE', ( #36618 ), #44295, .T. ) ;
#12064 = ORIENTED_EDGE ( 'NONE', *, *, #9392, .T. ) ;
#12065 = B_SPLINE_CURVE_WITH_KNOTS ( 'NONE', 1,
 ( #33326, #41471 ),
 .UNSPECIFIED., .F., .F.,
 ( 2, 2 ),
 ( 0.000000000000000000, 1.000000000000000000 ),
 .UNSPECIFIED. ) ;
#12066 = CARTESIAN_POINT ( 'NONE',  ( -13.05823872554153908, -9.336963863356308124, 70.86542013787308747 ) ) ;
#12067 = EDGE_CURVE ( 'NONE', #15704, #26298, #32698, .T. ) ;
#12068 = CARTESIAN_POINT ( 'NONE',  ( -24.45288365649568618, -15.45035942066159862, 69.68874360283344060 ) ) ;
#12069 = ORIENTED_EDGE ( 'NONE', *, *, #43510, .T. ) ;
#12070 = CARTESIAN_POINT ( 'NONE',  ( -11.17842666812006769, -10.74653426074781848, 57.39558607234117460 ) ) ;
#12071 = EDGE_CURVE ( 'NONE', #45570, #36726, #43404, .T. ) ;
#12072 = CARTESIAN_POINT ( 'NONE',  ( -11.08591710707173839, -18.72456284283582661, 61.42710830429783186 ) ) ;
#12073 = ORIENTED_EDGE ( 'NONE', *, *, #8727, .F. ) ;
#12075 = EDGE_CURVE ( 'NONE', #10295, #34444, #19813, .T. ) ;
#12074 = CARTESIAN_POINT ( 'NONE',  ( -12.26730668522635526, -19.62818085036556681, 65.01107574152555912 ) ) ;
#12076 = VERTEX_POINT ( 'NONE', #20902 ) ;
#12077 = DIRECTION ( 'NONE',  ( 3.071710424422018668E-17, -6.404604876783312462E-16, -1.000000000000000000 ) ) ;
#12078 = DIRECTION ( 'NONE',  ( -0.1240347345892086200, 1.145860353393066553E-16, -0.9922778767136676281 ) ) ;
#12079 = ORIENTED_EDGE ( 'NONE', *, *, #18443, .F. ) ;
#12080 = DIRECTION ( 'NONE',  ( -3.071710424422018668E-17, 6.404604876783312462E-16, 1.000000000000000000 ) ) ;
#12081 = DIRECTION ( 'NONE',  ( 0.9687793358424821033, -0.2479245821708680464, 0.000000000000000000 ) ) ;
#12082 = AXIS2_PLACEMENT_3D ( 'NONE', #7918, #281, #34725 ) ;
#12083 = CARTESIAN_POINT ( 'NONE',  ( -17.77409385650551243, -9.792211528768504536, 50.49490371617623197 ) ) ;
#12084 = DIRECTION ( 'NONE',  ( -0.9729319276368276759, -0.2310918955413239773, 6.827553174175007530E-08 ) ) ;
#12085 = CARTESIAN_POINT ( 'NONE',  ( -22.24151848281995214, -9.126331139912949197, 59.82147588101616265 ) ) ;
#12086 = ORIENTED_EDGE ( 'NONE', *, *, #40612, .F. ) ;
#12087 = DIRECTION ( 'NONE',  ( 2.866981220435666553E-17, -1.000000000000000000, -1.190614954331866791E-16 ) ) ;
#12088 = DIRECTION ( 'NONE',  ( 0.8398192074808118468, 0.5428661886195297326, 7.907900705247677662E-08 ) ) ;
#12089 = PLANE ( 'NONE',  #19525 ) ;
#12090 = CARTESIAN_POINT ( 'NONE',  ( -18.38376433957202849, -21.74317146278215773, 68.83017111679792777 ) ) ;
#12091 = DIRECTION ( 'NONE',  ( -0.000000000000000000, -1.000000000000000000, -0.000000000000000000 ) ) ;
#12092 = ORIENTED_EDGE ( 'NONE', *, *, #29570, .T. ) ;
#12093 = ORIENTED_EDGE ( 'NONE', *, *, #8114, .T. ) ;
#12094 = APPLICATION_CONTEXT ( 'automotive_design' ) ;
#12095 = DIRECTION ( 'NONE',  ( 0.8875028193683940358, 0.4608022847308269609, -4.020963237754318724E-08 ) ) ;
#12096 = CARTESIAN_POINT ( 'NONE',  ( -12.36794907275616850, -19.72224022788673636, 61.54678633597969650 ) ) ;
#12097 = VERTEX_POINT ( 'NONE', #47724 ) ;
#12098 = CARTESIAN_POINT ( 'NONE',  ( -10.00747521095153303, -15.51449648374953050, 57.61146884931378054 ) ) ;
#12099 = CARTESIAN_POINT ( 'NONE',  ( -15.47894645291934523, -21.58867816219044755, 68.46104220717563749 ) ) ;
#12100 = CARTESIAN_POINT ( 'NONE',  ( -20.75534385759799250, -8.623186033802570094, 49.24843789510466507 ) ) ;
#12101 = CARTESIAN_POINT ( 'NONE',  ( -28.05267866845275293, -15.70886298607290499, 54.49999999999995026 ) ) ;
#12102 = EDGE_CURVE ( 'NONE', #14963, #28111, #48095, .T. ) ;
#12103 = CARTESIAN_POINT ( 'NONE',  ( -14.48548941065490148, -8.400516866317895293, 67.27447142263336843 ) ) ;
#12104 = CARTESIAN_POINT ( 'NONE',  ( -10.82867469351122836, -11.34449526142513598, 67.73369307302053244 ) ) ;
#12105 = ORIENTED_EDGE ( 'NONE', *, *, #5632, .F. ) ;
#12106 = DIRECTION ( 'NONE',  ( -5.731567514496413899E-31, -1.020425574103664789E-16, -1.000000000000000000 ) ) ;
#12107 = CARTESIAN_POINT ( 'NONE',  ( -13.38462506958126319, -20.58719851387657940, 58.04650077714654088 ) ) ;
#12108 = LINE ( 'NONE', #27124, #13005 ) ;
#12109 = CARTESIAN_POINT ( 'NONE',  ( -12.80044372018415189, -20.06500349168936737, 72.10653684543767383 ) ) ;
#12110 = CARTESIAN_POINT ( 'NONE',  ( -16.03289554736505806, -7.947204745776725865, 67.32934463618931886 ) ) ;
#12111 = EDGE_CURVE ( 'NONE', #15459, #41134, #17443, .T. ) ;
#12112 = ORIENTED_EDGE ( 'NONE', *, *, #41587, .F. ) ;
#12113 = ORIENTED_EDGE ( 'NONE', *, *, #25640, .T. ) ;
#12114 = AXIS2_PLACEMENT_3D ( 'NONE', #5441, #1740, #34482 ) ;
#12115 = CARTESIAN_POINT ( 'NONE',  ( -22.86159385650551457, -9.295667164867525756, 49.30633214617472504 ) ) ;
#12116 = ORIENTED_EDGE ( 'NONE', *, *, #7655, .T. ) ;
#12117 = CARTESIAN_POINT ( 'NONE',  ( -12.01937617657256041, -9.681437477770858280, 60.72064570034685715 ) ) ;
#12118 = AXIS2_PLACEMENT_3D ( 'NONE', #343, #35023, #34790 ) ;
#12119 = CARTESIAN_POINT ( 'NONE',  ( -10.40511033146429831, -14.11732416830307280, 57.33336190745325212 ) ) ;
#12120 = ORIENTED_EDGE ( 'NONE', *, *, #5999, .F. ) ;
#12121 = CARTESIAN_POINT ( 'NONE',  ( -19.57409385759799036, -6.859212275519751323, 50.50378509014259265 ) ) ;
#12122 = EDGE_CURVE ( 'NONE', #48317, #30462, #40338, .T. ) ;
#12123 = CARTESIAN_POINT ( 'NONE',  ( -11.23918011089898705, -11.53084126649161512, 64.22170027535517534 ) ) ;
#12124 = CARTESIAN_POINT ( 'NONE',  ( -16.08649462381330864, -22.13826890709367845, 58.46398360678714567 ) ) ;
#12125 = ORIENTED_EDGE ( 'NONE', *, *, #46941, .F. ) ;
#12126 = EDGE_CURVE ( 'NONE', #30297, #2344, #964, .T. ) ;
#12127 = DIRECTION ( 'NONE',  ( -3.071710424422018668E-17, 6.404604876783312462E-16, 1.000000000000000000 ) ) ;
#12128 = EDGE_CURVE ( 'NONE', #41672, #40331, #41813, .T. ) ;
#12129 = CARTESIAN_POINT ( 'NONE',  ( -19.37616744185158879, -21.99900390342548206, 58.71002665166666645 ) ) ;
#12130 = EDGE_LOOP ( 'NONE', ( #29730, #40693, #37273, #3711 ) ) ;
#12131 = FACE_OUTER_BOUND ( 'NONE', #7502, .T. ) ;
#12132 = CARTESIAN_POINT ( 'NONE',  ( -13.84336496337389022, -20.88234202223394931, 68.46184952764561160 ) ) ;
#12133 = ORIENTED_EDGE ( 'NONE', *, *, #20178, .F. ) ;
#12134 = DIRECTION ( 'NONE',  ( 0.9687793358424819923, -0.2479245821708680464, 0.000000000000000000 ) ) ;
#12135 = CARTESIAN_POINT ( 'NONE',  ( -12.52738813637484405, -19.88632359053370990, 61.39678650461756604 ) ) ;
#12136 = CARTESIAN_POINT ( 'NONE',  ( -24.00897149951030940, -12.43446728902662457, 73.43328766012302822 ) ) ;
#12137 = ORIENTED_EDGE ( 'NONE', *, *, #23873, .F. ) ;
#12138 = CYLINDRICAL_SURFACE ( 'NONE', #28598, 0.1499999999999990508 ) ;
#12139 = CARTESIAN_POINT ( 'NONE',  ( -17.87364429212824390, -21.79475623858289168, 58.51439479403251909 ) ) ;
#12140 = EDGE_CURVE ( 'NONE', #12494, #35872, #3625, .T. ) ;
#12141 = DIRECTION ( 'NONE',  ( 3.549360974554993999E-17, -6.371834667797928663E-18, -1.000000000000000000 ) ) ;
#12142 = CARTESIAN_POINT ( 'NONE',  ( -24.04021708909630206, -12.36549076622675791, 73.12736853451067986 ) ) ;
#12143 = CARTESIAN_POINT ( 'NONE',  ( -24.37947642869176690, -14.01903517687732759, 73.42271482001694949 ) ) ;
#12144 = CARTESIAN_POINT ( 'NONE',  ( -14.60783717270099835, -21.70648693424663378, 58.35113322083577003 ) ) ;
#12145 = EDGE_CURVE ( 'NONE', #38602, #3056, #48397, .T. ) ;
#12146 = DIRECTION ( 'NONE',  ( -8.136802275736123818E-17, 2.353473986169886647E-17, -1.000000000000000000 ) ) ;
#12147 = CARTESIAN_POINT ( 'NONE',  ( -20.88427521310116575, -20.89426873771111559, 62.12973820747942000 ) ) ;
#12148 = CARTESIAN_POINT ( 'NONE',  ( -10.48723240375378829, -15.75052704102940915, 64.52388266229672809 ) ) ;
#12149 = EDGE_CURVE ( 'NONE', #10113, #17364, #18203, .T. ) ;
#12150 = ADVANCED_FACE ( 'NONE', ( #42469 ), #23274, .F. ) ;
#12151 = CARTESIAN_POINT ( 'NONE',  ( -16.16784385650552025, -6.428312510596451368, 51.20221977374900035 ) ) ;
#12152 = AXIS2_PLACEMENT_3D ( 'NONE', #38908, #19960, #5188 ) ;
#12153 = ORIENTED_EDGE ( 'NONE', *, *, #37682, .F. ) ;
#12154 = PLANE ( 'NONE',  #44007 ) ;
#12155 = CARTESIAN_POINT ( 'NONE',  ( -10.47928406297145720, -17.50635424218827296, 64.76592889887460558 ) ) ;
#12156 = ORIENTED_EDGE ( 'NONE', *, *, #15217, .T. ) ;
#12157 = CARTESIAN_POINT ( 'NONE',  ( -23.36565744117094923, -18.61087216430447455, 65.82389142905810786 ) ) ;
#12158 = CARTESIAN_POINT ( 'NONE',  ( -10.63173029587417595, -17.86977651231121911, 71.75992364232735099 ) ) ;
#12159 = CARTESIAN_POINT ( 'NONE',  ( -23.21283044961208830, -10.11939778159179859, 63.25681392212788268 ) ) ;
#12160 = CARTESIAN_POINT ( 'NONE',  ( -20.03282965983824226, -21.84088468745754597, 53.89198173725360874 ) ) ;
#12161 = ORIENTED_EDGE ( 'NONE', *, *, #25916, .F. ) ;
#12162 = CARTESIAN_POINT ( 'NONE',  ( -10.37599212182869124, -14.63324797960940593, 71.34254748307667171 ) ) ;
#12163 = CARTESIAN_POINT ( 'NONE',  ( -24.42401643431037073, -14.84212902100172293, 59.54300237020546405 ) ) ;
#12164 = LINE ( 'NONE', #20533, #46393 ) ;
#12165 = ORIENTED_EDGE ( 'NONE', *, *, #10699, .F. ) ;
#12166 = CARTESIAN_POINT ( 'NONE',  ( -16.99415041099795332, -7.769321291326151346, 70.37547239324983650 ) ) ;
#12167 = CARTESIAN_POINT ( 'NONE',  ( -23.69044173319201363, -11.56146079933792237, 59.63803016077844177 ) ) ;
#12168 = CARTESIAN_POINT ( 'NONE',  ( -24.55128148229147911, -12.63992024488134902, 69.97254205454612475 ) ) ;
#12169 = PLANE ( 'NONE',  #40920 ) ;
#12170 = DIRECTION ( 'NONE',  ( 1.000000000000000000, 0.000000000000000000, 0.000000000000000000 ) ) ;
#12171 = ORIENTED_EDGE ( 'NONE', *, *, #1893, .T. ) ;
#12172 = VERTEX_POINT ( 'NONE', #34089 ) ;
#12173 = CARTESIAN_POINT ( 'NONE',  ( -23.25534385541304161, -8.623186033802570094, 49.24843789510466507 ) ) ;
#12174 = EDGE_CURVE ( 'NONE', #23522, #42856, #377, .T. ) ;
#12175 = CARTESIAN_POINT ( 'NONE',  ( -22.75539019595754908, -10.19575032747719412, 66.82710158566565894 ) ) ;
#12176 = CARTESIAN_POINT ( 'NONE',  ( -23.34903492872366115, -11.08148469299992378, 73.43481278317960914 ) ) ;
#12177 = CARTESIAN_POINT ( 'NONE',  ( -16.94458633259734270, -7.374567983260779336, 74.14513688882354359 ) ) ;
#12178 =( BOUNDED_CURVE ( )  B_SPLINE_CURVE ( 3, ( #23860, #35874, #28749, #43541 ),
 .UNSPECIFIED., .F., .F. ) 
 B_SPLINE_CURVE_WITH_KNOTS ( ( 4, 4 ),
 ( 0.5000000000000000000, 0.9074455897393589598 ),
 .UNSPECIFIED. ) 
 CURVE ( )  GEOMETRIC_REPRESENTATION_ITEM ( )  RATIONAL_B_SPLINE_CURVE ( ( 0.9999999999999803491, 0.4567392136813388515, 0.3561768502900464761, 0.6983129098260818513 ) ) 
 REPRESENTATION_ITEM ( '' )  );
#12179 = AXIS2_PLACEMENT_3D ( 'NONE', #3746, #26164, #27123 ) ;
#12180 = EDGE_CURVE ( 'NONE', #27273, #26781, #26887, .T. ) ;
#12181 = CARTESIAN_POINT ( 'NONE',  ( -17.66159697976433307, -21.85550285805611637, 58.42025434932890704 ) ) ;
#12182 = CARTESIAN_POINT ( 'NONE',  ( -15.39388989008627995, -21.97733388496078177, 72.23070757706680922 ) ) ;
#12183 = CARTESIAN_POINT ( 'NONE',  ( -20.18941521006531303, -7.891347330600439136, 73.83601268700121523 ) ) ;
#12184 = CARTESIAN_POINT ( 'NONE',  ( -24.76540239943457422, -16.07765717072269140, 66.17829646510101327 ) ) ;
#12185 = ORIENTED_EDGE ( 'NONE', *, *, #46776, .T. ) ;
#12186 = CARTESIAN_POINT ( 'NONE',  ( -22.44011750557629270, -19.69186611616677851, 69.40091412993344022 ) ) ;
#12187 =( BOUNDED_SURFACE ( )  B_SPLINE_SURFACE ( 3, 1, ( 
 ( #3498, #37958 ),
 ( #4245, #33512 ),
 ( #44397, #19256 ),
 ( #48559, #46087 ),
 ( #30842, #19751 ),
 ( #27369, #1256 ),
 ( #46584, #12348 ) ),
 .UNSPECIFIED., .T., .F., .F. ) 
 B_SPLINE_SURFACE_WITH_KNOTS ( ( 4, 3, 4 ),
 ( 2, 2 ),
 ( 0.000000000000000000, 0.5000000000000000000, 1.000000000000000000 ),
 ( 0.000000000000000000, 1.000000000000000000 ),
 .UNSPECIFIED. ) 
 GEOMETRIC_REPRESENTATION_ITEM ( )  RATIONAL_B_SPLINE_SURFACE ( (
 ( 1.000000000000000000, 1.000000000000000000),
 ( 0.3333333333333335369, 0.3333333333333330373),
 ( 0.3333333333333335369, 0.3333333333333330373),
 ( 1.000000000000000000, 1.000000000000000000),
 ( 0.3333333333333333703, 0.3333333333333333703),
 ( 0.3333333333333333703, 0.3333333333333333703),
 ( 1.000000000000000000, 1.000000000000000000) ) ) 
 REPRESENTATION_ITEM ( '' )  SURFACE ( )  );
#12188 = CARTESIAN_POINT ( 'NONE',  ( -50.42509385541305988, -8.109206544744111511, 49.44999999999998863 ) ) ;
#12189 = ORIENTED_EDGE ( 'NONE', *, *, #19406, .F. ) ;
#12190 = CARTESIAN_POINT ( 'NONE',  ( -12.39983768287018329, -19.75505771991250725, 61.69118872147407018 ) ) ;
#12191 = CARTESIAN_POINT ( 'NONE',  ( -19.46797834413568040, -22.79580085574647441, 53.49999999999995026 ) ) ;
#12192 = ORIENTED_EDGE ( 'NONE', *, *, #20935, .F. ) ;
#12193 = CARTESIAN_POINT ( 'NONE',  ( -18.10844610942486099, -22.22787712852580455, 65.48498797171305341 ) ) ;
#12194 = ORIENTED_EDGE ( 'NONE', *, *, #23223, .T. ) ;
#12195 = DIRECTION ( 'NONE',  ( 6.291559634385637730E-07, -1.530398238691524640E-06, 0.9999999999986310950 ) ) ;
#12196 = CARTESIAN_POINT ( 'NONE',  ( 22.62590614458706639, 0.6407533398237036382, 50.52649563099625851 ) ) ;
#12197 = CARTESIAN_POINT ( 'NONE',  ( -50.42609385541305755, -14.90920654474428630, 74.09999999999998010 ) ) ;
#12198 = VERTEX_POINT ( 'NONE', #30426 ) ;
#12199 = CARTESIAN_POINT ( 'NONE',  ( -19.80621920301059902, -19.48766556757794532, 49.52966884056656482 ) ) ;
#12200 = DIRECTION ( 'NONE',  ( 0.9687793358424821033, -0.2479245821708679909, 0.000000000000000000 ) ) ;
#12201 = CARTESIAN_POINT ( 'NONE',  ( -23.34299683607928699, -18.64475395501998278, 73.17857113406003577 ) ) ;
#12202 = CARTESIAN_POINT ( 'NONE',  ( -10.40860991809309155, -15.50898095412354571, 57.85320721669017985 ) ) ;
#12203 = ADVANCED_FACE ( 'NONE', ( #34325 ), #45441, .T. ) ;
#12204 = ADVANCED_FACE ( 'NONE', ( #45920 ), #45690, .T. ) ;
#12205 = CARTESIAN_POINT ( 'NONE',  ( -11.38872272660762164, -18.35547376437386191, 57.80714557486621885 ) ) ;
#12206 = DIRECTION ( 'NONE',  ( -3.071710424422018668E-17, 6.404604876783312462E-16, 1.000000000000000000 ) ) ;
#12207 = DIRECTION ( 'NONE',  ( 0.5097212845717493668, -0.8603395911234852367, 0.000000000000000000 ) ) ;
#12208 = EDGE_LOOP ( 'NONE', ( #5495, #32035, #2033 ) ) ;
#12209 = CARTESIAN_POINT ( 'NONE',  ( -12.05483428091225129, -10.31798718066989551, 67.49896870046983111 ) ) ;
#12210 = ORIENTED_EDGE ( 'NONE', *, *, #17983, .F. ) ;
#12211 = DIRECTION ( 'NONE',  ( -3.071710424422018668E-17, 6.404604876783312462E-16, 1.000000000000000000 ) ) ;
#12212 = EDGE_LOOP ( 'NONE', ( #24017, #27100 ) ) ;
#12213 = CARTESIAN_POINT ( 'NONE',  ( -13.84085632603101956, -17.84827948783496865, 49.52966884056656482 ) ) ;
#12214 = AXIS2_PLACEMENT_3D ( 'NONE', #19128, #48674, #34135 ) ;
#12215 = ADVANCED_FACE ( 'NONE', ( #38024 ), #46559, .T. ) ;
#12216 = EDGE_CURVE ( 'NONE', #38535, #8357, #15070, .T. ) ;
#12217 = FACE_BOUND ( 'NONE', #9329, .T. ) ;
#12218 = VERTEX_POINT ( 'NONE', #17314 ) ;
#12219 = AXIS2_PLACEMENT_3D ( 'NONE', #5913, #9625, #24640 ) ;
#12220 = ORIENTED_EDGE ( 'NONE', *, *, #14116, .F. ) ;
#12221 = ORIENTED_EDGE ( 'NONE', *, *, #5782, .T. ) ;
#12222 = CYLINDRICAL_SURFACE ( 'NONE', #36708, 0.1499999999999963030 ) ;
#12223 = CARTESIAN_POINT ( 'NONE',  ( -22.07409385541323488, -6.859212275519745994, 50.50378509014079498 ) ) ;
#12224 = CARTESIAN_POINT ( 'NONE',  ( -16.50454646563301964, -22.20232569423288282, 65.34069100801451668 ) ) ;
#12225 = DIRECTION ( 'NONE',  ( -3.071710424422018668E-17, 6.404604876783312462E-16, 1.000000000000000000 ) ) ;
#12226 = LINE ( 'NONE', #35355, #12941 ) ;
#12227 = CARTESIAN_POINT ( 'NONE',  ( -19.43397249051689357, -8.102278120859530475, 60.07166125860918271 ) ) ;
#12228 = VERTEX_POINT ( 'NONE', #27922 ) ;
#12229 = ORIENTED_EDGE ( 'NONE', *, *, #33788, .F. ) ;
#12230 = CARTESIAN_POINT ( 'NONE',  ( -22.83659385650551954, -6.915538690918074494, 49.31353937987644542 ) ) ;
#12231 = EDGE_CURVE ( 'NONE', #26697, #25255, #29524, .T. ) ;
#12232 = CARTESIAN_POINT ( 'NONE',  ( -10.39679176622870038, -14.24023819782134304, 64.40275955115841100 ) ) ;
#12233 = FACE_OUTER_BOUND ( 'NONE', #19216, .T. ) ;
#12234 = DIRECTION ( 'NONE',  ( 2.866981220435666553E-17, -1.000000000000000000, -1.190614954331866791E-16 ) ) ;
#12235 = ORIENTED_EDGE ( 'NONE', *, *, #48551, .F. ) ;
#12236 = CARTESIAN_POINT ( 'NONE',  ( -20.69909385650551670, -8.114302828567740988, 52.18300498402516041 ) ) ;
#12237 = VERTEX_POINT ( 'NONE', #20055 ) ;
#12238 = DIRECTION ( 'NONE',  ( -3.840742979682813137E-07, 4.934726756126598837E-06, -0.9999999999877504653 ) ) ;
#12239 = CARTESIAN_POINT ( 'NONE',  ( -15.29809632361469873, -21.47854941203162937, 68.57592918283285144 ) ) ;
#12240 = CARTESIAN_POINT ( 'NONE',  ( -17.39761456938454742, -7.809256627251312644, 67.32039592144390383 ) ) ;
#12241 = EDGE_LOOP ( 'NONE', ( #37015, #46072, #45398, #27348, #40729 ) ) ;
#12242 = CARTESIAN_POINT ( 'NONE',  ( -11.63855245876247935, -18.75048069921609439, 68.23306329961977212 ) ) ;
#12243 = B_SPLINE_CURVE_WITH_KNOTS ( 'NONE', 3,
 ( #43622, #24667, #25143, #36437, #2719, #17726, #32754, #47781, #14020, #9882 ),
 .UNSPECIFIED., .F., .F.,
 ( 4, 2, 2, 2, 4 ),
 ( 0.000000000000000000, 0.2500000000000000000, 0.5000000000000000000, 0.7500000000000000000, 1.000000000000000000 ),
 .UNSPECIFIED. ) ;
#12244 = AXIS2_PLACEMENT_3D ( 'NONE', #13361, #16813, #32573 ) ;
#12245 = FACE_OUTER_BOUND ( 'NONE', #11664, .T. ) ;
#12246 = CARTESIAN_POINT ( 'NONE',  ( -50.42609385541305755, -14.80920654474422271, 68.06470588235292496 ) ) ;
#12247 = EDGE_LOOP ( 'NONE', ( #35853, #36976, #45268, #25438 ) ) ;
#12248 = CARTESIAN_POINT ( 'NONE',  ( -10.44551236293470353, -15.36195525749487345, 57.58409439150996434 ) ) ;
#12249 = LINE ( 'NONE', #31448, #26779 ) ;
#12250 = DIRECTION ( 'NONE',  ( -3.071710424422018668E-17, 6.404604876783312462E-16, 1.000000000000000000 ) ) ;
#12251 = ORIENTED_EDGE ( 'NONE', *, *, #42481, .T. ) ;
#12252 = DIRECTION ( 'NONE',  ( 2.200805972648249745E-07, 3.006001593475220059E-06, 0.9999999999954577445 ) ) ;
#12253 = ORIENTED_EDGE ( 'NONE', *, *, #33662, .F. ) ;
#12254 = CARTESIAN_POINT ( 'NONE',  ( -9.975237612755753602, -14.67793925367211116, 71.42808438716600961 ) ) ;
#12255 = CARTESIAN_POINT ( 'NONE',  ( -22.04114742393716142, -9.481025248639417313, 59.73643293354757589 ) ) ;
#12256 = ORIENTED_EDGE ( 'NONE', *, *, #25987, .T. ) ;
#12257 = ADVANCED_FACE ( 'NONE', ( #24960 ), #8980, .T. ) ;
#12258 = CYLINDRICAL_SURFACE ( 'NONE', #14001, 0.1500000000000038802 ) ;
#12259 = CARTESIAN_POINT ( 'NONE',  ( -23.81768783790253252, -11.95822662118994373, 59.49852322759251422 ) ) ;
#12260 = CARTESIAN_POINT ( 'NONE',  ( -44.67409385541304800, -14.80920654474410725, 70.50000000000000000 ) ) ;
#12261 = ORIENTED_EDGE ( 'NONE', *, *, #1728, .T. ) ;
#12262 = CARTESIAN_POINT ( 'NONE',  ( -9.990623027812100432, -14.31192454061599229, 64.57299275950818185 ) ) ;
#12263 = CARTESIAN_POINT ( 'NONE',  ( -15.13554010266625482, -21.89904150877020328, 68.76931220517136012 ) ) ;
#12264 = CARTESIAN_POINT ( 'NONE',  ( -19.65950609550678152, -21.49557518541719148, 65.75926423743261751 ) ) ;
#12265 = CARTESIAN_POINT ( 'NONE',  ( -10.89657400502345830, -17.34179108361152544, 68.28648913934780751 ) ) ;
#12266 = ORIENTED_EDGE ( 'NONE', *, *, #23913, .T. ) ;
#12267 = CARTESIAN_POINT ( 'NONE',  ( -16.07630405233268434, -7.886179812623181462, 67.55496168274575552 ) ) ;
#12268 = EDGE_CURVE ( 'NONE', #34163, #48033, #19497, .T. ) ;
#12269 = EDGE_CURVE ( 'NONE', #18224, #36615, #31864, .T. ) ;
#12270 = LINE ( 'NONE', #5630, #10215 ) ;
#12271 = ORIENTED_EDGE ( 'NONE', *, *, #10716, .F. ) ;
#12272 = EDGE_LOOP ( 'NONE', ( #41893, #13881 ) ) ;
#12273 = EDGE_CURVE ( 'NONE', #14369, #14223, #11306, .T. ) ;
#12274 = CARTESIAN_POINT ( 'NONE',  ( -24.85298803532284850, -14.24811622150979673, 69.76001114652854085 ) ) ;
#12275 = CARTESIAN_POINT ( 'NONE',  ( -19.46159385759798965, -7.228003583438117552, 51.38655588711986155 ) ) ;
#12276 = CARTESIAN_POINT ( 'NONE',  ( -17.42409385541300182, -14.80920654474440745, 53.27966884056655061 ) ) ;
#12277 = CARTESIAN_POINT ( 'NONE',  ( -20.44284385650551883, -8.811426318492348031, 52.18089403414751359 ) ) ;
#12278 = EDGE_CURVE ( 'NONE', #43778, #40803, #24001, .T. ) ;
#12279 = CARTESIAN_POINT ( 'NONE',  ( -27.42409385541305511, -25.10920654474410441, 56.99999999999999289 ) ) ;
#12280 = CARTESIAN_POINT ( 'NONE',  ( -12.20309422964675150, -20.12380354524033521, 64.98179449731530610 ) ) ;
#12281 = CARTESIAN_POINT ( 'NONE',  ( -9.974806312911359996, -14.91297370499342989, 74.89755268075251138 ) ) ;
#12282 = AXIS2_PLACEMENT_3D ( 'NONE', #8634, #38898, #37924 ) ;
#12283 = VECTOR ( 'NONE', #8481, 1000.000000000000000 ) ;
#12284 = ORIENTED_EDGE ( 'NONE', *, *, #46588, .F. ) ;
#12285 = ORIENTED_EDGE ( 'NONE', *, *, #33187, .T. ) ;
#12286 = CARTESIAN_POINT ( 'NONE',  ( -21.94239175829699207, -20.22099772874085488, 59.06442899522711087 ) ) ;
#12287 = EDGE_CURVE ( 'NONE', #1571, #37218, #30829, .T. ) ;
#12288 = CARTESIAN_POINT ( 'NONE',  ( -13.82689732469268229, -20.87277619789260186, 68.47097268802275494 ) ) ;
#12289 = CARTESIAN_POINT ( 'NONE',  ( -19.61601503992405071, -21.50980213996393786, 65.76486213821364402 ) ) ;
#12290 = CARTESIAN_POINT ( 'NONE',  ( -18.76558392140857023, -7.480892851696864021, 70.55563303198719893 ) ) ;
#12291 = ORIENTED_EDGE ( 'NONE', *, *, #45086, .F. ) ;
#12292 = ORIENTED_EDGE ( 'NONE', *, *, #23675, .F. ) ;
#12293 = DIRECTION ( 'NONE',  ( 1.371992797150048625E-08, -1.272593384837864910E-06, 0.9999999999991900923 ) ) ;
#12294 = CARTESIAN_POINT ( 'NONE',  ( -23.56879427660422266, -11.34691063241640130, 73.77682139093690239 ) ) ;
#12295 = DIRECTION ( 'NONE',  ( -0.000000000000000000, 1.000000000000000000, -0.000000000000000000 ) ) ;
#12296 = CARTESIAN_POINT ( 'NONE',  ( -15.13017050835524913, -18.89591645955643884, 49.52966884056656482 ) ) ;
#12297 = VERTEX_POINT ( 'NONE', #5040 ) ;
#12298 = CARTESIAN_POINT ( 'NONE',  ( -10.52991759648590531, -16.02177972226642311, 68.27767831073917648 ) ) ;
#12299 = DIRECTION ( 'NONE',  ( 0.7506333037770492878, -0.6607190350373991494, 0.000000000000000000 ) ) ;
#12300 = ORIENTED_EDGE ( 'NONE', *, *, #34675, .F. ) ;
#12301 = CARTESIAN_POINT ( 'NONE',  ( -11.63929734443426867, -10.76555703936739938, 57.35336384308645563 ) ) ;
#12302 =( BOUNDED_CURVE ( )  B_SPLINE_CURVE ( 3, ( #13585, #37196, #14530, #32790 ),
 .UNSPECIFIED., .F., .F. ) 
 B_SPLINE_CURVE_WITH_KNOTS ( ( 4, 4 ),
 ( 0.9074455897393730597, 1.000000000000000000 ),
 .UNSPECIFIED. ) 
 CURVE ( )  GEOMETRIC_REPRESENTATION_ITEM ( )  RATIONAL_B_SPLINE_CURVE ( ( 0.6983129098261336987, 0.7760317562607332853, 0.8765941196520220524, 1.000000000000000000 ) ) 
 REPRESENTATION_ITEM ( '' )  );
#12303 = DIRECTION ( 'NONE',  ( 5.888300609747748832E-06, 9.662809622277729834E-06, -0.9999999999359791003 ) ) ;
#12304 = EDGE_CURVE ( 'NONE', #2214, #2300, #9596, .T. ) ;
#12305 = ORIENTED_EDGE ( 'NONE', *, *, #28308, .T. ) ;
#12306 = CARTESIAN_POINT ( 'NONE',  ( -20.33799833967064075, -7.952690384846734517, 70.35076722350379441 ) ) ;
#12307 = AXIS2_PLACEMENT_3D ( 'NONE', #16444, #46260, #20646 ) ;
#12308 = AXIS2_PLACEMENT_3D ( 'NONE', #45316, #46038, #8619 ) ;
#12309 = ORIENTED_EDGE ( 'NONE', *, *, #15457, .T. ) ;
#12310 = DIRECTION ( 'NONE',  ( 1.143861049860740968E-05, -2.837703139598260652E-06, 0.9999999999305527743 ) ) ;
#12311 = CARTESIAN_POINT ( 'NONE',  ( -11.06572510127579356, -10.92528991087847068, 57.32247810849851533 ) ) ;
#12312 = ORIENTED_EDGE ( 'NONE', *, *, #42830, .T. ) ;
#12313 = CARTESIAN_POINT ( 'NONE',  ( -24.46828707212341669, -14.45681828193256280, 70.06763959435293998 ) ) ;
#12314 = EDGE_CURVE ( 'NONE', #22864, #7039, #9223, .T. ) ;
#12315 = CARTESIAN_POINT ( 'NONE',  ( -10.28038339137012258, -12.69496154482620121, 64.46824888007303400 ) ) ;
#12316 = CARTESIAN_POINT ( 'NONE',  ( -18.73034385650551670, -9.794322478646142471, 51.19202720610083190 ) ) ;
#12317 = CARTESIAN_POINT ( 'NONE',  ( -12.02400249370662522, -10.35258068100519324, 71.15820205995147774 ) ) ;
#12318 = VECTOR ( 'NONE', #3084, 1000.000000000000000 ) ;
#12319 = CARTESIAN_POINT ( 'NONE',  ( -22.21277271144190379, -9.101880927996923276, 59.88204583602121289 ) ) ;
#12320 = DIRECTION ( 'NONE',  ( -0.3303050442826436228, 0.9438742382973701606, 3.829623549872328137E-09 ) ) ;
#12321 = ORIENTED_EDGE ( 'NONE', *, *, #34830, .T. ) ;
#12323 = DIRECTION ( 'NONE',  ( -3.484385612528001215E-15, 0.000000000000000000, 1.000000000000000000 ) ) ;
#12322 =( BOUNDED_CURVE ( )  B_SPLINE_CURVE ( 3, ( #1755, #16748, #20215, #43118 ),
 .UNSPECIFIED., .F., .F. ) 
 B_SPLINE_CURVE_WITH_KNOTS ( ( 4, 4 ),
 ( 6.081827386389258017, 6.283185307179586232 ),
 .UNSPECIFIED. ) 
 CURVE ( )  GEOMETRIC_REPRESENTATION_ITEM ( )  RATIONAL_B_SPLINE_CURVE ( ( 1.000000000000000000, 0.9966241020034161124, 0.9966241020034161124, 1.000000000000000000 ) ) 
 REPRESENTATION_ITEM ( '' )  );
#12324 = CARTESIAN_POINT ( 'NONE',  ( -10.76216126260078987, -17.12512740823429525, 65.04228012599854480 ) ) ;
#12325 = CARTESIAN_POINT ( 'NONE',  ( -15.43659385541290341, -8.995762431863383313, 51.38120296130602327 ) ) ;
#12326 = CARTESIAN_POINT ( 'NONE',  ( -12.96596342764269139, -9.347744029417796696, 71.14925352873375175 ) ) ;
#12327 = FACE_OUTER_BOUND ( 'NONE', #39644, .T. ) ;
#12328 = VERTEX_POINT ( 'NONE', #5281 ) ;
#12329 = ORIENTED_EDGE ( 'NONE', *, *, #48471, .T. ) ;
#12330 = EDGE_CURVE ( 'NONE', #30065, #19883, #20299, .T. ) ;
#12331 = B_SPLINE_CURVE_WITH_KNOTS ( 'NONE', 3,
 ( #18593, #41505, #10504, #3346, #29949, #18351, #22551, #7305, #3096, #3585 ),
 .UNSPECIFIED., .F., .F.,
 ( 4, 2, 2, 2, 4 ),
 ( 0.1272669073657954342, 0.2522669073488127967, 0.3772669073318302146, 0.5022669073148475771, 0.6272669072978649396 ),
 .UNSPECIFIED. ) ;
#12332 = CARTESIAN_POINT ( 'NONE',  ( -21.33694466872984918, -9.004932385753821933, 73.90128753631783809 ) ) ;
#12333 = ORIENTED_EDGE ( 'NONE', *, *, #12145, .F. ) ;
#12334 = CARTESIAN_POINT ( 'NONE',  ( -20.46316679850361808, -18.39244407412632043, 49.52966884056656482 ) ) ;
#12335 = CARTESIAN_POINT ( 'NONE',  ( -45.92409385541306932, -16.70920654474410938, 70.87000000000000455 ) ) ;
#12336 = CARTESIAN_POINT ( 'NONE',  ( -20.73950801051994119, -8.137571121906521654, 63.41147264556233409 ) ) ;
#12337 = EDGE_CURVE ( 'NONE', #4669, #31415, #43392, .T. ) ;
#12338 = CARTESIAN_POINT ( 'NONE',  ( -19.60046790782316251, -21.46228069541063732, 65.46486213989528835 ) ) ;
#12339 = CARTESIAN_POINT ( 'NONE',  ( -14.73037927113499812, -8.285490617698924254, 67.40407820626249702 ) ) ;
#12340 = CARTESIAN_POINT ( 'NONE',  ( -12.21223302309773651, -10.13625172099550475, 60.75021366515743182 ) ) ;
#12341 = CARTESIAN_POINT ( 'NONE',  ( -20.49170831689750472, -8.461258797198503601, 63.59649424907593129 ) ) ;
#12342 =( BOUNDED_CURVE ( )  B_SPLINE_CURVE ( 3, ( #41496, #23282, #45701, #7785 ),
 .UNSPECIFIED., .F., .F. ) 
 B_SPLINE_CURVE_WITH_KNOTS ( ( 4, 4 ),
 ( 0.5000000000000000000, 0.9074455897393670645 ),
 .UNSPECIFIED. ) 
 CURVE ( )  GEOMETRIC_REPRESENTATION_ITEM ( )  RATIONAL_B_SPLINE_CURVE ( ( 1.000000000000019540, 0.4567392136813334114, 0.3561768502900171107, 0.6983129098260917322 ) ) 
 REPRESENTATION_ITEM ( '' )  );
#12343 = VERTEX_POINT ( 'NONE', #43198 ) ;
#12344 = ADVANCED_FACE ( 'NONE', ( #31628 ), #5775, .T. ) ;
#12345 = CARTESIAN_POINT ( 'NONE',  ( -22.47245519635065492, -19.73066437834766873, 72.65872596779033188 ) ) ;
#12346 = CARTESIAN_POINT ( 'NONE',  ( -22.96375064570672819, -10.44813988596692411, 63.08658113699938497 ) ) ;
#12347 = CARTESIAN_POINT ( 'NONE',  ( -12.73044152958719977, -14.59664269629646505, 52.02966884056656482 ) ) ;
#12348 = CARTESIAN_POINT ( 'NONE',  ( -11.82099749022622426, -9.899105802180386604, 64.21409645106085406 ) ) ;
#12349 = EDGE_CURVE ( 'NONE', #28760, #9874, #8817, .T. ) ;
#12350 = ORIENTED_EDGE ( 'NONE', *, *, #34691, .T. ) ;
#12351 = VECTOR ( 'NONE', #34863, 1000.000000000000114 ) ;
#12352 = ORIENTED_EDGE ( 'NONE', *, *, #22439, .T. ) ;
#12353 = CARTESIAN_POINT ( 'NONE',  ( -20.03518388220226143, -21.78744935781895009, 72.59133997248245862 ) ) ;
#12354 = ORIENTED_EDGE ( 'NONE', *, *, #40281, .F. ) ;
#12355 = DIRECTION ( 'NONE',  ( 0.000000000000000000, -0.000000000000000000, 1.000000000000000000 ) ) ;
#12356 = CARTESIAN_POINT ( 'NONE',  ( -18.50846021547567233, -7.843058547566564620, 74.14064372603324671 ) ) ;
#12357 = AXIS2_PLACEMENT_3D ( 'NONE', #41249, #48383, #11956 ) ;
#12358 = EDGE_LOOP ( 'NONE', ( #33894, #21089 ) ) ;
#12359 = CARTESIAN_POINT ( 'NONE',  ( -42.54541738482483026, -14.80920654474415699, 62.02941176470587692 ) ) ;
#12360 = CARTESIAN_POINT ( 'NONE',  ( -18.30911350570762153, -7.811336752399037131, 74.04884132303362776 ) ) ;
#12361 = ORIENTED_EDGE ( 'NONE', *, *, #20395, .F. ) ;
#12362 = CARTESIAN_POINT ( 'NONE',  ( -15.94320239998165967, -7.507703417504081322, 63.80864474281522547 ) ) ;
#12363 = CARTESIAN_POINT ( 'NONE',  ( -23.82261068186806696, -17.64831283868447542, 62.77360983446511966 ) ) ;
#12364 = ORIENTED_EDGE ( 'NONE', *, *, #38846, .T. ) ;
#12365 = DIRECTION ( 'NONE',  ( 1.224646799147353207E-16, 1.000000000000000000, -1.912410701131276611E-32 ) ) ;
#12366 = EDGE_CURVE ( 'NONE', #15929, #42340, #33281, .T. ) ;
#12367 = CARTESIAN_POINT ( 'NONE',  ( -23.59327504554355315, -11.39630409041826020, 69.90682860766239060 ) ) ;
#12368 = ORIENTED_EDGE ( 'NONE', *, *, #3335, .T. ) ;
#12369 = LINE ( 'NONE', #26675, #20535 ) ;
#12370 = CARTESIAN_POINT ( 'NONE',  ( -16.71219989829967645, -22.22520177033091926, 68.81065352759269160 ) ) ;
#12371 = LINE ( 'NONE', #7980, #22647 ) ;
#12372 = ORIENTED_EDGE ( 'NONE', *, *, #4638, .F. ) ;
#12373 = CARTESIAN_POINT ( 'NONE',  ( -10.45994342254983778, -13.68936021814239012, 57.54005269860393668 ) ) ;
#12374 = CARTESIAN_POINT ( 'NONE',  ( -14.25068859620041017, -8.513811488652077486, 70.72957628655862550 ) ) ;
#12375 = CARTESIAN_POINT ( 'NONE',  ( -15.56465948913149333, -7.543361525925791788, 53.27966884056655061 ) ) ;
#12376 = CARTESIAN_POINT ( 'NONE',  ( -10.49754805884589004, -17.55449835891870691, 68.28377192865846723 ) ) ;
#12377 = CARTESIAN_POINT ( 'NONE',  ( -24.36823009493971171, -13.92613870693967293, 73.19559539736981435 ) ) ;
#12378 = DIRECTION ( 'NONE',  ( 1.261798975490001659E-05, -2.391811517362266964E-06, 0.9999999999175328558 ) ) ;
#12379 = CONICAL_SURFACE ( 'NONE', #26549, 3077.683537175336824, 1.256637061435925240 ) ;
#12380 = VECTOR ( 'NONE', #219, 1000.000000000000114 ) ;
#12381 = FACE_OUTER_BOUND ( 'NONE', #29272, .T. ) ;
#12382 = DIRECTION ( 'NONE',  ( -3.071710424422018668E-17, 6.404604876783312462E-16, 1.000000000000000000 ) ) ;
#12383 = CARTESIAN_POINT ( 'NONE',  ( -22.23351441301664622, -19.96811234597608120, 69.58906588434240348 ) ) ;
#12384 = CARTESIAN_POINT ( 'NONE',  ( -17.23659385650551812, -6.915538690918074494, 49.31353937987644542 ) ) ;
#12385 = VERTEX_POINT ( 'NONE', #29135 ) ;
#12386 = EDGE_CURVE ( 'NONE', #32100, #11419, #7234, .T. ) ;
#12387 = CARTESIAN_POINT ( 'NONE',  ( -14.03276184351355127, -20.98997801200527391, 71.92607724353423748 ) ) ;
#12388 = CARTESIAN_POINT ( 'NONE',  ( -24.28316357868862241, -16.20676250134670582, 59.23218348001186939 ) ) ;
#12389 = ORIENTED_EDGE ( 'NONE', *, *, #43570, .T. ) ;
#12390 = DIRECTION ( 'NONE',  ( 0.8447509909909731718, -0.5351595679979651576, 0.000000000000000000 ) ) ;
#12391 = CARTESIAN_POINT ( 'NONE',  ( -10.77430091989677408, -12.46723135102848090, 57.62297568056796848 ) ) ;
#12392 = VECTOR ( 'NONE', #11906, 1000.000000000000000 ) ;
#12393 = CARTESIAN_POINT ( 'NONE',  ( -12.26581428767149795, -15.78626943986449760, 49.52966884056655772 ) ) ;
#12394 = CARTESIAN_POINT ( 'NONE',  ( -24.34138173484706158, -16.17068648017255583, 62.59328676670276792 ) ) ;
#12395 = VERTEX_POINT ( 'NONE', #29377 ) ;
#12396 = CARTESIAN_POINT ( 'NONE',  ( -24.40668608927523309, -14.31499747486667573, 66.25580842628600919 ) ) ;
#12397 = DIRECTION ( 'NONE',  ( -1.006957036272130273E-05, 6.253991260048532259E-06, 0.9999999999297456421 ) ) ;
#12398 = EDGE_CURVE ( 'NONE', #40297, #3376, #29873, .T. ) ;
#12399 = CARTESIAN_POINT ( 'NONE',  ( -16.55451525393793233, -12.46531383050667863, 47.99999999999994316 ) ) ;
#12400 = ORIENTED_EDGE ( 'NONE', *, *, #2359, .F. ) ;
#12401 = CARTESIAN_POINT ( 'NONE',  ( -17.42409385541299471, -14.80920654474435771, 49.52966884056655772 ) ) ;
#12402 = EDGE_CURVE ( 'NONE', #35636, #18401, #28316, .T. ) ;
#12403 = CARTESIAN_POINT ( 'NONE',  ( -21.67055903134415473, -17.89628178023893668, 50.77966884056655772 ) ) ;
#12404 = PLANE ( 'NONE',  #42622 ) ;
#12405 = CARTESIAN_POINT ( 'NONE',  ( -24.46479343890040425, -14.44719913075708995, 66.48292729247951627 ) ) ;
#12406 = CARTESIAN_POINT ( 'NONE',  ( -22.78678303852979425, -9.565966637465477262, 53.49999999999994316 ) ) ;
#12407 = VERTEX_POINT ( 'NONE', #40453 ) ;
#12408 = VERTEX_POINT ( 'NONE', #6731 ) ;
#12409 = CARTESIAN_POINT ( 'NONE',  ( -20.27409385541304232, -6.859212275519751323, 50.50378509014259265 ) ) ;
#12410 = CARTESIAN_POINT ( 'NONE',  ( -22.94085434386056832, -9.802298134861713308, 70.19673941016031904 ) ) ;
#12411 = AXIS2_PLACEMENT_3D ( 'NONE', #30919, #23528, #34098 ) ;
#12412 = CARTESIAN_POINT ( 'NONE',  ( -14.03870967672415304, -8.172720116890397790, 70.91453050697840865 ) ) ;
#12413 = EDGE_CURVE ( 'NONE', #36713, #11687, #26568, .T. ) ;
#12414 = VECTOR ( 'NONE', #21641, 1000.000000000000000 ) ;
#12415 = AXIS2_PLACEMENT_3D ( 'NONE', #47444, #13677, #5608 ) ;
#12416 = EDGE_CURVE ( 'NONE', #48505, #31312, #32399, .T. ) ;
#12417 = CARTESIAN_POINT ( 'NONE',  ( -12.89447938415233175, -16.05746464591688749, 52.02966884056656482 ) ) ;
#12418 = EDGE_CURVE ( 'NONE', #36238, #2574, #6972, .T. ) ;
#12419 = CARTESIAN_POINT ( 'NONE',  ( -17.72634068467203505, -21.85272461955047874, 58.70553378267869249 ) ) ;
#12420 = CARTESIAN_POINT ( 'NONE',  ( -17.16915267636370146, -4.372400222636961153, 54.49999999999995026 ) ) ;
#12421 = VECTOR ( 'NONE', #2862, 1000.000000000000000 ) ;
#12422 = LINE ( 'NONE', #12900, #14663 ) ;
#12423 = ORIENTED_EDGE ( 'NONE', *, *, #14551, .T. ) ;
#12424 = CARTESIAN_POINT ( 'NONE',  ( -22.39933173914730702, -19.73341662423927190, 69.18920472232342433 ) ) ;
#12425 = VECTOR ( 'NONE', #299, 1000.000000000000114 ) ;
#12426 = CARTESIAN_POINT ( 'NONE',  ( -24.26711730922272281, -13.09851334671752632, 59.57087637770133171 ) ) ;
#12427 = ORIENTED_EDGE ( 'NONE', *, *, #3044, .F. ) ;
#12428 = CARTESIAN_POINT ( 'NONE',  ( -12.38457195078649598, -19.73934731251468477, 61.69678635356166296 ) ) ;
#12429 = CARTESIAN_POINT ( 'NONE',  ( -20.35208293893518672, -8.450992964911224092, 67.08104082230126153 ) ) ;
#12430 = VERTEX_POINT ( 'NONE', #25206 ) ;
#12431 = CARTESIAN_POINT ( 'NONE',  ( -13.71283467540607504, -11.09584481999758232, 49.52966884056655772 ) ) ;
#12432 = CARTESIAN_POINT ( 'NONE',  ( -21.94239013569476171, -20.22099906679998327, 58.76442899523448204 ) ) ;
#12433 = CARTESIAN_POINT ( 'NONE',  ( -24.03160971261424805, -17.26750559640275640, 69.71339792588547368 ) ) ;
#12434 = CARTESIAN_POINT ( 'NONE',  ( -19.30272045617997634, -8.014115550771091279, 59.96092997145632353 ) ) ;
#12435 = ORIENTED_EDGE ( 'NONE', *, *, #28012, .T. ) ;
#12436 = CARTESIAN_POINT ( 'NONE',  ( -10.33271527364436082, -17.09297260451290867, 57.79422236154066184 ) ) ;
#12437 = CARTESIAN_POINT ( 'NONE',  ( -17.75585263246644985, -22.25182633040162372, 58.50529758609160069 ) ) ;
#12438 = CARTESIAN_POINT ( 'NONE',  ( -45.92409385541306222, -14.20017296387473316, 71.05663168951063824 ) ) ;
#12439 = CARTESIAN_POINT ( 'NONE',  ( -18.37786432726835883, -21.79469297182707521, 69.10042588711679912 ) ) ;
#12440 = APPLICATION_PROTOCOL_DEFINITION ( 'draft international standard', 'automotive_design', 1998, #39771 ) ;
#12441 = DIRECTION ( 'NONE',  ( 1.000000000000000000, 2.866981220435666553E-17, 0.000000000000000000 ) ) ;
#12442 = DIRECTION ( 'NONE',  ( -6.919810407550069512E-06, -1.067025350021132924E-05, 0.9999999999191310218 ) ) ;
#12443 = DIRECTION ( 'NONE',  ( -3.071710424422018668E-17, 6.404604876783312462E-16, 1.000000000000000000 ) ) ;
#12444 = ORIENTED_EDGE ( 'NONE', *, *, #29177, .F. ) ;
#12445 = DIRECTION ( 'NONE',  ( 0.000000000000000000, 0.000000000000000000, 1.000000000000000000 ) ) ;
#12446 = VERTEX_POINT ( 'NONE', #36985 ) ;
#12447 = VECTOR ( 'NONE', #11807, 1000.000000000000000 ) ;
#12448 = DIRECTION ( 'NONE',  ( -3.071710424422018668E-17, 6.404604876783312462E-16, 1.000000000000000000 ) ) ;
#12449 = CARTESIAN_POINT ( 'NONE',  ( -13.14999064602648637, -9.265557826385967033, 67.37942786034257381 ) ) ;
#12450 = ORIENTED_EDGE ( 'NONE', *, *, #13071, .F. ) ;
#12451 = CARTESIAN_POINT ( 'NONE',  ( -19.97164249076357478, -21.81019033462135326, 69.11977790463622284 ) ) ;
#12452 = AXIS2_PLACEMENT_3D ( 'NONE', #2627, #28734, #39812 ) ;
#12453 = FACE_BOUND ( 'NONE', #8399, .T. ) ;
#12454 = EDGE_CURVE ( 'NONE', #26524, #37287, #18276, .T. ) ;
#12455 = VERTEX_POINT ( 'NONE', #17556 ) ;
#12456 = ORIENTED_EDGE ( 'NONE', *, *, #12549, .T. ) ;
#12457 = EDGE_LOOP ( 'NONE', ( #21841, #41436, #31569, #40622, #45587, #20866, #6044, #29393, #43096, #19202, #5510, #38212, #6578, #5875, #6450, #23175, #6341, #23801, #187, #26177, #42029, #43396, #32480, #18383, #39046, #12372 ) ) ;
#12458 = DIRECTION ( 'NONE',  ( -0.9524241471993248886, 0.0009228828802118167144, -0.3047743298226213704 ) ) ;
#12459 = CARTESIAN_POINT ( 'NONE',  ( -11.60006209888454443, -10.16330164164447325, 71.08397698276321819 ) ) ;
#12460 =( BOUNDED_CURVE ( )  B_SPLINE_CURVE ( 3, ( #33481, #17743, #44603, #14040 ),
 .UNSPECIFIED., .F., .F. ) 
 B_SPLINE_CURVE_WITH_KNOTS ( ( 4, 4 ),
 ( 0.5000000000000000000, 0.9074455897393702841 ),
 .UNSPECIFIED. ) 
 CURVE ( )  GEOMETRIC_REPRESENTATION_ITEM ( )  RATIONAL_B_SPLINE_CURVE ( ( 1.000000000000006661, 0.4567392136813283043, 0.3561768502900239941, 0.6983129098261012802 ) ) 
 REPRESENTATION_ITEM ( '' )  );
#12461 = CARTESIAN_POINT ( 'NONE',  ( -21.27276468869498416, -8.962107285475900298, 73.61631126181501372 ) ) ;
#12462 = CARTESIAN_POINT ( 'NONE',  ( -10.61641583932764910, -11.78277314028518319, 74.74335662173743344 ) ) ;
#12463 = CARTESIAN_POINT ( 'NONE',  ( -16.32745258320347759, -21.77369344365219561, 61.77040269689842944 ) ) ;
#12464 = VERTEX_POINT ( 'NONE', #33282 ) ;
#12465 = ORIENTED_EDGE ( 'NONE', *, *, #40310, .F. ) ;
#12466 = CARTESIAN_POINT ( 'NONE',  ( -22.16159385650551528, -9.295667164867525756, 49.30633214617472504 ) ) ;
#12467 = LINE ( 'NONE', #38568, #17321 ) ;
#12468 = CYLINDRICAL_SURFACE ( 'NONE', #26813, 0.1499999999999998834 ) ;
#12469 = CARTESIAN_POINT ( 'NONE',  ( -17.42409385541300892, -14.80920654474439324, 56.49999999999994316 ) ) ;
#12470 = VERTEX_POINT ( 'NONE', #44648 ) ;
#12471 = CARTESIAN_POINT ( 'NONE',  ( -21.88034385650551883, -6.424090610841176385, 49.80797279389977916 ) ) ;
#12472 =( BOUNDED_CURVE ( )  B_SPLINE_CURVE ( 3, ( #46735, #13208, #9069, #20635 ),
 .UNSPECIFIED., .F., .F. ) 
 B_SPLINE_CURVE_WITH_KNOTS ( ( 4, 4 ),
 ( 0.9074455897393662873, 1.000000000000000000 ),
 .UNSPECIFIED. ) 
 CURVE ( )  GEOMETRIC_REPRESENTATION_ITEM ( )  RATIONAL_B_SPLINE_CURVE ( ( 0.6983129098260957290, 0.7760317562607005337, 0.8765941196520019574, 1.000000000000000000 ) ) 
 REPRESENTATION_ITEM ( '' )  );
#12473 = EDGE_CURVE ( 'NONE', #28707, #29774, #38042, .T. ) ;
#12474 = EDGE_LOOP ( 'NONE', ( #14443, #45831, #45823, #8018 ) ) ;
#12475 = EDGE_CURVE ( 'NONE', #43128, #17100, #10910, .T. ) ;
#12476 = EDGE_CURVE ( 'NONE', #28650, #44593, #40090, .T. ) ;
#12477 = CARTESIAN_POINT ( 'NONE',  ( -14.80056147340629380, -21.78207226143426922, 61.82095877133116346 ) ) ;
#12478 = DIRECTION ( 'NONE',  ( 0.000000000000000000, 0.000000000000000000, -1.000000000000000000 ) ) ;
#12479 = AXIS2_PLACEMENT_3D ( 'NONE', #34230, #34730, #15758 ) ;
#12480 = FACE_OUTER_BOUND ( 'NONE', #18505, .T. ) ;
#12481 = VECTOR ( 'NONE', #37147, 1000.000000000000114 ) ;
#12482 = ORIENTED_EDGE ( 'NONE', *, *, #37278, .F. ) ;
#12483 = CARTESIAN_POINT ( 'NONE',  ( -15.39388989008627995, -21.97733388496078177, 72.23070757706680922 ) ) ;
#12484 = CIRCLE ( 'NONE', #35250, 1.999999999999999112 ) ;
#12485 = VECTOR ( 'NONE', #38704, 999.9999999999998863 ) ;
#12486 = LINE ( 'NONE', #1157, #36150 ) ;
#12487 = CARTESIAN_POINT ( 'NONE',  ( -23.78676187654788521, -10.93361199230012559, 73.54688693628270357 ) ) ;
#12488 = CARTESIAN_POINT ( 'NONE',  ( -22.83578998848691199, -19.92954559311242235, 72.76587817586035101 ) ) ;
#12489 = ORIENTED_EDGE ( 'NONE', *, *, #39975, .T. ) ;
#12490 = VECTOR ( 'NONE', #45947, 1000.000000000000114 ) ;
#12491 = DIRECTION ( 'NONE',  ( 0.000000000000000000, 0.000000000000000000, 1.000000000000000000 ) ) ;
#12492 = CYLINDRICAL_SURFACE ( 'NONE', #21293, 2.000000000000001776 ) ;
#12493 = CARTESIAN_POINT ( 'NONE',  ( -20.10953249554714262, -7.859859036490854045, 73.88130001012858372 ) ) ;
#12494 = VERTEX_POINT ( 'NONE', #22476 ) ;
#12495 = LINE ( 'NONE', #24319, #25176 ) ;
#12496 = VERTEX_POINT ( 'NONE', #26661 ) ;
#12497 = CARTESIAN_POINT ( 'NONE',  ( -14.99555751708010121, -21.85235056220836469, 65.14950770721691242 ) ) ;
#12498 = FACE_OUTER_BOUND ( 'NONE', #32877, .T. ) ;
#12499 = EDGE_LOOP ( 'NONE', ( #21277, #24710, #45320, #24050, #45063 ) ) ;
#12500 = CARTESIAN_POINT ( 'NONE',  ( -16.18802525292456096, -21.75305063948447426, 62.17057002965735535 ) ) ;
#12502 = EDGE_CURVE ( 'NONE', #14825, #39482, #15799, .T. ) ;
#12501 = CARTESIAN_POINT ( 'NONE',  ( -10.81170448216924740, -12.36318809540519048, 57.34329390664808557 ) ) ;
#12503 = CARTESIAN_POINT ( 'NONE',  ( -10.56492483649129710, -13.18000429128331774, 71.50828586225090078 ) ) ;
#12504 = FACE_OUTER_BOUND ( 'NONE', #31192, .T. ) ;
#12505 = VERTEX_POINT ( 'NONE', #557 ) ;
#12506 = CARTESIAN_POINT ( 'NONE',  ( -24.21013527259002629, -17.88545513683227384, 59.11723130990997532 ) ) ;
#12507 = CARTESIAN_POINT ( 'NONE',  ( -20.64758772760614036, -8.594144261551539543, 63.53951371574645179 ) ) ;
#12508 = FACE_OUTER_BOUND ( 'NONE', #25603, .T. ) ;
#12509 = CARTESIAN_POINT ( 'NONE',  ( -22.28399030946148329, -9.162456282157330989, 59.84454312193096825 ) ) ;
#12510 = ORIENTED_EDGE ( 'NONE', *, *, #24641, .T. ) ;
#12511 = DIRECTION ( 'NONE',  ( -3.071710424422018668E-17, 6.404604876783312462E-16, 1.000000000000000000 ) ) ;
#12512 = CARTESIAN_POINT ( 'NONE',  ( -24.72860576188992709, -16.27458831476113943, 62.78667002183767210 ) ) ;
#12513 = VERTEX_POINT ( 'NONE', #27142 ) ;
#12514 = ORIENTED_EDGE ( 'NONE', *, *, #21062, .T. ) ;
#12515 = CARTESIAN_POINT ( 'NONE',  ( -13.01482893870565682, -8.804038099563683772, 63.95300575187839343 ) ) ;
#12516 = EDGE_CURVE ( 'NONE', #1995, #8331, #14430, .T. ) ;
#12517 = CARTESIAN_POINT ( 'NONE',  ( -11.03161394367693049, -18.63672047605813376, 57.92059234540772650 ) ) ;
#12518 = CARTESIAN_POINT ( 'NONE',  ( -12.88034385759799250, -9.360768649639302552, 51.01397948905922419 ) ) ;
#12519 = CARTESIAN_POINT ( 'NONE',  ( -12.35460334350678480, -9.982084953531975557, 57.16223665588471192 ) ) ;
#12520 = LINE ( 'NONE', #5388, #23613 ) ;
#12521 = CARTESIAN_POINT ( 'NONE',  ( -23.30282330091471366, -18.60927750845715067, 69.29371984660140527 ) ) ;
#12522 = AXIS2_PLACEMENT_3D ( 'NONE', #17215, #12804, #43092 ) ;
#12523 = FACE_OUTER_BOUND ( 'NONE', #7819, .T. ) ;
#12524 = VERTEX_POINT ( 'NONE', #23455 ) ;
#12525 = ORIENTED_EDGE ( 'NONE', *, *, #1771, .T. ) ;
#12526 = CARTESIAN_POINT ( 'NONE',  ( -10.64577699202231287, -11.71757285455929853, 74.67344842241411129 ) ) ;
#12527 = CARTESIAN_POINT ( 'NONE',  ( 0.000000000000000000, 0.000000000000000000, 0.000000000000000000 ) ) ;
#12528 = DIRECTION ( 'NONE',  ( -3.071710424422018668E-17, 6.404604876783312462E-16, 1.000000000000000000 ) ) ;
#12529 = VECTOR ( 'NONE', #3797, 1000.000000000000114 ) ;
#12530 = FACE_OUTER_BOUND ( 'NONE', #13264, .T. ) ;
#12531 = DIRECTION ( 'NONE',  ( 2.866981220435666553E-17, -1.000000000000000000, -1.190614954331866791E-16 ) ) ;
#12532 = EDGE_LOOP ( 'NONE', ( #15736, #18352, #18717, #31507, #18919 ) ) ;
#12533 = EDGE_CURVE ( 'NONE', #6805, #21796, #45379, .T. ) ;
#12534 = ADVANCED_FACE ( 'NONE', ( #18775 ), #4018, .F. ) ;
#12535 = DIRECTION ( 'NONE',  ( 0.000000000000000000, 0.000000000000000000, -1.000000000000000000 ) ) ;
#12536 = FACE_OUTER_BOUND ( 'NONE', #38813, .T. ) ;
#12537 = FACE_OUTER_BOUND ( 'NONE', #1128, .T. ) ;
#12538 = CARTESIAN_POINT ( 'NONE',  ( -15.79779810604033408, -7.538871719435400465, 67.34018486351625654 ) ) ;
#12539 = ORIENTED_EDGE ( 'NONE', *, *, #47400, .T. ) ;
#12540 = CARTESIAN_POINT ( 'NONE',  ( -13.10125976363765332, -9.301846226610548385, 71.07755262771341620 ) ) ;
#12541 = EDGE_CURVE ( 'NONE', #46061, #43599, #24837, .T. ) ;
#12542 = EDGE_CURVE ( 'NONE', #15202, #48304, #41260, .T. ) ;
#12543 = LINE ( 'NONE', #31258, #3919 ) ;
#12544 = ORIENTED_EDGE ( 'NONE', *, *, #30460, .F. ) ;
#12545 = EDGE_CURVE ( 'NONE', #37822, #48265, #21313, .T. ) ;
#12546 = VECTOR ( 'NONE', #21155, 1000.000000000000000 ) ;
#12547 =( BOUNDED_CURVE ( )  B_SPLINE_CURVE ( 3, ( #23922, #47296, #39415, #20468 ),
 .UNSPECIFIED., .F., .F. ) 
 B_SPLINE_CURVE_WITH_KNOTS ( ( 4, 4 ),
 ( 0.5000000000000000000, 0.9074455897393658432 ),
 .UNSPECIFIED. ) 
 CURVE ( )  GEOMETRIC_REPRESENTATION_ITEM ( )  RATIONAL_B_SPLINE_CURVE ( ( 0.9999999999999861222, 0.4567392136813359649, 0.3561768502900413691, 0.6983129098260872913 ) ) 
 REPRESENTATION_ITEM ( '' )  );
#12548 = CARTESIAN_POINT ( 'NONE',  ( -11.14029015952437263, -10.80702246001832023, 57.46549161190092292 ) ) ;
#12549 = EDGE_CURVE ( 'NONE', #36492, #300, #11317, .T. ) ;
#12550 = DIRECTION ( 'NONE',  ( -2.866981220435666553E-17, 1.000000000000000000, 1.190614954331866791E-16 ) ) ;
#12551 = ORIENTED_EDGE ( 'NONE', *, *, #27819, .T. ) ;
#12552 = DIRECTION ( 'NONE',  ( 0.000000000000000000, -0.8949343913984053600, -0.4461977533475104396 ) ) ;
#12553 = AXIS2_PLACEMENT_3D ( 'NONE', #16252, #28340, #16978 ) ;
#12554 = ORIENTED_EDGE ( 'NONE', *, *, #40667, .T. ) ;
#12555 = DIRECTION ( 'NONE',  ( -0.2466764125338440639, -0.9690979039805150963, 7.162324212089591066E-08 ) ) ;
#12556 = CARTESIAN_POINT ( 'NONE',  ( -21.08681864223905578, -8.776014225774568800, 73.75695571861821520 ) ) ;
#12557 = ORIENTED_EDGE ( 'NONE', *, *, #3390, .F. ) ;
#12558 = CARTESIAN_POINT ( 'NONE',  ( -24.26499744607890818, -17.75976858747020160, 62.65856309191605789 ) ) ;
#12559 = CYLINDRICAL_SURFACE ( 'NONE', #24246, 0.1499999999999964140 ) ;
#12560 = EDGE_CURVE ( 'NONE', #17265, #17004, #41190, .T. ) ;
#12561 = CARTESIAN_POINT ( 'NONE',  ( -18.56159385650551741, -9.295667164867525756, 49.30633214617472504 ) ) ;
#12562 = CARTESIAN_POINT ( 'NONE',  ( -24.06787342886325121, -18.28917680027896608, 54.27966884056654351 ) ) ;
#12563 = AXIS2_PLACEMENT_3D ( 'NONE', #3181, #37137, #48478 ) ;
#12564 = B_SPLINE_CURVE_WITH_KNOTS ( 'NONE', 3,
 ( #25172, #29838, #22201, #10869, #14048, #13813, #29342, #18484, #37188, #48053 ),
 .UNSPECIFIED., .F., .F.,
 ( 4, 2, 2, 2, 4 ),
 ( 0.000000000000000000, 0.2500000000000000000, 0.5000000000000000000, 0.7500000000000000000, 1.000000000000000000 ),
 .UNSPECIFIED. ) ;
#12565 = CARTESIAN_POINT ( 'NONE',  ( -10.62638924718675248, -11.76062588693173794, 74.75828993396721955 ) ) ;
#12566 = PLANE ( 'NONE',  #47069 ) ;
#12567 = ORIENTED_EDGE ( 'NONE', *, *, #28012, .F. ) ;
#12568 = CYLINDRICAL_SURFACE ( 'NONE', #22374, 4.686499999999997002 ) ;
#12569 = DIRECTION ( 'NONE',  ( -3.071710424422018668E-17, 6.404604876783312462E-16, 1.000000000000000000 ) ) ;
#12570 = CARTESIAN_POINT ( 'NONE',  ( -14.98927377128279304, -8.246306944878789125, 56.49999999999994316 ) ) ;
#12571 = CARTESIAN_POINT ( 'NONE',  ( -24.61022370753789090, -12.84395140709443162, 66.40272499809746876 ) ) ;
#12572 = CARTESIAN_POINT ( 'NONE',  ( -20.69990174146486694, -20.99685511590434217, 62.34301292963910157 ) ) ;
#12573 = VERTEX_POINT ( 'NONE', #9163 ) ;
#12574 = VERTEX_POINT ( 'NONE', #28105 ) ;
#12575 = DIRECTION ( 'NONE',  ( -0.8875028193683940358, -0.4608022847308269609, 4.020963237607658939E-08 ) ) ;
#12576 = DIRECTION ( 'NONE',  ( 0.6621635203543605463, 0.7493593746073505812, 2.316976118889565779E-08 ) ) ;
#12577 = ORIENTED_EDGE ( 'NONE', *, *, #13609, .T. ) ;
#12578 = CARTESIAN_POINT ( 'NONE',  ( -22.58763249286555208, -20.18056880150341215, 65.81766459098905386 ) ) ;
#12579 = DIRECTION ( 'NONE',  ( 2.403795750412638671E-06, 2.069898558110202305E-06, 0.9999999999949686913 ) ) ;
#12580 = DIRECTION ( 'NONE',  ( 0.9687793358424822143, -0.2479245821708672415, 0.000000000000000000 ) ) ;
#12581 = CARTESIAN_POINT ( 'NONE',  ( -10.42462062184586635, -14.89508117765250361, 75.09778901762284420 ) ) ;
#12582 = CARTESIAN_POINT ( 'NONE',  ( -10.63483670088760924, -17.87674068094334245, 71.75213521449022380 ) ) ;
#12583 = CARTESIAN_POINT ( 'NONE',  ( -10.89237721494850142, -17.47219765205588615, 71.86718162093610829 ) ) ;
#12584 = ORIENTED_EDGE ( 'NONE', *, *, #27608, .F. ) ;
#12585 = CARTESIAN_POINT ( 'NONE',  ( -22.65122241358830024, -10.07311426451252956, 66.75002127378915873 ) ) ;
#12586 = DIRECTION ( 'NONE',  ( 0.9687793358424821033, -0.2479245821708677133, 0.000000000000000000 ) ) ;
#12587 = AXIS2_PLACEMENT_3D ( 'NONE', #30745, #5612, #12252 ) ;
#12588 = CARTESIAN_POINT ( 'NONE',  ( -12.27729925481933471, -9.991218852276041673, 60.55918086709623083 ) ) ;
#12589 = CARTESIAN_POINT ( 'NONE',  ( -12.56076107774658723, -9.694232635630330108, 74.47489936300191005 ) ) ;
#12590 = ADVANCED_FACE ( 'NONE', ( #23942 ), #38705, .T. ) ;
#12591 = CIRCLE ( 'NONE', #40118, 1.999999999999999112 ) ;
#12592 = ORIENTED_EDGE ( 'NONE', *, *, #19217, .T. ) ;
#12593 = EDGE_LOOP ( 'NONE', ( #42237, #20653, #40778, #24091 ) ) ;
#12594 = ORIENTED_EDGE ( 'NONE', *, *, #47060, .T. ) ;
#12595 = EDGE_CURVE ( 'NONE', #37558, #44222, #1769, .T. ) ;
#12596 = CARTESIAN_POINT ( 'NONE',  ( 18.46573386768564973, 2.144455078683989768, 49.30629848276630156 ) ) ;
#12597 = CARTESIAN_POINT ( 'NONE',  ( -24.07263600646086132, -12.61902678358097063, 69.88128981831194153 ) ) ;
#12598 = VECTOR ( 'NONE', #21734, 1000.000000000000114 ) ;
#12599 =( BOUNDED_SURFACE ( )  B_SPLINE_SURFACE ( 3, 1, ( 
 ( #4160, #26072 ),
 ( #41827, #33668 ),
 ( #19159, #34167 ),
 ( #15693, #8101 ),
 ( #48711, #37365 ),
 ( #4384, #38104 ),
 ( #30510, #34405 ) ),
 .UNSPECIFIED., .T., .F., .F. ) 
 B_SPLINE_SURFACE_WITH_KNOTS ( ( 4, 3, 4 ),
 ( 2, 2 ),
 ( 0.000000000000000000, 0.5000000000000000000, 1.000000000000000000 ),
 ( 0.000000000000000000, 1.000000000000000000 ),
 .UNSPECIFIED. ) 
 GEOMETRIC_REPRESENTATION_ITEM ( )  RATIONAL_B_SPLINE_SURFACE ( (
 ( 1.000000000000000000, 1.000000000000000000),
 ( 0.3333333333333335369, 0.3333333333333330373),
 ( 0.3333333333333335369, 0.3333333333333330373),
 ( 1.000000000000000000, 1.000000000000000000),
 ( 0.3333333333333333703, 0.3333333333333333703),
 ( 0.3333333333333333703, 0.3333333333333333703),
 ( 1.000000000000000000, 1.000000000000000000) ) ) 
 REPRESENTATION_ITEM ( '' )  SURFACE ( )  );
#12600 = ORIENTED_EDGE ( 'NONE', *, *, #30501, .T. ) ;
#12601 = DIRECTION ( 'NONE',  ( -2.866981220435666553E-17, 1.000000000000000000, 1.190614954331866791E-16 ) ) ;
#12602 = FACE_OUTER_BOUND ( 'NONE', #22502, .T. ) ;
#12603 = CLOSED_SHELL ( 'NONE', ( #7942, #3398, #6308, #44340, #32890, #34737, #19150, #10499, #17965, #26228, #13250, #46307, #5210, #32344, #32139, #39474, #18821, #44812, #17304, #33813, #17086, #3977, #26468, #37968, #3255, #5267, #13327, #22438, #35948, #9222, #18316, #20053, #41053, #40488, #43718, #29344, #47476, #42224, #14680, #7946, #44526, #28777, #43002, #15577, #30564, #19573, #44740, #25041, #40287, #11676, #36193, #46999, #17844, #44714, #12150, #2502, #19496, #4555, #24387, #22861, #31568, #16689, #29404, #11746, #46084, #6054, #2077, #38549, #30902, #30771, #46782, #41978, #25491, #10286, #14201, #19827, #20591, #12663, #33709, #33713 ) ) ;
#12604 = ORIENTED_EDGE ( 'NONE', *, *, #30706, .F. ) ;
#12605 = ADVANCED_FACE ( 'NONE', ( #43130 ), #5223, .T. ) ;
#12606 = CARTESIAN_POINT ( 'NONE',  ( -10.63794491530182640, -17.88370890602386609, 71.74435113740163672 ) ) ;
#12607 = DIRECTION ( 'NONE',  ( -3.071710424422018668E-17, 6.404604876783312462E-16, 1.000000000000000000 ) ) ;
#12608 = EDGE_CURVE ( 'NONE', #39039, #7306, #38858, .T. ) ;
#12609 = EDGE_LOOP ( 'NONE', ( #968, #42057 ) ) ;
#12610 = CARTESIAN_POINT ( 'NONE',  ( -4.924093855413054222, -6.359206544744109735, 63.99999999999998579 ) ) ;
#12611 =( BOUNDED_CURVE ( )  B_SPLINE_CURVE ( 3, ( #1747, #24155, #35941, #38921 ),
 .UNSPECIFIED., .F., .F. ) 
 B_SPLINE_CURVE_WITH_KNOTS ( ( 4, 4 ),
 ( 0.4074455897393705062, 0.5000000000000000000 ),
 .UNSPECIFIED. ) 
 CURVE ( )  GEOMETRIC_REPRESENTATION_ITEM ( )  RATIONAL_B_SPLINE_CURVE ( ( 0.6983129098261044998, 0.7760317562607099706, 0.8765941196520091738, 1.000000000000003109 ) ) 
 REPRESENTATION_ITEM ( '' )  );
#12612 = CARTESIAN_POINT ( 'NONE',  ( -10.58350140945814744, -13.32355762376674768, 71.43501841499802651 ) ) ;
#12613 = ORIENTED_EDGE ( 'NONE', *, *, #39616, .T. ) ;
#12614 = CYLINDRICAL_SURFACE ( 'NONE', #75, 0.1499999999999973577 ) ;
#12615 = CARTESIAN_POINT ( 'NONE',  ( -16.45013838383832550, -21.79965580723203189, 68.83993634381745608 ) ) ;
#12616 = CARTESIAN_POINT ( 'NONE',  ( -19.42896739221782809, -21.56812523091048206, 62.29503644570711174 ) ) ;
#12617 = VERTEX_POINT ( 'NONE', #35963 ) ;
#12618 = CARTESIAN_POINT ( 'NONE',  ( -50.42609385541305755, -14.90920654474413887, 60.01764705882352047 ) ) ;
#12619 = CARTESIAN_POINT ( 'NONE',  ( -22.27985548098255109, -20.46033401586769429, 58.87787560672637710 ) ) ;
#12620 = AXIS2_PLACEMENT_3D ( 'NONE', #28964, #6568, #36565 ) ;
#12621 = EDGE_CURVE ( 'NONE', #17138, #3477, #4405, .T. ) ;
#12622 = CARTESIAN_POINT ( 'NONE',  ( -14.53530919737752924, -21.67646582726403182, 58.34430615535840303 ) ) ;
#12623 = CARTESIAN_POINT ( 'NONE',  ( 23.52590614458706852, 1.890747609047893185, 50.53028072113869484 ) ) ;
#12624 = CARTESIAN_POINT ( 'NONE',  ( -17.54909385759799179, -8.112991634885936776, 51.74999426922421719 ) ) ;
#12625 = VECTOR ( 'NONE', #43186, 1000.000000000000000 ) ;
#12626 = DIRECTION ( 'NONE',  ( -3.071710424422018668E-17, 6.404604876783312462E-16, 1.000000000000000000 ) ) ;
#12627 =( BOUNDED_CURVE ( )  B_SPLINE_CURVE ( 3, ( #22581, #37577, #1133, #46452 ),
 .UNSPECIFIED., .F., .F. ) 
 B_SPLINE_CURVE_WITH_KNOTS ( ( 4, 4 ),
 ( 0.5000000000000000000, 0.9074455897393668424 ),
 .UNSPECIFIED. ) 
 CURVE ( )  GEOMETRIC_REPRESENTATION_ITEM ( )  RATIONAL_B_SPLINE_CURVE ( ( 0.9999999999999977796, 0.4567392136813193115, 0.3561768502900270472, 0.6983129098261184886 ) ) 
 REPRESENTATION_ITEM ( '' )  );
#12628 = DIRECTION ( 'NONE',  ( -1.224646799147353207E-16, -1.000000000000000000, 1.912410701131276611E-32 ) ) ;
#12629 = DIRECTION ( 'NONE',  ( 1.000000000000000000, 0.000000000000000000, 0.000000000000000000 ) ) ;
#12630 = DIRECTION ( 'NONE',  ( 1.000000000000000000, -1.224646799147353207E-16, 3.142942573426604379E-15 ) ) ;
#12631 = CARTESIAN_POINT ( 'NONE',  ( -17.68659385650551741, -9.302874398569244363, 51.68646062012417985 ) ) ;
#12632 = VERTEX_POINT ( 'NONE', #31318 ) ;
#12633 = CARTESIAN_POINT ( 'NONE',  ( -10.42544315765747420, -13.95862937692757555, 57.74265221125428837 ) ) ;
#12634 = CYLINDRICAL_SURFACE ( 'NONE', #17889, 1.999999999999999556 ) ;
#12635 = EDGE_LOOP ( 'NONE', ( #41031, #30639, #13782, #30137, #40673 ) ) ;
#12636 = FACE_OUTER_BOUND ( 'NONE', #40251, .T. ) ;
#12637 = CARTESIAN_POINT ( 'NONE',  ( -15.01040879766030223, -21.85754770930110880, 65.24450189717120452 ) ) ;
#12638 = ADVANCED_BREP_SHAPE_REPRESENTATION ( '', ( #48569, #29031 ), #39238 ) ;
#12639 = CARTESIAN_POINT ( 'NONE',  ( -16.17130706675677132, -22.15324536104840547, 58.46302426628946591 ) ) ;
#12640 = CARTESIAN_POINT ( 'NONE',  ( -22.62394951084894146, -10.04809318868971424, 70.29706442286226320 ) ) ;
#12641 = CARTESIAN_POINT ( 'NONE',  ( -21.31115985637654120, -8.927249709250720144, 73.88656608925673197 ) ) ;
#12642 = ORIENTED_EDGE ( 'NONE', *, *, #21237, .T. ) ;
#12643 = CARTESIAN_POINT ( 'NONE',  ( -13.35550429318260512, -8.568184490765622385, 57.15463139269148485 ) ) ;
#12644 = CARTESIAN_POINT ( 'NONE',  ( -17.81160558974999830, -14.71003671187606088, 53.27966884056655061 ) ) ;
#12645 = CARTESIAN_POINT ( 'NONE',  ( -12.23301264461619553, -10.03852782535897958, 60.84446034103241630 ) ) ;
#12646 = EDGE_LOOP ( 'NONE', ( #10970, #34606 ) ) ;
#12647 = AXIS2_PLACEMENT_3D ( 'NONE', #21810, #18344, #39379 ) ;
#12648 = CARTESIAN_POINT ( 'NONE',  ( -18.52137898189696230, -22.17812618198155761, 72.42477605357316861 ) ) ;
#12649 = CARTESIAN_POINT ( 'NONE',  ( -23.85748962928175132, -11.92509172808648543, 59.49707787073156595 ) ) ;
#12650 = CARTESIAN_POINT ( 'NONE',  ( -24.55871722839809834, -12.66422925090921225, 69.88747596251579353 ) ) ;
#12651 = ADVANCED_FACE ( 'NONE', ( #12602 ), #3094, .T. ) ;
#12652 = CARTESIAN_POINT ( 'NONE',  ( -21.73098984888145679, -8.730191469543168381, 70.31627926275058371 ) ) ;
#12653 = FACE_OUTER_BOUND ( 'NONE', #7225, .T. ) ;
#12654 = ORIENTED_EDGE ( 'NONE', *, *, #45154, .T. ) ;
#12655 = VERTEX_POINT ( 'NONE', #35002 ) ;
#12656 = CARTESIAN_POINT ( 'NONE',  ( -22.80534385541304232, -7.595227055684746986, 51.75156210489594599 ) ) ;
#12657 = VECTOR ( 'NONE', #13721, 1000.000000000000000 ) ;
#12658 = CARTESIAN_POINT ( 'NONE',  ( -24.40658449907487793, -15.78251210865724907, 69.53307488410803217 ) ) ;
#12659 = CARTESIAN_POINT ( 'NONE',  ( -17.72612443559818018, -7.765381109175947927, 60.36588690973874094 ) ) ;
#12660 = DIRECTION ( 'NONE',  ( 1.224646799147353207E-16, 1.000000000000000000, -1.912410701131276611E-32 ) ) ;
#12661 = CARTESIAN_POINT ( 'NONE',  ( -24.31561971792381982, -17.63961254754600816, 66.12169969450457074 ) ) ;
#12662 = ORIENTED_EDGE ( 'NONE', *, *, #44201, .F. ) ;
#12663 = ADVANCED_FACE ( 'NONE', ( #2003 ), #16998, .F. ) ;
#12664 = CARTESIAN_POINT ( 'NONE',  ( 8.575906144586950219, -6.109215713985405749, 50.50605614422795497 ) ) ;
#12665 = FACE_OUTER_BOUND ( 'NONE', #504, .T. ) ;
#12666 = EDGE_CURVE ( 'NONE', #14945, #30767, #28361, .T. ) ;
#12667 = EDGE_LOOP ( 'NONE', ( #45907, #38084, #17334, #7349, #19064 ) ) ;
#12668 = CARTESIAN_POINT ( 'NONE',  ( -24.21013527259002629, -17.88545513683227384, 59.11723130990997532 ) ) ;
#12669 = CARTESIAN_POINT ( 'NONE',  ( -17.15681863660994821, -7.812702811906586220, 74.07091344620687323 ) ) ;
#12670 = ORIENTED_EDGE ( 'NONE', *, *, #37212, .F. ) ;
#12671 = EDGE_CURVE ( 'NONE', #16961, #8530, #36730, .T. ) ;
#12672 = CARTESIAN_POINT ( 'NONE',  ( -13.35819042472069107, -21.05197888995676436, 61.70141705377209007 ) ) ;
#12673 = CARTESIAN_POINT ( 'NONE',  ( -15.03427660820159772, -21.44211488324610571, 65.12068745241758450 ) ) ;
#12674 = ORIENTED_EDGE ( 'NONE', *, *, #6406, .F. ) ;
#12675 = CARTESIAN_POINT ( 'NONE',  ( -10.50893933415051507, -13.43540278197273885, 74.96345540680638919 ) ) ;
#12676 = AXIS2_PLACEMENT_3D ( 'NONE', #34656, #27031, #42298 ) ;
#12677 = DIRECTION ( 'NONE',  ( -0.9710973231077276724, 0.2386838684389876730, -7.431671637556418335E-08 ) ) ;
#12678 = ADVANCED_FACE ( 'NONE', ( #39672 ), #8160, .T. ) ;
#12679 = EDGE_CURVE ( 'NONE', #42061, #21742, #7165, .T. ) ;
#12680 = CARTESIAN_POINT ( 'NONE',  ( -21.78783678618839303, -8.770877803870156697, 70.38778484029896276 ) ) ;
#12681 = CARTESIAN_POINT ( 'NONE',  ( -22.50978241177926975, -19.61935080069436665, 72.64400553400905380 ) ) ;
#12682 = ORIENTED_EDGE ( 'NONE', *, *, #28776, .F. ) ;
#12683 = CARTESIAN_POINT ( 'NONE',  ( -10.31595651221557830, -17.04027680973078063, 57.79486398785477519 ) ) ;
#12684 = CARTESIAN_POINT ( 'NONE',  ( 10.57590614458695377, 2.144455078683989768, 49.30629848276630156 ) ) ;
#12685 = CARTESIAN_POINT ( 'NONE',  ( -23.73684003905821527, -18.76684476618103403, 72.95023626440647035 ) ) ;
#12686 = FACE_BOUND ( 'NONE', #32713, .T. ) ;
#12687 = TOROIDAL_SURFACE ( 'NONE', #40222, 1.499999999999998224, 0.5000000000000000000 ) ;
#12688 = LINE ( 'NONE', #38541, #30575 ) ;
#12689 = CARTESIAN_POINT ( 'NONE',  ( -24.39763799706551950, -15.84669482609578317, 69.54779622430706354 ) ) ;
#12690 = AXIS2_PLACEMENT_3D ( 'NONE', #30398, #14352, #4289 ) ;
#12691 = DIRECTION ( 'NONE',  ( 0.02400335114476204179, -0.9997118780597843424, -1.529429985666831130E-10 ) ) ;
#12692 = ORIENTED_EDGE ( 'NONE', *, *, #34781, .F. ) ;
#12693 = CARTESIAN_POINT ( 'NONE',  ( -10.67763251680271175, -12.94209746246583492, 64.34124149314979491 ) ) ;
#12694 = ORIENTED_EDGE ( 'NONE', *, *, #34274, .T. ) ;
#12695 = B_SPLINE_CURVE_WITH_KNOTS ( 'NONE', 3,
 ( #5060, #38531, #35800, #16841, #42241, #46423, #27936, #31644, #35072, #20069 ),
 .UNSPECIFIED., .F., .F.,
 ( 4, 2, 2, 2, 4 ),
 ( 0.6272669072877483654, 0.7522669073072711932, 0.8772669073267939099, 1.002266907346316627, 1.127266907365839455 ),
 .UNSPECIFIED. ) ;
#12696 = CARTESIAN_POINT ( 'NONE',  ( -11.14372862008015019, -11.71776470779160917, 67.80967772160084905 ) ) ;
#12697 = CARTESIAN_POINT ( 'NONE',  ( -22.88419851978063591, -10.42888047092867865, 63.07185995612697837 ) ) ;
#12698 = VERTEX_POINT ( 'NONE', #47783 ) ;
#12699 = AXIS2_PLACEMENT_3D ( 'NONE', #29685, #19328, #3837 ) ;
#12700 = CARTESIAN_POINT ( 'NONE',  ( -15.28291166272247992, -21.52618791248891128, 68.87592918174580348 ) ) ;
#12701 = EDGE_CURVE ( 'NONE', #26903, #48665, #40626, .T. ) ;
#12702 = FACE_BOUND ( 'NONE', #37905, .T. ) ;
#12703 = VERTEX_POINT ( 'NONE', #29072 ) ;
#12704 = ORIENTED_EDGE ( 'NONE', *, *, #11049, .F. ) ;
#12705 = VERTEX_POINT ( 'NONE', #43623 ) ;
#12706 = CARTESIAN_POINT ( 'NONE',  ( -17.91610874870965020, -22.24302035646641684, 62.13181838639658139 ) ) ;
#12707 = CIRCLE ( 'NONE', #25296, 0.4000000000000006883 ) ;
#12708 = CARTESIAN_POINT ( 'NONE',  ( -23.16117746674104438, -18.90708040007733359, 62.63934749780565880 ) ) ;
#12709 = EDGE_CURVE ( 'NONE', #35477, #32441, #27696, .T. ) ;
#12710 = DIRECTION ( 'NONE',  ( -2.866981220435666553E-17, 1.000000000000000000, 1.190614954331866791E-16 ) ) ;
#12711 = CARTESIAN_POINT ( 'NONE',  ( -17.42409385541300182, -14.80920654474440745, 53.27966884056655061 ) ) ;
#12712 = CARTESIAN_POINT ( 'NONE',  ( -10.75331705403316818, -16.93070056221711184, 57.98760548944069626 ) ) ;
#12713 = ORIENTED_EDGE ( 'NONE', *, *, #8010, .F. ) ;
#12714 = ORIENTED_EDGE ( 'NONE', *, *, #47249, .T. ) ;
#12715 = CARTESIAN_POINT ( 'NONE',  ( -21.93659385650551741, -6.915538690918074494, 49.31353937987644542 ) ) ;
#12716 = VECTOR ( 'NONE', #29638, 1000.000000000000000 ) ;
#12717 = CARTESIAN_POINT ( 'NONE',  ( -43.17409385541305511, -15.80920654474410725, 56.99999999999999289 ) ) ;
#12718 = CARTESIAN_POINT ( 'NONE',  ( -13.27161037900033058, -18.02158587759403829, 49.52966884056656482 ) ) ;
#12719 = DIRECTION ( 'NONE',  ( -2.209513405570979834E-06, 7.769005115158032304E-07, 0.9999999999972571940 ) ) ;
#12720 = CARTESIAN_POINT ( 'NONE',  ( -22.61159385650551457, -6.922745924619793101, 51.69366785382590024 ) ) ;
#12721 = EDGE_CURVE ( 'NONE', #16722, #30190, #25340, .T. ) ;
#12722 = VERTEX_POINT ( 'NONE', #14021 ) ;
#12723 = AXIS2_PLACEMENT_3D ( 'NONE', #14614, #14375, #22289 ) ;
#12724 = DIRECTION ( 'NONE',  ( 1.015202570477164967E-16, 0.3090169943749398462, -0.9510565162951560847 ) ) ;
#12725 = CARTESIAN_POINT ( 'NONE',  ( -16.55627334167764175, -21.80933031065637806, 68.99560815001524361 ) ) ;
#12726 = AXIS2_PLACEMENT_3D ( 'NONE', #22035, #41472, #129 ) ;
#12727 = PLANE ( 'NONE',  #22087 ) ;
#12728 = ORIENTED_EDGE ( 'NONE', *, *, #26187, .F. ) ;
#12729 = B_SPLINE_CURVE_WITH_KNOTS ( 'NONE', 3,
 ( #10616, #32539, #28610, #17740, #17508, #7180, #36937, #14277, #44135, #6918 ),
 .UNSPECIFIED., .F., .F.,
 ( 4, 2, 2, 2, 4 ),
 ( 0.1272669073658429240, 0.2522669073463211231, 0.3772669073267993500, 0.5022669073072775214, 0.6272669072877556928 ),
 .UNSPECIFIED. ) ;
#12730 = FACE_OUTER_BOUND ( 'NONE', #29878, .T. ) ;
#12731 = ADVANCED_FACE ( 'NONE', ( #6906 ), #2720, .T. ) ;
#12732 = CARTESIAN_POINT ( 'NONE',  ( -10.65715545825994681, -16.81507633650918976, 61.30175972107676330 ) ) ;
#12733 = CARTESIAN_POINT ( 'NONE',  ( -10.42608517478068109, -14.63970064516040637, 68.08473508565809595 ) ) ;
#12734 = DIRECTION ( 'NONE',  ( 0.9687793358424821033, -0.2479245821708677133, 0.000000000000000000 ) ) ;
#12735 = EDGE_CURVE ( 'NONE', #10228, #5216, #17810, .T. ) ;
#12736 = ORIENTED_EDGE ( 'NONE', *, *, #8966, .F. ) ;
#12737 = CARTESIAN_POINT ( 'NONE',  ( -12.23220206747518013, -19.57856285391799034, 58.22682373937800548 ) ) ;
#12738 = CARTESIAN_POINT ( 'NONE',  ( -19.22781571947377444, -4.195962512586791426, 54.61912878955446615 ) ) ;
#12739 = CYLINDRICAL_SURFACE ( 'NONE', #44171, 1.999999999999999112 ) ;
#12740 = VERTEX_POINT ( 'NONE', #28597 ) ;
#12741 = LINE ( 'NONE', #1164, #815 ) ;
#12742 = VERTEX_POINT ( 'NONE', #29315 ) ;
#12743 = FACE_OUTER_BOUND ( 'NONE', #16714, .T. ) ;
#12744 = LINE ( 'NONE', #17137, #35080 ) ;
#12745 = ORIENTED_EDGE ( 'NONE', *, *, #48606, .T. ) ;
#12746 = DIRECTION ( 'NONE',  ( -3.071710424422018668E-17, 6.404604876783312462E-16, 1.000000000000000000 ) ) ;
#12747 = CARTESIAN_POINT ( 'NONE',  ( -20.19838274129777389, -21.29432534982823810, 72.61298750797109847 ) ) ;
#12748 = CARTESIAN_POINT ( 'NONE',  ( -14.22441497990486958, -8.081217732231424478, 67.44470516081543110 ) ) ;
#12749 = DIRECTION ( 'NONE',  ( -5.104528445087193737E-07, -5.317498825627977299E-07, -0.9999999999997284394 ) ) ;
#12750 = ORIENTED_EDGE ( 'NONE', *, *, #4935, .F. ) ;
#12751 = CARTESIAN_POINT ( 'NONE',  ( -23.83080496556880945, -17.75212211224490133, 59.28906343887996400 ) ) ;
#12752 = CARTESIAN_POINT ( 'NONE',  ( -20.66207812730969096, -8.601311705287542964, 63.50048569590220637 ) ) ;
#12753 =( BOUNDED_CURVE ( )  B_SPLINE_CURVE ( 3, ( #22621, #36882, #232, #30020 ),
 .UNSPECIFIED., .F., .F. ) 
 B_SPLINE_CURVE_WITH_KNOTS ( ( 4, 4 ),
 ( 0.4074455897393681747, 0.5000000000000000000 ),
 .UNSPECIFIED. ) 
 CURVE ( )  GEOMETRIC_REPRESENTATION_ITEM ( )  RATIONAL_B_SPLINE_CURVE ( ( 0.6983129098261053880, 0.7760317562607254027, 0.8765941196520283807, 1.000000000000026201 ) ) 
 REPRESENTATION_ITEM ( '' )  );
#12755 = EDGE_CURVE ( 'NONE', #13527, #32027, #43087, .T. ) ;
#12754 = CARTESIAN_POINT ( 'NONE',  ( -23.85820194903862657, -17.69173191509663567, 62.48833042115954584 ) ) ;
#12756 = VERTEX_POINT ( 'NONE', #10374 ) ;
#12757 = FACE_OUTER_BOUND ( 'NONE', #10556, .T. ) ;
#12758 = ADVANCED_FACE ( 'NONE', ( #44351 ), #29872, .T. ) ;
#12759 = CARTESIAN_POINT ( 'NONE',  ( -24.72421832269116138, -16.29687976975823460, 62.75475226558750563 ) ) ;
#12760 = EDGE_CURVE ( 'NONE', #40280, #40811, #39837, .T. ) ;
#12761 = EDGE_CURVE ( 'NONE', #34423, #6071, #26476, .T. ) ;
#12762 = ORIENTED_EDGE ( 'NONE', *, *, #19653, .F. ) ;
#12763 = ORIENTED_EDGE ( 'NONE', *, *, #35430, .T. ) ;
#12764 = CARTESIAN_POINT ( 'NONE',  ( -23.65513889391139557, -11.50482878637529716, 62.83729622335476961 ) ) ;
#12765 = CARTESIAN_POINT ( 'NONE',  ( -20.00855069579964862, -21.31476573450181888, 72.70478738568573362 ) ) ;
#12766 = DIRECTION ( 'NONE',  ( -3.071710424422018668E-17, 6.404604876783312462E-16, 1.000000000000000000 ) ) ;
#12767 = CARTESIAN_POINT ( 'NONE',  ( -16.61784385650551954, -9.790100578890868377, 49.79778022625163203 ) ) ;
#12768 = CARTESIAN_POINT ( 'NONE',  ( -12.39491807234433551, -9.940094850350357447, 57.37470223362350907 ) ) ;
#12769 = LINE ( 'NONE', #20154, #29070 ) ;
#12770 = CARTESIAN_POINT ( 'NONE',  ( -24.27033198218900978, -13.12649362337911718, 62.83264177274070050 ) ) ;
#12771 =( BOUNDED_CURVE ( )  B_SPLINE_CURVE ( 3, ( #32351, #6716, #39723, #17546 ),
 .UNSPECIFIED., .F., .F. ) 
 B_SPLINE_CURVE_WITH_KNOTS ( ( 4, 4 ),
 ( 0.9074455897393625126, 1.000000000000000000 ),
 .UNSPECIFIED. ) 
 CURVE ( )  GEOMETRIC_REPRESENTATION_ITEM ( )  RATIONAL_B_SPLINE_CURVE ( ( 0.6983129098260738576, 0.7760317562606816599, 0.8765941196519904111, 1.000000000000000000 ) ) 
 REPRESENTATION_ITEM ( '' )  );
#12772 = CARTESIAN_POINT ( 'NONE',  ( -13.88634980723361778, -21.36569984987395188, 72.03269384293926691 ) ) ;
#12773 = ORIENTED_EDGE ( 'NONE', *, *, #25234, .T. ) ;
#12774 = ORIENTED_EDGE ( 'NONE', *, *, #28829, .F. ) ;
#12775 = CARTESIAN_POINT ( 'NONE',  ( -10.96024275427387984, -11.10349598290784989, 60.79230391164892211 ) ) ;
#12776 = CARTESIAN_POINT ( 'NONE',  ( -22.86159385541300182, -7.228003583438063373, 51.38655588711991840 ) ) ;
#12777 = DIRECTION ( 'NONE',  ( 0.3636930986378153485, 0.9315188296557532777, -1.850371886801397451E-09 ) ) ;
#12778 = CARTESIAN_POINT ( 'NONE',  ( -17.42409385541299471, -14.80920654474435594, 52.02966884056656482 ) ) ;
#12779 = ORIENTED_EDGE ( 'NONE', *, *, #2394, .F. ) ;
#12780 = ADVANCED_FACE ( 'NONE', ( #7408 ), #7658, .F. ) ;
#12781 = DIRECTION ( 'NONE',  ( 2.181982678098338148E-16, 0.000000000000000000, -1.000000000000000000 ) ) ;
#12782 = CARTESIAN_POINT ( 'NONE',  ( -14.91623309787384066, -21.82459129695467581, 65.26743172979871588 ) ) ;
#12783 = CARTESIAN_POINT ( 'NONE',  ( -19.89283007060495123, -10.81159512726059191, 49.52966884056655772 ) ) ;
#12784 = VERTEX_POINT ( 'NONE', #48504 ) ;
#12785 = CARTESIAN_POINT ( 'NONE',  ( -24.81734138798520561, -15.73308575106217511, 69.64652101300646336 ) ) ;
#12786 = ORIENTED_EDGE ( 'NONE', *, *, #7105, .F. ) ;
#12787 = CARTESIAN_POINT ( 'NONE',  ( -22.63063519912030941, -20.13802011715040052, 69.35230721051679836 ) ) ;
#12788 = PLANE ( 'NONE',  #9239 ) ;
#12789 = ORIENTED_EDGE ( 'NONE', *, *, #45645, .F. ) ;
#12790 = CARTESIAN_POINT ( 'NONE',  ( -13.60167271156757707, -11.21037387301822186, 50.77966884056655772 ) ) ;
#12791 = ORIENTED_EDGE ( 'NONE', *, *, #13134, .F. ) ;
#12792 = DIRECTION ( 'NONE',  ( -0.9893874368562762811, 0.1453014101478983522, -3.604276813338691349E-17 ) ) ;
#12793 = CARTESIAN_POINT ( 'NONE',  ( -18.60463909989377385, -22.16515503909319307, 72.32864992405023941 ) ) ;
#12794 = ORIENTED_EDGE ( 'NONE', *, *, #35644, .T. ) ;
#12795 = CARTESIAN_POINT ( 'NONE',  ( -15.18638434861223452, -8.119849305256630956, 57.14999999999947278 ) ) ;
#12796 = CARTESIAN_POINT ( 'NONE',  ( -16.11159385541290590, -8.990409506049370947, 49.61344411288057898 ) ) ;
#12797 = CARTESIAN_POINT ( 'NONE',  ( -18.11159385650551457, -6.922745924619793101, 51.69366785382590024 ) ) ;
#12798 = EDGE_LOOP ( 'NONE', ( #42476, #38044, #20992, #10821, #16314, #48407, #43343 ) ) ;
#12799 = CARTESIAN_POINT ( 'NONE',  ( -17.82745577869553699, -7.820727362736762167, 60.38060779106270104 ) ) ;
#12800 = CARTESIAN_POINT ( 'NONE',  ( -19.24035349434955577, -7.583912967164861740, 63.68735177183580021 ) ) ;
#12801 = CARTESIAN_POINT ( 'NONE',  ( -16.45566506110110083, -21.79267588865899086, 62.04095995016087528 ) ) ;
#12802 = ORIENTED_EDGE ( 'NONE', *, *, #37342, .T. ) ;
#12803 = CARTESIAN_POINT ( 'NONE',  ( -24.10584571748465521, -12.56049761727124370, 73.39225570139795707 ) ) ;
#12804 = DIRECTION ( 'NONE',  ( 0.000000000000000000, 1.000000000000000000, -0.000000000000000000 ) ) ;
#12805 = CARTESIAN_POINT ( 'NONE',  ( -23.46260370332431933, -11.17067683354235719, 73.66193301755811262 ) ) ;
#12806 = FACE_BOUND ( 'NONE', #31205, .T. ) ;
#12807 = CARTESIAN_POINT ( 'NONE',  ( -12.26730668522635526, -19.62818085036556681, 65.01107574152555912 ) ) ;
#12808 = ADVANCED_FACE ( 'NONE', ( #11573 ), #23260, .T. ) ;
#12809 = EDGE_CURVE ( 'NONE', #40331, #3004, #9457, .T. ) ;
#12810 = VECTOR ( 'NONE', #26971, 1000.000000000000000 ) ;
#12811 = VERTEX_POINT ( 'NONE', #4428 ) ;
#12812 = ORIENTED_EDGE ( 'NONE', *, *, #3325, .T. ) ;
#12813 = DIRECTION ( 'NONE',  ( 0.000000000000000000, -0.000000000000000000, 1.000000000000000000 ) ) ;
#12814 = CARTESIAN_POINT ( 'NONE',  ( -21.46381135070672386, -20.59674881067212127, 69.21017043924877044 ) ) ;
#12815 = ORIENTED_EDGE ( 'NONE', *, *, #41804, .T. ) ;
#12816 = CARTESIAN_POINT ( 'NONE',  ( -24.34865124180699070, -15.83455620839685452, 66.13612870751769890 ) ) ;
#12817 = DIRECTION ( 'NONE',  ( 0.6478992145799702396, -0.7617260713318518839, 1.927832152310587483E-08 ) ) ;
#12818 = CARTESIAN_POINT ( 'NONE',  ( -18.22409385759798894, -9.359200813967568422, 50.49621490985803263 ) ) ;
#12819 = DIRECTION ( 'NONE',  ( -2.866981220435666553E-17, 1.000000000000000000, 1.190614954331866791E-16 ) ) ;
#12820 = CARTESIAN_POINT ( 'NONE',  ( -11.12219343327886811, -17.98741664779230121, 71.72285496256920112 ) ) ;
#12821 = CARTESIAN_POINT ( 'NONE',  ( -10.95917937052863422, -17.62195967018737619, 71.58190244267143498 ) ) ;
#12822 = ORIENTED_EDGE ( 'NONE', *, *, #37535, .T. ) ;
#12823 = ADVANCED_FACE ( 'NONE', ( #41619 ), #19447, .T. ) ;
#12824 = EDGE_CURVE ( 'NONE', #28108, #22354, #11829, .T. ) ;
#12825 = B_SPLINE_CURVE_WITH_KNOTS ( 'NONE', 3,
 ( #25151, #47791, #18223, #28835, #10847, #36215, #25870, #32992, #6913, #10610 ),
 .UNSPECIFIED., .F., .F.,
 ( 4, 2, 2, 2, 4 ),
 ( 0.000000000000000000, 0.2500000000000000000, 0.5000000000000000000, 0.7500000000000000000, 1.000000000000000000 ),
 .UNSPECIFIED. ) ;
#12826 = CARTESIAN_POINT ( 'NONE',  ( -22.58588533274201282, -20.18224782263116523, 69.36073240021890740 ) ) ;
#12827 = CARTESIAN_POINT ( 'NONE',  ( -19.17437844398820346, -7.979623566120205957, 63.44561363416070776 ) ) ;
#12828 = CARTESIAN_POINT ( 'NONE',  ( -23.21283114448125673, -10.11939864774917908, 63.25681283445349123 ) ) ;
#12829 = CARTESIAN_POINT ( 'NONE',  ( -12.58002129225892674, -9.148929240056048684, 74.43427715830415536 ) ) ;
#12830 = CARTESIAN_POINT ( 'NONE',  ( -21.46447785953442278, -9.092825438250168091, 70.13132491419585790 ) ) ;
#12831 = EDGE_LOOP ( 'NONE', ( #3775, #10472, #39736, #35678 ) ) ;
#12832 = VERTEX_POINT ( 'NONE', #15000 ) ;
#12833 = ORIENTED_EDGE ( 'NONE', *, *, #31880, .T. ) ;
#12834 = EDGE_CURVE ( 'NONE', #24853, #18111, #34883, .T. ) ;
#12835 = DIRECTION ( 'NONE',  ( -0.000000000000000000, -1.000000000000000000, -0.000000000000000000 ) ) ;
#12836 = CARTESIAN_POINT ( 'NONE',  ( -20.03075563493810307, -21.35977203713853712, 72.69918973885827995 ) ) ;
#12837 = ORIENTED_EDGE ( 'NONE', *, *, #270, .T. ) ;
#12838 = CARTESIAN_POINT ( 'NONE',  ( -10.43656091707388534, -14.37069178587375973, 67.92970350560246118 ) ) ;
#12839 = CARTESIAN_POINT ( 'NONE',  ( -22.68978555823764864, -10.11602685316156780, 73.57341092052691067 ) ) ;
#12840 = AXIS2_PLACEMENT_3D ( 'NONE', #21936, #18228, #25158 ) ;
#12841 = ORIENTED_EDGE ( 'NONE', *, *, #824, .T. ) ;
#12842 = CARTESIAN_POINT ( 'NONE',  ( -14.65765131015531253, -21.78034674156931061, 54.27966884056655061 ) ) ;
#12843 = CARTESIAN_POINT ( 'NONE',  ( -19.43748438392636402, -21.56872497219108098, 58.41018533341049590 ) ) ;
#12844 = EDGE_LOOP ( 'NONE', ( #39490, #5323, #4930, #47671, #30927 ) ) ;
#12845 = DIRECTION ( 'NONE',  ( -2.112005902016726815E-14, 0.000000000000000000, -1.000000000000000000 ) ) ;
#12846 = EDGE_LOOP ( 'NONE', ( #23529, #16590, #1528, #26762, #40975 ) ) ;
#12847 = CARTESIAN_POINT ( 'NONE',  ( -23.56138404952065812, -11.33988834032952830, 70.19210750372964469 ) ) ;
#12848 = ORIENTED_EDGE ( 'NONE', *, *, #8190, .T. ) ;
#12849 = CARTESIAN_POINT ( 'NONE',  ( -15.77151528785019430, -19.20744933288474954, 52.02966884056656482 ) ) ;
#12850 = CARTESIAN_POINT ( 'NONE',  ( -46.47622156840087371, -14.20920654474410760, 70.13000000000000966 ) ) ;
#12851 = CARTESIAN_POINT ( 'NONE',  ( -18.91460061187875397, -21.70800071742875303, 58.66940498489888256 ) ) ;
#12852 = ORIENTED_EDGE ( 'NONE', *, *, #7906, .F. ) ;
#12853 = CARTESIAN_POINT ( 'NONE',  ( -24.40658499505740053, -15.78250870199476807, 69.83307488408829045 ) ) ;
#12854 = DIRECTION ( 'NONE',  ( 0.9687793358424821033, -0.2479245821708680464, 0.000000000000000000 ) ) ;
#12855 = CARTESIAN_POINT ( 'NONE',  ( -30.42409385541305156, -8.109206544744111511, 51.75000000000000711 ) ) ;
#12856 = CARTESIAN_POINT ( 'NONE',  ( -16.20683845212634111, -21.70255763714999020, 58.58585572420326315 ) ) ;
#12857 = CARTESIAN_POINT ( 'NONE',  ( -10.45529269445903253, -15.48619349139875467, 61.14862166396536480 ) ) ;
#12858 = CARTESIAN_POINT ( 'NONE',  ( -10.40174263535760524, -17.29725023780839166, 61.34238537770443855 ) ) ;
#12859 = ORIENTED_EDGE ( 'NONE', *, *, #18273, .F. ) ;
#12860 = DIRECTION ( 'NONE',  ( 0.000000000000000000, 1.000000000000000000, -0.000000000000000000 ) ) ;
#12861 = CARTESIAN_POINT ( 'NONE',  ( -11.97490362423377164, -10.33561459433851404, 67.78424783647008667 ) ) ;
#12862 = CARTESIAN_POINT ( 'NONE',  ( -23.04402284766838349, -19.06632961612601918, 59.16938527523783620 ) ) ;
#12863 = DIRECTION ( 'NONE',  ( 1.000000000000000000, 2.866981220435666553E-17, 0.000000000000000000 ) ) ;
#12864 = CARTESIAN_POINT ( 'NONE',  ( -14.19711780326422712, -21.02108897209633298, 72.15280992966681595 ) ) ;
#12865 = CARTESIAN_POINT ( 'NONE',  ( -15.71784385650551741, -9.790100578890868377, 49.79778022625163203 ) ) ;
#12866 = EDGE_CURVE ( 'NONE', #5991, #47078, #11337, .T. ) ;
#12867 = EDGE_LOOP ( 'NONE', ( #4455, #6325, #13111, #22762, #16008 ) ) ;
#12868 = CARTESIAN_POINT ( 'NONE',  ( -10.43125849979191955, -13.91324152291312366, 57.74825034919034294 ) ) ;
#12869 = DIRECTION ( 'NONE',  ( 0.7224352045700187519, 0.6914386272098739239, -9.340627245513716657E-09 ) ) ;
#12870 = ORIENTED_EDGE ( 'NONE', *, *, #20609, .F. ) ;
#12871 = B_SPLINE_CURVE_WITH_KNOTS ( 'NONE', 3,
 ( #55, #23194, #41166, #15526, #15284, #22456, #4465, #37703, #26155, #15778 ),
 .UNSPECIFIED., .F., .F.,
 ( 4, 2, 2, 2, 4 ),
 ( 0.6272669072877858909, 0.7522669073072849599, 0.8772669073267839179, 1.002266907346282876, 1.127266907365781945 ),
 .UNSPECIFIED. ) ;
#12872 = CARTESIAN_POINT ( 'NONE',  ( -24.42668993457695592, -13.99045928592870780, 73.40799407547365263 ) ) ;
#12873 = CARTESIAN_POINT ( 'NONE',  ( -10.64203103149789698, -13.07586850037579040, 67.75334752786112347 ) ) ;
#12874 = CARTESIAN_POINT ( 'NONE',  ( -23.03380641475053281, -9.905658051014942345, 66.65526928932193584 ) ) ;
#12875 = CARTESIAN_POINT ( 'NONE',  ( -23.21760288594795441, -10.12534664246260441, 63.26460134184395656 ) ) ;
#12876 = CARTESIAN_POINT ( 'NONE',  ( -16.91855014848012928, -22.24212009645463439, 72.28047803099305213 ) ) ;
#12877 = VERTEX_POINT ( 'NONE', #45576 ) ;
#12878 = CARTESIAN_POINT ( 'NONE',  ( -13.92409385541305511, -10.60920654474410618, 80.49999999999998579 ) ) ;
#12879 = EDGE_CURVE ( 'NONE', #2353, #41372, #45378, .T. ) ;
#12880 = CARTESIAN_POINT ( 'NONE',  ( -19.05927265761716072, -8.002745927047119068, 63.43089191541108107 ) ) ;
#12881 = VERTEX_POINT ( 'NONE', #11366 ) ;
#12882 = AXIS2_PLACEMENT_3D ( 'NONE', #41945, #42187, #12378 ) ;
#12883 = CARTESIAN_POINT ( 'NONE',  ( -18.52160066619603995, -22.17809164712859271, 72.44657480731611088 ) ) ;
#12884 = EDGE_CURVE ( 'NONE', #12524, #3450, #39635, .T. ) ;
#12885 = EDGE_CURVE ( 'NONE', #11741, #39260, #39918, .T. ) ;
#12886 = CARTESIAN_POINT ( 'NONE',  ( -23.46018882259003036, -11.26354882964838033, 73.37809979709153652 ) ) ;
#12887 = CARTESIAN_POINT ( 'NONE',  ( -10.37497030826117417, -14.69804335084345581, 71.32782692816427073 ) ) ;
#12888 =( BOUNDED_SURFACE ( )  B_SPLINE_SURFACE ( 3, 1, ( 
 ( #2061, #20051 ),
 ( #43443, #13121 ),
 ( #16335, #31374 ),
 ( #27919, #5530 ),
 ( #24729, #31130 ),
 ( #42468, #24492 ),
 ( #13369, #39731 ) ),
 .UNSPECIFIED., .T., .F., .F. ) 
 B_SPLINE_SURFACE_WITH_KNOTS ( ( 4, 3, 4 ),
 ( 2, 2 ),
 ( 0.000000000000000000, 0.5000000000000000000, 1.000000000000000000 ),
 ( 0.000000000000000000, 1.000000000000000000 ),
 .UNSPECIFIED. ) 
 GEOMETRIC_REPRESENTATION_ITEM ( )  RATIONAL_B_SPLINE_SURFACE ( (
 ( 1.000000000000000000, 1.000000000000000000),
 ( 0.3333333333333335369, 0.3333333333333330373),
 ( 0.3333333333333335369, 0.3333333333333330373),
 ( 1.000000000000000000, 1.000000000000000000),
 ( 0.3333333333333333703, 0.3333333333333333703),
 ( 0.3333333333333333703, 0.3333333333333333703),
 ( 1.000000000000000000, 1.000000000000000000) ) ) 
 REPRESENTATION_ITEM ( '' )  SURFACE ( )  );
#12889 = CARTESIAN_POINT ( 'NONE',  ( -46.29409385541305255, -13.72754205882879042, 70.03986341317408915 ) ) ;
#12890 = EDGE_LOOP ( 'NONE', ( #27698, #35629, #38709, #47515, #10383 ) ) ;
#12891 = ORIENTED_EDGE ( 'NONE', *, *, #42838, .T. ) ;
#12892 = CARTESIAN_POINT ( 'NONE',  ( -23.14284385541304800, -7.587656875400192291, 49.25157356644813689 ) ) ;
#12893 = CYLINDRICAL_SURFACE ( 'NONE', #6768, 2.000000000000001776 ) ;
#12894 = CARTESIAN_POINT ( 'NONE',  ( -19.23866564181064831, -21.62168251543363695, 58.82507384655653482 ) ) ;
#12895 = FACE_OUTER_BOUND ( 'NONE', #43660, .T. ) ;
#12896 =( BOUNDED_CURVE ( )  B_SPLINE_CURVE ( 3, ( #19848, #34848, #27946, #8773 ),
 .UNSPECIFIED., .F., .F. ) 
 B_SPLINE_CURVE_WITH_KNOTS ( ( 4, 4 ),
 ( 0.000000000000000000, 0.4074455897393631787 ),
 .UNSPECIFIED. ) 
 CURVE ( )  GEOMETRIC_REPRESENTATION_ITEM ( )  RATIONAL_B_SPLINE_CURVE ( ( 1.000000000000000000, 0.4567392136813412939, 0.3561768502900337641, 0.6983129098260774104 ) ) 
 REPRESENTATION_ITEM ( '' )  );
#12897 = DIRECTION ( 'NONE',  ( -3.413470714839332458E-33, 1.190614954331866791E-16, -1.000000000000000000 ) ) ;
#12898 = CARTESIAN_POINT ( 'NONE',  ( -13.97495002277310583, -20.90053183151249172, 68.47127524766125362 ) ) ;
#12899 = CARTESIAN_POINT ( 'NONE',  ( -10.44916082259176093, -15.83527127794237543, 64.80771589743309846 ) ) ;
#12900 = CARTESIAN_POINT ( 'NONE',  ( -46.29409385541305966, -14.20920654474410760, 71.05212771298751306 ) ) ;
#12901 = VERTEX_POINT ( 'NONE', #529 ) ;
#12902 = CARTESIAN_POINT ( 'NONE',  ( -21.73662441638722953, -9.231682010981758779, 66.67622112302015580 ) ) ;
#12903 = CARTESIAN_POINT ( 'NONE',  ( -21.18000576974785787, -20.77541348745421246, 69.35450184739246993 ) ) ;
#12904 =( BOUNDED_CURVE ( )  B_SPLINE_CURVE ( 2, ( #849, #46874, #20540, #27913, #31124, #30896, #46396, #35541, #31854 ),
 .UNSPECIFIED., .F., .F. ) 
 B_SPLINE_CURVE_WITH_KNOTS ( ( 3, 2, 2, 2, 3 ),
 ( 0.5416666666666667407, 0.5520833333333334814, 0.5625000000000000000, 0.5729166666666665186, 0.5833333333333332593 ),
 .UNSPECIFIED. ) 
 CURVE ( )  GEOMETRIC_REPRESENTATION_ITEM ( )  RATIONAL_B_SPLINE_CURVE ( ( 0.9999999999999992228, 0.9238795325112875156, 1.000000000000000000, 0.9238795325112867385, 1.000000000000000000, 0.9238795325112867385, 1.000000000000000000, 0.9238795325112875156, 0.9999999999999992228 ) ) 
 REPRESENTATION_ITEM ( '' )  );
#12905 = VECTOR ( 'NONE', #42644, 1000.000000000000000 ) ;
#12906 = ORIENTED_EDGE ( 'NONE', *, *, #12595, .F. ) ;
#12907 = CARTESIAN_POINT ( 'NONE',  ( -10.31364544024427410, -17.03300993871772562, 57.80265247535063367 ) ) ;
#12908 = CARTESIAN_POINT ( 'NONE',  ( -10.02613496734058351, -15.68824233352117403, 61.18789043449853438 ) ) ;
#12909 = VERTEX_POINT ( 'NONE', #7938 ) ;
#12910 = CARTESIAN_POINT ( 'NONE',  ( -10.43972881942000086, -15.77115500203794873, 64.52243715390834211 ) ) ;
#12911 = AXIS2_PLACEMENT_3D ( 'NONE', #12803, #32264, #43350 ) ;
#12912 = DIRECTION ( 'NONE',  ( -2.846534185458051278E-06, -1.189262794577403004E-05, -0.9999999999252313643 ) ) ;
#12913 = EDGE_CURVE ( 'NONE', #25709, #18406, #4232, .T. ) ;
#12914 = CARTESIAN_POINT ( 'NONE',  ( -12.50766613833180330, -19.86205114983803455, 64.86674886870797252 ) ) ;
#12915 = CARTESIAN_POINT ( 'NONE',  ( -22.50979607835742158, -19.61933652539927309, 72.94400553403978904 ) ) ;
#12916 = ORIENTED_EDGE ( 'NONE', *, *, #35977, .T. ) ;
#12917 = CARTESIAN_POINT ( 'NONE',  ( -18.67529344402863956, -22.15414776727839907, 72.39855560065855400 ) ) ;
#12918 = DIRECTION ( 'NONE',  ( -2.191687988502693051E-06, 1.258878959409210278E-05, 0.9999999999183594168 ) ) ;
#12919 = CARTESIAN_POINT ( 'NONE',  ( -24.10556926794565413, -12.55028678686139898, 69.65754220287278997 ) ) ;
#12920 = DIRECTION ( 'NONE',  ( 3.071710424422018668E-17, -6.404604876783312462E-16, -1.000000000000000000 ) ) ;
#12921 = B_SPLINE_CURVE_WITH_KNOTS ( 'NONE', 1,
 ( #48360, #26701 ),
 .UNSPECIFIED., .F., .F.,
 ( 2, 2 ),
 ( 0.000000000000000000, 1.000000000000000000 ),
 .UNSPECIFIED. ) ;
#12922 = FACE_OUTER_BOUND ( 'NONE', #23464, .T. ) ;
#12923 = ORIENTED_EDGE ( 'NONE', *, *, #4163, .F. ) ;
#12924 = DIRECTION ( 'NONE',  ( -0.3478314405900307937, -0.9375570856950865561, 0.000000000000000000 ) ) ;
#12925 = DIRECTION ( 'NONE',  ( -1.000000000000000000, 0.000000000000000000, 9.637352644315596475E-17 ) ) ;
#12926 = CARTESIAN_POINT ( 'NONE',  ( -14.92764441971231726, -21.34891144748960201, 61.93600440564248544 ) ) ;
#12927 = VERTEX_POINT ( 'NONE', #8404 ) ;
#12928 = DIRECTION ( 'NONE',  ( 0.5820088206811424580, -0.8131824719270214219, 7.019974882119937445E-08 ) ) ;
#12929 = FACE_BOUND ( 'NONE', #33914, .T. ) ;
#12930 = ORIENTED_EDGE ( 'NONE', *, *, #3544, .F. ) ;
#12931 = ORIENTED_EDGE ( 'NONE', *, *, #48449, .T. ) ;
#12932 = ORIENTED_EDGE ( 'NONE', *, *, #3580, .F. ) ;
#12933 = EDGE_CURVE ( 'NONE', #29013, #14217, #29846, .T. ) ;
#12934 = EDGE_CURVE ( 'NONE', #12832, #33156, #44982, .T. ) ;
#12935 = CARTESIAN_POINT ( 'NONE',  ( -14.90981281861414587, -21.39562369906352757, 61.78600440604535748 ) ) ;
#12936 = CARTESIAN_POINT ( 'NONE',  ( -10.39693166811831304, -15.37990016280386740, 57.58264896457095006 ) ) ;
#12937 = CARTESIAN_POINT ( 'NONE',  ( -48.42409385541304800, -27.10920654474410796, 45.99999999999998579 ) ) ;
#12938 = DIRECTION ( 'NONE',  ( 0.000000000000000000, 0.000000000000000000, -1.000000000000000000 ) ) ;
#12939 = ORIENTED_EDGE ( 'NONE', *, *, #5380, .F. ) ;
#12940 = ORIENTED_EDGE ( 'NONE', *, *, #42220, .F. ) ;
#12941 = VECTOR ( 'NONE', #5088, 1000.000000000000000 ) ;
#12942 = EDGE_CURVE ( 'NONE', #17100, #18739, #19476, .T. ) ;
#12943 = CARTESIAN_POINT ( 'NONE',  ( -21.43034385650551954, -9.794322478646142471, 51.19202720610083901 ) ) ;
#12944 = VECTOR ( 'NONE', #20847, 1000.000000000000000 ) ;
#12945 = LINE ( 'NONE', #39050, #14182 ) ;
#12946 = CYLINDRICAL_SURFACE ( 'NONE', #44903, 0.1500000000000007716 ) ;
#12947 = EDGE_CURVE ( 'NONE', #14347, #9986, #43630, .T. ) ;
#12948 = CARTESIAN_POINT ( 'NONE',  ( -21.76784385650551101, -6.428312510596451368, 51.20221977374900035 ) ) ;
#12949 = ORIENTED_EDGE ( 'NONE', *, *, #2452, .T. ) ;
#12950 = CARTESIAN_POINT ( 'NONE',  ( -10.08052675126636721, -16.06451543208143917, 68.09272439531302723 ) ) ;
#12951 = CARTESIAN_POINT ( 'NONE',  ( -10.91015311220344053, -11.19381230364907864, 64.29882037057124933 ) ) ;
#12952 = CARTESIAN_POINT ( 'NONE',  ( -17.35619151017142769, -7.809413324447545435, 67.02039598641979978 ) ) ;
#12953 = ORIENTED_EDGE ( 'NONE', *, *, #30078, .F. ) ;
#12954 = LINE ( 'NONE', #39315, #16348 ) ;
#12955 = B_SPLINE_CURVE_WITH_KNOTS ( 'NONE', 1,
 ( #29725, #27002 ),
 .UNSPECIFIED., .F., .F.,
 ( 2, 2 ),
 ( 0.000000000000000000, 1.000000000000000000 ),
 .UNSPECIFIED. ) ;
#12956 = CARTESIAN_POINT ( 'NONE',  ( -10.42477179210370686, -17.36325313327283482, 61.27087820301521504 ) ) ;
#12957 = CARTESIAN_POINT ( 'NONE',  ( -10.98142154448249208, -12.07205956039035399, 74.66726427164191193 ) ) ;
#12958 = CARTESIAN_POINT ( 'NONE',  ( -22.28468842640968006, -19.91619389767071269, 65.98949666203347419 ) ) ;
#12959 = VERTEX_POINT ( 'NONE', #41399 ) ;
#12960 = CARTESIAN_POINT ( 'NONE',  ( -24.43362369560107794, -14.05489154181400124, 73.27271507725298250 ) ) ;
#12961 = EDGE_CURVE ( 'NONE', #48574, #28733, #11487, .T. ) ;
#12962 = CARTESIAN_POINT ( 'NONE',  ( -23.75972628784533569, -10.79550978475969991, 54.27966884056655061 ) ) ;
#12963 = CARTESIAN_POINT ( 'NONE',  ( -12.41100344835299474, -20.32040484475852082, 68.51374354841996706 ) ) ;
#12964 = ORIENTED_EDGE ( 'NONE', *, *, #40745, .F. ) ;
#12965 = CARTESIAN_POINT ( 'NONE',  ( -10.40245588357037043, -14.17414831712846990, 61.20349182037644198 ) ) ;
#12966 = ORIENTED_EDGE ( 'NONE', *, *, #19502, .F. ) ;
#12967 = AXIS2_PLACEMENT_3D ( 'NONE', #18379, #14920, #18135 ) ;
#12968 = CARTESIAN_POINT ( 'NONE',  ( -19.17247849636888901, -7.567181371456696226, 63.61584626116109575 ) ) ;
#12969 = CARTESIAN_POINT ( 'NONE',  ( -20.19231683483797113, -8.325423577284544407, 70.55100341277886855 ) ) ;
#12970 = ORIENTED_EDGE ( 'NONE', *, *, #45087, .T. ) ;
#12971 = DIRECTION ( 'NONE',  ( 1.424565731581784133E-06, -1.060674514654238452E-05, 0.9999999999427338082 ) ) ;
#12972 = LINE ( 'NONE', #28501, #23196 ) ;
#12973 = CIRCLE ( 'NONE', #46811, 4.686499999999998778 ) ;
#12974 = CARTESIAN_POINT ( 'NONE',  ( -18.98976565384166193, -12.86018837663894843, 53.27966884056655061 ) ) ;
#12975 = FACE_OUTER_BOUND ( 'NONE', #13840, .T. ) ;
#12976 = ORIENTED_EDGE ( 'NONE', *, *, #24687, .F. ) ;
#12977 = CARTESIAN_POINT ( 'NONE',  ( -10.63483670088760924, -17.87674068094334245, 71.75213521449022380 ) ) ;
#12978 = PRODUCT_DEFINITION_CONTEXT ( 'detailed design', #46687, 'design' ) ;
#12979 = CARTESIAN_POINT ( 'NONE',  ( -13.71293426195967413, -21.26916566922604801, 68.64120525947689089 ) ) ;
#12980 = CARTESIAN_POINT ( 'NONE',  ( -23.42083229484411788, -19.23001078651488172, 62.47690011599960513 ) ) ;
#12981 = VERTEX_POINT ( 'NONE', #18745 ) ;
#12982 = ADVANCED_FACE ( 'NONE', ( #23428 ), #44689, .T. ) ;
#12983 = DIRECTION ( 'NONE',  ( 0.9687793358424821033, -0.2479245821708680464, 0.000000000000000000 ) ) ;
#12984 = CARTESIAN_POINT ( 'NONE',  ( -11.53435529947139315, -18.68938829637487942, 61.16221976381599745 ) ) ;
#12985 = ORIENTED_EDGE ( 'NONE', *, *, #3066, .F. ) ;
#12986 = VERTEX_POINT ( 'NONE', #5693 ) ;
#12987 = CARTESIAN_POINT ( 'NONE',  ( -20.10876870628512592, -21.27392007786688666, 72.51364836102385425 ) ) ;
#12988 = EDGE_CURVE ( 'NONE', #13624, #46626, #31056, .T. ) ;
#12989 = CARTESIAN_POINT ( 'NONE',  ( -11.15651104234136781, -18.05456883900698983, 57.95147637344698666 ) ) ;
#12990 = CARTESIAN_POINT ( 'NONE',  ( -18.41784385650552736, -9.790100578890868377, 49.79778022625163203 ) ) ;
#12991 = CARTESIAN_POINT ( 'NONE',  ( -28.42409385541305511, -25.10920654474410441, 52.99999999999997158 ) ) ;
#12992 = CARTESIAN_POINT ( 'NONE',  ( -18.69178539469224987, -19.32099559247695097, 49.52966884056656482 ) ) ;
#12993 = CARTESIAN_POINT ( 'NONE',  ( -19.78161167002369325, -21.87648970866461440, 65.64203102478617780 ) ) ;
#12994 = CARTESIAN_POINT ( 'NONE',  ( -23.04402284766838349, -19.06632961612601918, 59.16938527523783620 ) ) ;
#12995 = ORIENTED_EDGE ( 'NONE', *, *, #17828, .F. ) ;
#12996 = ORIENTED_EDGE ( 'NONE', *, *, #37471, .T. ) ;
#12997 = ADVANCED_FACE ( 'NONE', ( #20464 ), #42867, .T. ) ;
#12998 = CARTESIAN_POINT ( 'NONE',  ( -10.61707248396235315, -11.78131495581930999, 74.60194320761131337 ) ) ;
#12999 = DIRECTION ( 'NONE',  ( 0.000000000000000000, 0.000000000000000000, 1.000000000000000000 ) ) ;
#13000 = CARTESIAN_POINT ( 'NONE',  ( -21.96934083826521444, -20.13288636094451789, 58.77945318984681933 ) ) ;
#13001 = CARTESIAN_POINT ( 'NONE',  ( -20.64578759472022540, -21.08007238041850684, 58.64475173743925751 ) ) ;
#13002 = DIRECTION ( 'NONE',  ( 2.866981220435666553E-17, -1.000000000000000000, -1.190614954331866791E-16 ) ) ;
#13003 = ADVANCED_FACE ( 'NONE', ( #16974 ), #1228, .T. ) ;
#13004 = CARTESIAN_POINT ( 'NONE',  ( -11.06587071220225660, -11.88109531467702773, 71.16148941250592941 ) ) ;
#13005 = VECTOR ( 'NONE', #4004, 1000.000000000000000 ) ;
#13006 = B_SPLINE_CURVE_WITH_KNOTS ( 'NONE', 1,
 ( #11920, #8457 ),
 .UNSPECIFIED., .F., .F.,
 ( 2, 2 ),
 ( 0.000000000000000000, 1.000000000000000000 ),
 .UNSPECIFIED. ) ;
#13007 = ORIENTED_EDGE ( 'NONE', *, *, #18349, .T. ) ;
#13008 = DIRECTION ( 'NONE',  ( 1.000000000000000000, 0.000000000000000000, 0.000000000000000000 ) ) ;
#13009 = CARTESIAN_POINT ( 'NONE',  ( -15.62914763455529332, -21.57516310569510054, 72.23678623017254097 ) ) ;
#13010 = LINE ( 'NONE', #5406, #40591 ) ;
#13011 =( BOUNDED_SURFACE ( )  B_SPLINE_SURFACE ( 3, 1, ( 
 ( #15960, #22392 ),
 ( #23370, #482 ),
 ( #26331, #23139 ),
 ( #15717, #37896 ),
 ( #14980, #37386 ),
 ( #30774, #26578 ),
 ( #38129, #4406 ) ),
 .UNSPECIFIED., .T., .F., .F. ) 
 B_SPLINE_SURFACE_WITH_KNOTS ( ( 4, 3, 4 ),
 ( 2, 2 ),
 ( 0.000000000000000000, 0.5000000000000000000, 1.000000000000000000 ),
 ( 0.000000000000000000, 1.000000000000000000 ),
 .UNSPECIFIED. ) 
 GEOMETRIC_REPRESENTATION_ITEM ( )  RATIONAL_B_SPLINE_SURFACE ( (
 ( 1.000000000000000000, 1.000000000000000000),
 ( 0.3333333333333335369, 0.3333333333333330373),
 ( 0.3333333333333335369, 0.3333333333333330373),
 ( 1.000000000000000000, 1.000000000000000000),
 ( 0.3333333333333333703, 0.3333333333333333703),
 ( 0.3333333333333333703, 0.3333333333333333703),
 ( 1.000000000000000000, 1.000000000000000000) ) ) 
 REPRESENTATION_ITEM ( '' )  SURFACE ( )  );
#13012 = EDGE_CURVE ( 'NONE', #39661, #43615, #47348, .T. ) ;
#13013 = ORIENTED_EDGE ( 'NONE', *, *, #29269, .T. ) ;
#13014 = EDGE_CURVE ( 'NONE', #25854, #1499, #32676, .T. ) ;
#13015 = CARTESIAN_POINT ( 'NONE',  ( -23.58371808145649950, -11.48100254794470310, 69.96381055508895486 ) ) ;
#13016 = LINE ( 'NONE', #8625, #18806 ) ;
#13017 = EDGE_CURVE ( 'NONE', #41929, #26221, #31539, .T. ) ;
#13018 = CARTESIAN_POINT ( 'NONE',  ( -17.84575570470781258, -7.371070506658266908, 60.33706685437874739 ) ) ;
#13019 = CARTESIAN_POINT ( 'NONE',  ( -22.68104036972259507, -20.08820309574320362, 69.36692159779713052 ) ) ;
#13020 = CARTESIAN_POINT ( 'NONE',  ( -22.38659385759799036, -7.222650657624104298, 49.61879703869476543 ) ) ;
#13021 =( BOUNDED_CURVE ( )  B_SPLINE_CURVE ( 3, ( #37623, #46011, #12264, #26816 ),
 .UNSPECIFIED., .F., .F. ) 
 B_SPLINE_CURVE_WITH_KNOTS ( ( 4, 4 ),
 ( 0.9074455897393673975, 1.000000000000000000 ),
 .UNSPECIFIED. ) 
 CURVE ( )  GEOMETRIC_REPRESENTATION_ITEM ( )  RATIONAL_B_SPLINE_CURVE ( ( 0.6983129098261030565, 0.7760317562607068620, 0.8765941196520058432, 1.000000000000000000 ) ) 
 REPRESENTATION_ITEM ( '' )  );
#13022 = ORIENTED_EDGE ( 'NONE', *, *, #31358, .F. ) ;
#13023 = B_SPLINE_CURVE_WITH_KNOTS ( 'NONE', 1,
 ( #33925, #37605 ),
 .UNSPECIFIED., .F., .F.,
 ( 2, 2 ),
 ( 0.000000000000000000, 1.000000000000000000 ),
 .UNSPECIFIED. ) ;
#13024 = CARTESIAN_POINT ( 'NONE',  ( -13.17078218117215549, -9.186392337449538203, 67.39414915108072535 ) ) ;
#13025 = ORIENTED_EDGE ( 'NONE', *, *, #19904, .F. ) ;
#13026 = DIRECTION ( 'NONE',  ( -1.000000000000000000, 0.000000000000000000, 0.000000000000000000 ) ) ;
#13027 = CYLINDRICAL_SURFACE ( 'NONE', #45507, 0.1499999999999984401 ) ;
#13028 = ORIENTED_EDGE ( 'NONE', *, *, #40997, .T. ) ;
#13029 = CARTESIAN_POINT ( 'NONE',  ( -15.88659385541290447, -7.222650657623934656, 49.61879703869460201 ) ) ;
#13030 = CARTESIAN_POINT ( 'NONE',  ( -12.64201450438284624, -19.99346662158319887, 72.22142341168820678 ) ) ;
#13031 = ORIENTED_EDGE ( 'NONE', *, *, #16274, .T. ) ;
#13032 = CARTESIAN_POINT ( 'NONE',  ( -21.06635048418738165, -21.30826373965517817, 62.29966805574095901 ) ) ;
#13033 = CARTESIAN_POINT ( 'NONE',  ( -14.79922921121938195, -7.836842249070715916, 57.03495322699122738 ) ) ;
#13034 = DIRECTION ( 'NONE',  ( -0.5097212845717550289, 0.8603395911234817950, 0.000000000000000000 ) ) ;
#13035 = EDGE_LOOP ( 'NONE', ( #10533, #25830, #2928, #40089, #13937 ) ) ;
#13036 = CARTESIAN_POINT ( 'NONE',  ( -24.18037300165767434, -17.94870813986570113, 59.18873840842728384 ) ) ;
#13037 =( BOUNDED_CURVE ( )  B_SPLINE_CURVE ( 3, ( #91, #41196, #12132, #807 ),
 .UNSPECIFIED., .F., .F. ) 
 B_SPLINE_CURVE_WITH_KNOTS ( ( 4, 4 ),
 ( 0.4074455897393615689, 0.5000000000000000000 ),
 .UNSPECIFIED. ) 
 CURVE ( )  GEOMETRIC_REPRESENTATION_ITEM ( )  RATIONAL_B_SPLINE_CURVE ( ( 0.6983129098260865142, 0.7760317562606893205, 0.8765941196519929646, 0.9999999999999950040 ) ) 
 REPRESENTATION_ITEM ( '' )  );
#13038 = DIRECTION ( 'NONE',  ( 3.071710424422018052E-17, -6.404604876783311476E-16, -1.000000000000000000 ) ) ;
#13039 = CARTESIAN_POINT ( 'NONE',  ( -24.76961015134066102, -16.05258769581026002, 66.26336133875032885 ) ) ;
#13040 = EDGE_LOOP ( 'NONE', ( #8574, #10992, #12916, #48404, #33301 ) ) ;
#13041 = ORIENTED_EDGE ( 'NONE', *, *, #40709, .T. ) ;
#13042 = LINE ( 'NONE', #20700, #27505 ) ;
#13043 = PLANE ( 'NONE',  #13178 ) ;
#13044 = ORIENTED_EDGE ( 'NONE', *, *, #34654, .T. ) ;
#13045 = DIRECTION ( 'NONE',  ( -3.071710424422018668E-17, 6.404604876783312462E-16, 1.000000000000000000 ) ) ;
#13046 = DIRECTION ( 'NONE',  ( -3.071710424422018668E-17, 6.404604876783312462E-16, 1.000000000000000000 ) ) ;
#13047 = CARTESIAN_POINT ( 'NONE',  ( -18.89909385759798965, -8.105421454601382081, 49.25000573077640098 ) ) ;
#13048 = CARTESIAN_POINT ( 'NONE',  ( -13.03317698800707802, -8.790695117698408723, 64.10935296935409156 ) ) ;
#13049 = CARTESIAN_POINT ( 'NONE',  ( -22.48114103837971101, -19.64927616005747879, 72.64400547034465205 ) ) ;
#13050 = CARTESIAN_POINT ( 'NONE',  ( -33.52409385541305653, -6.359206544744109735, 51.54999999999998295 ) ) ;
#13051 = VERTEX_POINT ( 'NONE', #1491 ) ;
#13052 = ADVANCED_FACE ( 'NONE', ( #9138 ), #6284, .T. ) ;
#13053 = FACE_OUTER_BOUND ( 'NONE', #41126, .T. ) ;
#13054 = CARTESIAN_POINT ( 'NONE',  ( -18.78584198798900928, -7.883846953673406155, 63.58656136513857149 ) ) ;
#13055 = CARTESIAN_POINT ( 'NONE',  ( -22.88264614489240856, -10.34704276773305764, 63.35713876973677827 ) ) ;
#13056 = CARTESIAN_POINT ( 'NONE',  ( -12.86353962931362283, -9.432586330540292607, 74.33395128836551180 ) ) ;
#13057 = CARTESIAN_POINT ( 'NONE',  ( -13.45042104576995889, -20.57396378630483369, 61.62719528072427266 ) ) ;
#13058 = EDGE_LOOP ( 'NONE', ( #26669, #25019, #1840, #16972, #11633 ) ) ;
#13059 = ORIENTED_EDGE ( 'NONE', *, *, #12721, .T. ) ;
#13060 = ORIENTED_EDGE ( 'NONE', *, *, #11942, .F. ) ;
#13061 = CARTESIAN_POINT ( 'NONE',  ( -35.32409385541306079, -8.109206544744111511, 49.44999999999998863 ) ) ;
#13062 = CARTESIAN_POINT ( 'NONE',  ( -18.92057809895272058, -7.919864474132484844, 66.90071783790342863 ) ) ;
#13063 = CARTESIAN_POINT ( 'NONE',  ( -20.04849592361258104, -21.35284569240296548, 72.69006679631317525 ) ) ;
#13064 = ORIENTED_EDGE ( 'NONE', *, *, #48070, .T. ) ;
#13065 = EDGE_CURVE ( 'NONE', #29117, #15587, #16323, .T. ) ;
#13066 = CARTESIAN_POINT ( 'NONE',  ( -10.43656090296491179, -14.37069206989541392, 68.08629950323120283 ) ) ;
#13067 = AXIS2_PLACEMENT_3D ( 'NONE', #43324, #35425, #46537 ) ;
#13068 = VECTOR ( 'NONE', #12724, 1000.000000000000114 ) ;
#13069 = CARTESIAN_POINT ( 'NONE',  ( -9.994877497295997060, -15.37525289974553289, 57.75448116320448833 ) ) ;
#13070 = EDGE_CURVE ( 'NONE', #33767, #43808, #5919, .T. ) ;
#13071 = EDGE_CURVE ( 'NONE', #936, #25681, #36445, .T. ) ;
#13072 = ORIENTED_EDGE ( 'NONE', *, *, #7848, .F. ) ;
#13073 = CARTESIAN_POINT ( 'NONE',  ( -11.32469277870022850, -18.34471304272907588, 58.10714594244493725 ) ) ;
#13074 = FACE_OUTER_BOUND ( 'NONE', #33793, .T. ) ;
#13075 = VERTEX_POINT ( 'NONE', #21186 ) ;
#13076 = DIRECTION ( 'NONE',  ( 0.000000000000000000, 0.000000000000000000, -1.000000000000000000 ) ) ;
#13077 = EDGE_LOOP ( 'NONE', ( #46836, #30320, #6332, #2004, #45342, #47167, #10668, #15210, #3770, #13022, #45494, #46483 ) ) ;
#13078 = DIRECTION ( 'NONE',  ( 0.000000000000000000, 1.000000000000000000, 0.000000000000000000 ) ) ;
#13079 = ORIENTED_EDGE ( 'NONE', *, *, #1212, .F. ) ;
#13080 = DIRECTION ( 'NONE',  ( -3.549360974551879847E-17, 6.371834667872723308E-18, 1.000000000000000000 ) ) ;
#13081 = LINE ( 'NONE', #9418, #39336 ) ;
#13082 = CARTESIAN_POINT ( 'NONE',  ( -11.68672710392437608, -10.05669134056747005, 67.68392285705759548 ) ) ;
#13083 = VERTEX_POINT ( 'NONE', #17942 ) ;
#13084 = CARTESIAN_POINT ( 'NONE',  ( -35.42409385541304800, -9.359200813967566646, 50.49621490985803263 ) ) ;
#13085 = CARTESIAN_POINT ( 'NONE',  ( -24.42401512807229125, -14.72416121340251571, 62.99679879080087375 ) ) ;
#13086 = CARTESIAN_POINT ( 'NONE',  ( -24.08271688320076720, -11.46738811444140538, 63.11251657512028146 ) ) ;
#13087 = DIRECTION ( 'NONE',  ( 0.000000000000000000, 0.9999954153791273948, 0.003028072113819836077 ) ) ;
#13088 = CARTESIAN_POINT ( 'NONE',  ( -10.46375309629256201, -15.55739590339904233, 61.32172507360417057 ) ) ;
#13089 = CARTESIAN_POINT ( 'NONE',  ( -18.92409385541305511, -15.80920654474410725, 52.21286476528345588 ) ) ;
#13090 = ORIENTED_EDGE ( 'NONE', *, *, #2839, .F. ) ;
#13091 = CARTESIAN_POINT ( 'NONE',  ( -23.80521486491402428, -10.96423656519770340, 73.51193299235829670 ) ) ;
#13092 = CARTESIAN_POINT ( 'NONE',  ( -11.84412991438031248, -19.03588838109888570, 71.70188265515885462 ) ) ;
#13093 = CARTESIAN_POINT ( 'NONE',  ( -17.42409385541299471, -14.80920654474435594, 52.02966884056656482 ) ) ;
#13094 = CARTESIAN_POINT ( 'NONE',  ( -23.19948571119275726, -18.85291137746749968, 65.83861571032234394 ) ) ;
#13095 = CARTESIAN_POINT ( 'NONE',  ( -16.44909385650551670, -8.104110260919579645, 48.81699501597546487 ) ) ;
#13096 = EDGE_CURVE ( 'NONE', #38891, #19754, #19163, .T. ) ;
#13097 = ORIENTED_EDGE ( 'NONE', *, *, #11107, .T. ) ;
#13098 = CARTESIAN_POINT ( 'NONE',  ( -16.48446094845526488, -7.818459999738816002, 60.29208735039289735 ) ) ;
#13099 = CARTESIAN_POINT ( 'NONE',  ( -24.42398663107514523, -15.65075326911586906, 73.01775867260030850 ) ) ;
#13100 = ORIENTED_EDGE ( 'NONE', *, *, #29970, .F. ) ;
#13101 = CARTESIAN_POINT ( 'NONE',  ( -21.99178428503402216, -9.439038574390064440, 60.02171213140444195 ) ) ;
#13102 = CARTESIAN_POINT ( 'NONE',  ( -23.49945856589985027, -11.21686614839013885, 66.57781614479455357 ) ) ;
#13103 = CARTESIAN_POINT ( 'NONE',  ( -12.63116919492461854, -9.104687665260810192, 70.96270001146038453 ) ) ;
#13104 = FACE_OUTER_BOUND ( 'NONE', #1044, .T. ) ;
#13105 = PLANE ( 'NONE',  #37596 ) ;
#13106 = ORIENTED_EDGE ( 'NONE', *, *, #19160, .T. ) ;
#13107 = CARTESIAN_POINT ( 'NONE',  ( -12.10973142303912908, -9.588019877982702610, 57.19597242491963840 ) ) ;
#13108 = DIRECTION ( 'NONE',  ( 1.224646799147353207E-16, 1.000000000000000000, -1.912410701131276611E-32 ) ) ;
#13109 = VECTOR ( 'NONE', #24735, 1000.000000000000000 ) ;
#13110 = CARTESIAN_POINT ( 'NONE',  ( -23.70099262725067746, -17.91056972029587513, 59.23208246994288118 ) ) ;
#13111 = ORIENTED_EDGE ( 'NONE', *, *, #9237, .T. ) ;
#13112 = CARTESIAN_POINT ( 'NONE',  ( -17.15134141312287852, -7.364115244199362920, 70.67531166753866501 ) ) ;
#13113 =( BOUNDED_CURVE ( )  B_SPLINE_CURVE ( 3, ( #23070, #16377, #27474, #38059 ),
 .UNSPECIFIED., .F., .F. ) 
 B_SPLINE_CURVE_WITH_KNOTS ( ( 4, 4 ),
 ( 0.000000000000000000, 0.4074455897393672310 ),
 .UNSPECIFIED. ) 
 CURVE ( )  GEOMETRIC_REPRESENTATION_ITEM ( )  RATIONAL_B_SPLINE_CURVE ( ( 1.000000000000000000, 0.4567392136813307468, 0.3561768502900298783, 0.6983129098260973944 ) ) 
 REPRESENTATION_ITEM ( '' )  );
#13114 = CARTESIAN_POINT ( 'NONE',  ( -23.49719401221368642, -11.32496260901646856, 73.47266466796968132 ) ) ;
#13115 = DIRECTION ( 'NONE',  ( 2.866981220435666553E-17, -1.000000000000000000, -1.190614954331866791E-16 ) ) ;
#13116 = CARTESIAN_POINT ( 'NONE',  ( -10.75774562132040479, -12.66857536220184777, 64.45763188802062871 ) ) ;
#13117 = VERTEX_POINT ( 'NONE', #6405 ) ;
#13118 = ORIENTED_EDGE ( 'NONE', *, *, #44769, .T. ) ;
#13119 = CARTESIAN_POINT ( 'NONE',  ( -19.48659385541304090, -7.222650657624104298, 49.61879703869476543 ) ) ;
#13120 = CARTESIAN_POINT ( 'NONE',  ( -10.91566558191575531, -17.52836192114708425, 64.83559378099900528 ) ) ;
#13121 = CARTESIAN_POINT ( 'NONE',  ( -15.28303595616968913, -7.672713470548185200, 74.19330299898706471 ) ) ;
#13122 = CARTESIAN_POINT ( 'NONE',  ( -11.55573855159262386, -10.21941529800896653, 71.15388400389697665 ) ) ;
#13123 = CARTESIAN_POINT ( 'NONE',  ( -24.44839783832460967, -14.20609194633158623, 69.94715494824646385 ) ) ;
#13124 = EDGE_CURVE ( 'NONE', #40875, #6404, #19503, .T. ) ;
#13125 = CARTESIAN_POINT ( 'NONE',  ( -45.92409385541306222, -13.70421070448076861, 72.76000000000000512 ) ) ;
#13126 = ORIENTED_EDGE ( 'NONE', *, *, #18776, .F. ) ;
#13127 = CARTESIAN_POINT ( 'NONE',  ( -19.35269785843539125, -22.00525528091193195, 58.72496154332668539 ) ) ;
#13128 = CARTESIAN_POINT ( 'NONE',  ( -24.39459507417318562, -17.43899346222085711, 69.66985698250167047 ) ) ;
#13129 = VERTEX_POINT ( 'NONE', #36650 ) ;
#13130 = CARTESIAN_POINT ( 'NONE',  ( -23.83080496556880945, -17.75212211224490133, 59.28906343887996400 ) ) ;
#13131 = CARTESIAN_POINT ( 'NONE',  ( -16.16523928603239924, -21.74967706772850207, 62.05568406594436226 ) ) ;
#13132 = AXIS2_PLACEMENT_3D ( 'NONE', #18376, #45485, #26271 ) ;
#13133 = ORIENTED_EDGE ( 'NONE', *, *, #29378, .F. ) ;
#13134 = EDGE_CURVE ( 'NONE', #24440, #43669, #41484, .T. ) ;
#13135 = ADVANCED_FACE ( 'NONE', ( #10815 ), #13528, .T. ) ;
#13136 = CARTESIAN_POINT ( 'NONE',  ( -19.23866243364646422, -21.62168334911581269, 58.52507384657483414 ) ) ;
#13137 = DIRECTION ( 'NONE',  ( 0.7800143876985550229, -0.6257615799833393666, 5.505484597913564244E-08 ) ) ;
#13138 = ORIENTED_EDGE ( 'NONE', *, *, #9628, .F. ) ;
#13139 = EDGE_CURVE ( 'NONE', #46408, #42407, #32959, .T. ) ;
#13140 = DIRECTION ( 'NONE',  ( -3.964551025433374905E-06, -2.747358590626761473E-07, 0.9999999999921033167 ) ) ;
#13141 = AXIS2_PLACEMENT_3D ( 'NONE', #33288, #15311, #11164 ) ;
#13142 = EDGE_CURVE ( 'NONE', #21061, #20803, #14472, .T. ) ;
#13143 = CARTESIAN_POINT ( 'NONE',  ( -10.69226473215256590, -16.91570156256109669, 61.45743193859061648 ) ) ;
#13144 = CARTESIAN_POINT ( 'NONE',  ( -24.71334378318632830, -13.26952680650525274, 59.47772536435775947 ) ) ;
#13145 = ORIENTED_EDGE ( 'NONE', *, *, #9280, .T. ) ;
#13146 = CARTESIAN_POINT ( 'NONE',  ( -14.40524399388063514, -8.438208624349055498, 67.55975084334407654 ) ) ;
#13147 = CARTESIAN_POINT ( 'NONE',  ( -24.37683854932038585, -15.97618581480151434, 66.21324926630431662 ) ) ;
#13148 = CARTESIAN_POINT ( 'NONE',  ( -21.36489517220793743, -8.963474395264050543, 73.75128753236120360 ) ) ;
#13149 = CARTESIAN_POINT ( 'NONE',  ( -11.60526899143904345, -18.79015832504765626, 68.23161775275829655 ) ) ;
#13150 = CARTESIAN_POINT ( 'NONE',  ( -21.63336539757928634, -9.153348366551478321, 66.94677872351418557 ) ) ;
#13151 = EDGE_CURVE ( 'NONE', #45924, #27231, #332, .T. ) ;
#13152 = CARTESIAN_POINT ( 'NONE',  ( -16.71957921250844592, -21.82421608262117729, 68.71032757591046902 ) ) ;
#13153 = EDGE_LOOP ( 'NONE', ( #23802, #24318 ) ) ;
#13154 = CARTESIAN_POINT ( 'NONE',  ( -13.86149102995237037, -8.266187410065942487, 74.30616366049129340 ) ) ;
#13155 = CARTESIAN_POINT ( 'NONE',  ( -20.12398138731996511, -21.75278012861551247, 72.60489934222226793 ) ) ;
#13156 = CARTESIAN_POINT ( 'NONE',  ( -13.41327373486474883, -20.54621981236622830, 58.04650078084816300 ) ) ;
#13157 =( BOUNDED_CURVE ( )  B_SPLINE_CURVE ( 3, ( #13233, #28286, #39602, #21139 ),
 .UNSPECIFIED., .F., .F. ) 
 B_SPLINE_CURVE_WITH_KNOTS ( ( 4, 4 ),
 ( 0.4074455897393602921, 0.5000000000000000000 ),
 .UNSPECIFIED. ) 
 CURVE ( )  GEOMETRIC_REPRESENTATION_ITEM ( )  RATIONAL_B_SPLINE_CURVE ( ( 0.6983129098260720813, 0.7760317562606737773, 0.8765941196519813072, 0.9999999999999900080 ) ) 
 REPRESENTATION_ITEM ( '' )  );
#13158 = ORIENTED_EDGE ( 'NONE', *, *, #35096, .T. ) ;
#13159 = CARTESIAN_POINT ( 'NONE',  ( -27.42409385541305511, -25.10920654474410441, 81.99999999999998579 ) ) ;
#13160 = ORIENTED_EDGE ( 'NONE', *, *, #39737, .T. ) ;
#13161 = ORIENTED_EDGE ( 'NONE', *, *, #20956, .T. ) ;
#13162 = ORIENTED_EDGE ( 'NONE', *, *, #39849, .F. ) ;
#13163 = DIRECTION ( 'NONE',  ( -3.071710424422018668E-17, 6.404604876783312462E-16, 1.000000000000000000 ) ) ;
#13164 = AXIS2_PLACEMENT_3D ( 'NONE', #22299, #29442, #33856 ) ;
#13165 = CARTESIAN_POINT ( 'NONE',  ( -23.75261229635691862, -11.81743247384379991, 59.76770420102489823 ) ) ;
#13166 = CARTESIAN_POINT ( 'NONE',  ( -17.36778503871311230, -7.359366238864594401, 67.21313763515482265 ) ) ;
#13167 = CARTESIAN_POINT ( 'NONE',  ( 18.54465614458695200, 3.140741878271521070, 50.53406581128081143 ) ) ;
#13168 = LINE ( 'NONE', #1626, #41714 ) ;
#13169 =( BOUNDED_CURVE ( )  B_SPLINE_CURVE ( 3, ( #5629, #20639, #35634, #31952 ),
 .UNSPECIFIED., .F., .F. ) 
 B_SPLINE_CURVE_WITH_KNOTS ( ( 4, 4 ),
 ( 0.5000000000000000000, 0.9074455897393722825 ),
 .UNSPECIFIED. ) 
 CURVE ( )  GEOMETRIC_REPRESENTATION_ITEM ( )  RATIONAL_B_SPLINE_CURVE ( ( 0.9999999999999791278, 0.4567392136813193115, 0.3561768502900400923, 0.6983129098261189327 ) ) 
 REPRESENTATION_ITEM ( '' )  );
#13170 = EDGE_LOOP ( 'NONE', ( #10073, #20002 ) ) ;
#13171 = ORIENTED_EDGE ( 'NONE', *, *, #591, .T. ) ;
#13172 = CARTESIAN_POINT ( 'NONE',  ( -21.37409385650551741, -9.792211528768504536, 50.49490371617623197 ) ) ;
#13173 = CARTESIAN_POINT ( 'NONE',  ( -13.85393650630732054, -8.270265118416840977, 74.38450092284953996 ) ) ;
#13174 = AXIS2_PLACEMENT_3D ( 'NONE', #5734, #6681, #17015 ) ;
#13175 = PLANE ( 'NONE',  #9536 ) ;
#13176 = ADVANCED_FACE ( 'NONE', ( #43846 ), #14243, .F. ) ;
#13177 = CARTESIAN_POINT ( 'NONE',  ( -21.59909385650551528, -8.114302828567740988, 52.18300498402516041 ) ) ;
#13178 = AXIS2_PLACEMENT_3D ( 'NONE', #28806, #43844, #28074 ) ;
#13179 = ORIENTED_EDGE ( 'NONE', *, *, #41129, .F. ) ;
#13180 = DIRECTION ( 'NONE',  ( 1.000000000000000000, 0.000000000000000000, 0.000000000000000000 ) ) ;
#13181 = ADVANCED_FACE ( 'NONE', ( #25359 ), #6884, .T. ) ;
#13182 = CARTESIAN_POINT ( 'NONE',  ( -24.72409385541305582, -14.90920654474416729, 63.03529411764704804 ) ) ;
#13183 = CARTESIAN_POINT ( 'NONE',  ( -11.64235247690698749, -18.84330696305777408, 68.51689631558762983 ) ) ;
#13184 = ORIENTED_EDGE ( 'NONE', *, *, #48245, .T. ) ;
#13185 = CYLINDRICAL_SURFACE ( 'NONE', #35125, 2.000000000000008882 ) ;
#13186 = DIRECTION ( 'NONE',  ( 3.298726456874245264E-06, -1.683524832386861475E-06, -0.9999999999931420414 ) ) ;
#13187 = CARTESIAN_POINT ( 'NONE',  ( -16.20683845212634111, -21.70255763714999020, 58.58585572420326315 ) ) ;
#13188 = LINE ( 'NONE', #39559, #12944 ) ;
#13189 = EDGE_CURVE ( 'NONE', #22471, #45412, #16793, .T. ) ;
#13190 = EDGE_LOOP ( 'NONE', ( #41093, #30734 ) ) ;
#13191 = AXIS2_PLACEMENT_3D ( 'NONE', #34954, #8635, #28317 ) ;
#13192 = CARTESIAN_POINT ( 'NONE',  ( -11.07857831884827604, -11.73724749328988359, 71.23860870961335934 ) ) ;
#13193 = EDGE_CURVE ( 'NONE', #32966, #48033, #14974, .T. ) ;
#13194 = CARTESIAN_POINT ( 'NONE',  ( -22.93054552543627977, -10.40195957496224644, 66.95671006072360854 ) ) ;
#13195 = DIRECTION ( 'NONE',  ( 7.381188785182666071E-06, 5.670466977913946987E-06, 0.9999999999566818731 ) ) ;
#13196 = ORIENTED_EDGE ( 'NONE', *, *, #11005, .F. ) ;
#13197 = CYLINDRICAL_SURFACE ( 'NONE', #19731, 0.1500000000000050460 ) ;
#13198 = AXIS2_PLACEMENT_3D ( 'NONE', #46002, #1663, #27038 ) ;
#13199 = VERTEX_POINT ( 'NONE', #3426 ) ;
#13200 = CARTESIAN_POINT ( 'NONE',  ( -14.66404237506551311, -7.889278293989088198, 60.42722112806361423 ) ) ;
#13201 = ADVANCED_FACE ( 'NONE', ( #8119 ), #41594, .T. ) ;
#13202 = VERTEX_POINT ( 'NONE', #34187 ) ;
#13203 = CARTESIAN_POINT ( 'NONE',  ( -10.98557813051190024, -17.68114236276378293, 71.56718193507128944 ) ) ;
#13204 = CARTESIAN_POINT ( 'NONE',  ( -15.56465948913149155, -7.543361525925791788, 54.27966884056655061 ) ) ;
#13205 = CARTESIAN_POINT ( 'NONE',  ( -13.60894707410760240, -8.877133421815647907, 60.85439169328856934 ) ) ;
#13206 = DIRECTION ( 'NONE',  ( 0.9687793358424821033, -0.2479245821708679909, 0.000000000000000000 ) ) ;
#13207 = ORIENTED_EDGE ( 'NONE', *, *, #37086, .F. ) ;
#13208 = CARTESIAN_POINT ( 'NONE',  ( -13.40417755890050699, -20.60086790338396057, 58.34650048655475274 ) ) ;
#13209 = AXIS2_PLACEMENT_3D ( 'NONE', #45112, #15509, #33488 ) ;
#13210 = ADVANCED_FACE ( 'NONE', ( #7138 ), #37139, .T. ) ;
#13211 = DIRECTION ( 'NONE',  ( -0.8603395911234869020, -0.5097212845717467022, 0.000000000000000000 ) ) ;
#13212 = CARTESIAN_POINT ( 'NONE',  ( -15.29626560849200878, -8.084834557582363246, 73.96496852212565898 ) ) ;
#13213 = VERTEX_POINT ( 'NONE', #245 ) ;
#13214 =( BOUNDED_CURVE ( )  B_SPLINE_CURVE ( 3, ( #25226, #43706, #6267, #9729 ),
 .UNSPECIFIED., .F., .F. ) 
 B_SPLINE_CURVE_WITH_KNOTS ( ( 4, 4 ),
 ( 0.000000000000000000, 0.4074455897393638448 ),
 .UNSPECIFIED. ) 
 CURVE ( )  GEOMETRIC_REPRESENTATION_ITEM ( )  RATIONAL_B_SPLINE_CURVE ( ( 1.000000000000000000, 0.4567392136813241965, 0.3561768502900274358, 0.6983129098261096068 ) ) 
 REPRESENTATION_ITEM ( '' )  );
#13215 = CARTESIAN_POINT ( 'NONE',  ( -11.06796828401846078, -18.69550736580278993, 61.53356777548469125 ) ) ;
#13216 = EDGE_LOOP ( 'NONE', ( #47726, #33416 ) ) ;
#13217 = ORIENTED_EDGE ( 'NONE', *, *, #47404, .F. ) ;
#13218 = CARTESIAN_POINT ( 'NONE',  ( -24.08907123645992243, -11.48026457312919391, 63.13713595337925000 ) ) ;
#13219 = CARTESIAN_POINT ( 'NONE',  ( -20.10940917962770769, -21.27365406404410564, 72.59582005363583335 ) ) ;
#13220 = DIRECTION ( 'NONE',  ( -1.000000000000000000, -1.669677910507523057E-21, -6.493791346278465266E-22 ) ) ;
#13221 = CARTESIAN_POINT ( 'NONE',  ( -18.47409385650551528, -9.792211528768504536, 50.49490371617623197 ) ) ;
#13222 = DIRECTION ( 'NONE',  ( 3.413470714839332458E-33, -1.190614954331866791E-16, 1.000000000000000000 ) ) ;
#13223 = CARTESIAN_POINT ( 'NONE',  ( -12.79725882921341551, -20.12850138265567068, 72.10653676770067477 ) ) ;
#13224 = B_SPLINE_CURVE_WITH_KNOTS ( 'NONE', 3,
 ( #11100, #24, #48511, #19454, #34461, #18467, #4207, #30071, #45094, #33470 ),
 .UNSPECIFIED., .F., .F.,
 ( 4, 2, 2, 2, 4 ),
 ( 0.000000000000000000, 0.2500000000000000000, 0.5000000000000000000, 0.7500000000000000000, 1.000000000000000000 ),
 .UNSPECIFIED. ) ;
#13225 = DIRECTION ( 'NONE',  ( -2.168404344971008375E-16, -0.000000000000000000, 1.000000000000000000 ) ) ;
#13226 = CARTESIAN_POINT ( 'NONE',  ( -10.53028993777715883, -16.28642212234895226, 71.73278239416407587 ) ) ;
#13227 = CARTESIAN_POINT ( 'NONE',  ( -13.90630441925721250, -21.37656106130631173, 72.06461169531037569 ) ) ;
#13228 = ORIENTED_EDGE ( 'NONE', *, *, #27195, .T. ) ;
#13229 = ORIENTED_EDGE ( 'NONE', *, *, #38282, .T. ) ;
#13230 = CARTESIAN_POINT ( 'NONE',  ( -11.32522400900782067, -11.27219014254736074, 60.96413645226084554 ) ) ;
#13231 = DIRECTION ( 'NONE',  ( -3.071710424422018668E-17, 6.404604876783312462E-16, 1.000000000000000000 ) ) ;
#13232 = AXIS2_PLACEMENT_3D ( 'NONE', #10861, #11114, #36686 ) ;
#13233 = CARTESIAN_POINT ( 'NONE',  ( -11.42622084110231029, -18.51434063454204093, 61.27710833181470917 ) ) ;
#13234 = FACE_OUTER_BOUND ( 'NONE', #46972, .T. ) ;
#13235 = DIRECTION ( 'NONE',  ( 1.000000000000000000, 2.866981220435666553E-17, 0.000000000000000000 ) ) ;
#13236 = VECTOR ( 'NONE', #4469, 1000.000000000000000 ) ;
#13237 = EDGE_CURVE ( 'NONE', #40280, #19312, #19420, .T. ) ;
#13238 = AXIS2_PLACEMENT_3D ( 'NONE', #33486, #48527, #18734 ) ;
#13239 = AXIS2_PLACEMENT_3D ( 'NONE', #13093, #32323, #28388 ) ;
#13240 = VERTEX_POINT ( 'NONE', #41846 ) ;
#13241 = DIRECTION ( 'NONE',  ( 0.4433615477241706904, -0.8963428685495450354, 2.661652803430218851E-08 ) ) ;
#13242 = CARTESIAN_POINT ( 'NONE',  ( -10.21393201348709212, -12.93341964037237091, 67.89865688031065361 ) ) ;
#13243 = CARTESIAN_POINT ( 'NONE',  ( -10.98557813051190202, -17.68114236276378293, 71.56718193507127523 ) ) ;
#13244 = FACE_OUTER_BOUND ( 'NONE', #16108, .T. ) ;
#13245 = B_SPLINE_CURVE_WITH_KNOTS ( 'NONE', 1,
 ( #29579, #40417 ),
 .UNSPECIFIED., .F., .F.,
 ( 2, 2 ),
 ( 0.000000000000000000, 1.000000000000000000 ),
 .UNSPECIFIED. ) ;
#13246 = ORIENTED_EDGE ( 'NONE', *, *, #5938, .F. ) ;
#13247 = CARTESIAN_POINT ( 'NONE',  ( -11.64547064851736202, -18.85300969848255193, 64.63218190802510321 ) ) ;
#13248 = CARTESIAN_POINT ( 'NONE',  ( -13.53325528467554406, -21.16256411608339150, 65.17124155742401115 ) ) ;
#13249 = DIRECTION ( 'NONE',  ( 2.866981220435666553E-17, -1.000000000000000000, -1.190614954331866791E-16 ) ) ;
#13250 = ADVANCED_FACE ( 'NONE', ( #29784 ), #38126, .T. ) ;
#13251 = CARTESIAN_POINT ( 'NONE',  ( -8.424093855413060439, -6.859206544744110623, 47.99999999999998579 ) ) ;
#13252 = LINE ( 'NONE', #29270, #28094 ) ;
#13253 = ADVANCED_FACE ( 'NONE', ( #34427 ), #18430, .F. ) ;
#13254 = CARTESIAN_POINT ( 'NONE',  ( -14.78597691548102411, -7.841758819152822468, 56.98853511513466685 ) ) ;
#13255 = ORIENTED_EDGE ( 'NONE', *, *, #12666, .T. ) ;
#13256 = EDGE_LOOP ( 'NONE', ( #22517, #30822, #31250, #14396 ) ) ;
#13257 = DIRECTION ( 'NONE',  ( -0.05202058437830281434, 0.9986460127597465153, -1.657953767072174380E-08 ) ) ;
#13258 = ADVANCED_FACE ( 'NONE', ( #44815 ), #26092, .T. ) ;
#13259 = FACE_OUTER_BOUND ( 'NONE', #17409, .T. ) ;
#13260 = ORIENTED_EDGE ( 'NONE', *, *, #21333, .T. ) ;
#13261 = CARTESIAN_POINT ( 'NONE',  ( -10.27563016671317619, -12.71093163253470237, 64.46110259866301817 ) ) ;
#13262 = CARTESIAN_POINT ( 'NONE',  ( -13.83659385650551776, -6.915538690918075382, 49.31353937987644542 ) ) ;
#13263 = VECTOR ( 'NONE', #22013, 1000.000000000000114 ) ;
#13264 = EDGE_LOOP ( 'NONE', ( #9091, #23742, #27695, #30631, #30360 ) ) ;
#13265 = CARTESIAN_POINT ( 'NONE',  ( -12.02400285154091897, -10.35258023360360369, 71.07966224361382501 ) ) ;
#13266 = ADVANCED_FACE ( 'NONE', ( #41103 ), #22898, .F. ) ;
#13267 = CARTESIAN_POINT ( 'NONE',  ( -19.45281838860202228, -9.697037067072804106, 54.07175714974879099 ) ) ;
#13268 = DIRECTION ( 'NONE',  ( -0.000000000000000000, -1.000000000000000000, -0.000000000000000000 ) ) ;
#13269 = ORIENTED_EDGE ( 'NONE', *, *, #2736, .T. ) ;
#13270 = FACE_OUTER_BOUND ( 'NONE', #7839, .T. ) ;
#13271 = AXIS2_PLACEMENT_3D ( 'NONE', #25657, #33267, #37710 ) ;
#13272 = FACE_OUTER_BOUND ( 'NONE', #32001, .T. ) ;
#13273 = CARTESIAN_POINT ( 'NONE',  ( -17.82409385541305369, -14.80920654474410725, 48.99999999999997868 ) ) ;
#13274 = CARTESIAN_POINT ( 'NONE',  ( -23.80321451250838649, -17.81075939459467961, 59.00378417737415049 ) ) ;
#13275 = ORIENTED_EDGE ( 'NONE', *, *, #18531, .F. ) ;
#13276 = VERTEX_POINT ( 'NONE', #4180 ) ;
#13277 = CARTESIAN_POINT ( 'NONE',  ( -10.77303329795002895, -12.62668660113453178, 60.79853568451941470 ) ) ;
#13278 = CARTESIAN_POINT ( 'NONE',  ( -18.57335281209669731, -21.76520412651811043, 72.57038810541313012 ) ) ;
#13279 = VERTEX_POINT ( 'NONE', #22388 ) ;
#13280 = CARTESIAN_POINT ( 'NONE',  ( -24.33438471898804778, -15.92705986081045744, 66.06324874090134358 ) ) ;
#13281 = CARTESIAN_POINT ( 'NONE',  ( -23.25590038356622102, -18.77701127317174112, 62.56226639404914636 ) ) ;
#13282 = VECTOR ( 'NONE', #22943, 1000.000000000000000 ) ;
#13283 = CARTESIAN_POINT ( 'NONE',  ( -17.32409385759798681, -9.359200813967568422, 50.49621490985803263 ) ) ;
#13284 = CARTESIAN_POINT ( 'NONE',  ( -23.82366785274684418, -10.99486113721019009, 73.47697904737684382 ) ) ;
#13285 = ADVANCED_FACE ( 'NONE', ( #33685 ), #30282, .T. ) ;
#13286 = CARTESIAN_POINT ( 'NONE',  ( -10.63418523514201652, -17.87528017975677130, 71.61072290056861789 ) ) ;
#13287 = CARTESIAN_POINT ( 'NONE',  ( -45.92409385541306222, -13.70421070448077039, 70.50000000000000000 ) ) ;
#13288 = ADVANCED_FACE ( 'NONE', ( #30040 ), #24555, .T. ) ;
#13289 = ORIENTED_EDGE ( 'NONE', *, *, #15489, .F. ) ;
#13290 = CARTESIAN_POINT ( 'NONE',  ( -45.37196614242555626, -14.20920654474410760, 70.87000000000000455 ) ) ;
#13291 = CARTESIAN_POINT ( 'NONE',  ( -24.48495216189764534, -12.43291116107568861, 73.39225569044465658 ) ) ;
#13292 = CARTESIAN_POINT ( 'NONE',  ( -13.51031689544038805, -20.61338442564125728, 61.80029829250916151 ) ) ;
#13293 =( BOUNDED_CURVE ( )  B_SPLINE_CURVE ( 3, ( #32266, #29525, #2925, #29040 ),
 .UNSPECIFIED., .F., .F. ) 
 B_SPLINE_CURVE_WITH_KNOTS ( ( 4, 4 ),
 ( 0.9074455897393689519, 1.000000000000000000 ),
 .UNSPECIFIED. ) 
 CURVE ( )  GEOMETRIC_REPRESENTATION_ITEM ( )  RATIONAL_B_SPLINE_CURVE ( ( 0.6983129098261018353, 0.7760317562607057518, 0.8765941196520051770, 1.000000000000000000 ) ) 
 REPRESENTATION_ITEM ( '' )  );
#13294 = ORIENTED_EDGE ( 'NONE', *, *, #41059, .F. ) ;
#13295 = ORIENTED_EDGE ( 'NONE', *, *, #14834, .T. ) ;
#13296 = ORIENTED_EDGE ( 'NONE', *, *, #30967, .F. ) ;
#13297 = CARTESIAN_POINT ( 'NONE',  ( -17.65810221059773610, -7.762793303104815301, 63.56529088875731759 ) ) ;
#13298 = FILL_AREA_STYLE_COLOUR ( '', #33109 ) ;
#13299 = VECTOR ( 'NONE', #47940, 1000.000000000000114 ) ;
#13300 = CARTESIAN_POINT ( 'NONE',  ( -21.70317610893864924, -9.269322718887449852, 63.41827076980987954 ) ) ;
#13301 =( BOUNDED_SURFACE ( )  B_SPLINE_SURFACE ( 3, 1, ( 
 ( #46161, #46890 ),
 ( #4805, #39011 ),
 ( #867, #34580 ),
 ( #12902, #38260 ),
 ( #1328, #8494 ),
 ( #24009, #9228 ),
 ( #38768, #5287 ) ),
 .UNSPECIFIED., .T., .F., .F. ) 
 B_SPLINE_SURFACE_WITH_KNOTS ( ( 4, 3, 4 ),
 ( 2, 2 ),
 ( 0.000000000000000000, 0.5000000000000000000, 1.000000000000000000 ),
 ( 0.000000000000000000, 1.000000000000000000 ),
 .UNSPECIFIED. ) 
 GEOMETRIC_REPRESENTATION_ITEM ( )  RATIONAL_B_SPLINE_SURFACE ( (
 ( 1.000000000000000000, 1.000000000000000000),
 ( 0.3333333333333335369, 0.3333333333333330373),
 ( 0.3333333333333335369, 0.3333333333333330373),
 ( 1.000000000000000000, 1.000000000000000000),
 ( 0.3333333333333333703, 0.3333333333333333703),
 ( 0.3333333333333333703, 0.3333333333333333703),
 ( 1.000000000000000000, 1.000000000000000000) ) ) 
 REPRESENTATION_ITEM ( '' )  SURFACE ( )  );
#13302 = EDGE_LOOP ( 'NONE', ( #23631, #27053 ) ) ;
#13303 =( BOUNDED_SURFACE ( )  B_SPLINE_SURFACE ( 3, 1, ( 
 ( #7779, #30671 ),
 ( #3832, #41986 ),
 ( #38258, #45206 ),
 ( #4547, #12184 ),
 ( #27201, #8492 ),
 ( #33592, #48632 ),
 ( #44970, #41246 ) ),
 .UNSPECIFIED., .T., .F., .F. ) 
 B_SPLINE_SURFACE_WITH_KNOTS ( ( 4, 3, 4 ),
 ( 2, 2 ),
 ( 0.000000000000000000, 0.5000000000000000000, 1.000000000000000000 ),
 ( 0.000000000000000000, 1.000000000000000000 ),
 .UNSPECIFIED. ) 
 GEOMETRIC_REPRESENTATION_ITEM ( )  RATIONAL_B_SPLINE_SURFACE ( (
 ( 1.000000000000000000, 1.000000000000000000),
 ( 0.3333333333333335369, 0.3333333333333330373),
 ( 0.3333333333333335369, 0.3333333333333330373),
 ( 1.000000000000000000, 1.000000000000000000),
 ( 0.3333333333333333703, 0.3333333333333333703),
 ( 0.3333333333333333703, 0.3333333333333333703),
 ( 1.000000000000000000, 1.000000000000000000) ) ) 
 REPRESENTATION_ITEM ( '' )  SURFACE ( )  );
#13304 = CIRCLE ( 'NONE', #30651, 1.249999999999999334 ) ;
#13305 = AXIS2_PLACEMENT_3D ( 'NONE', #28635, #46864, #2283 ) ;
#13306 = CARTESIAN_POINT ( 'NONE',  ( -16.18458696102261385, -7.463033837898945144, 60.40017247762416019 ) ) ;
#13307 = DIRECTION ( 'NONE',  ( 2.866981220435666553E-17, -1.000000000000000000, -1.190614954331866791E-16 ) ) ;
#13308 = ORIENTED_EDGE ( 'NONE', *, *, #34768, .T. ) ;
#13309 = CARTESIAN_POINT ( 'NONE',  ( -18.53667165497532920, -10.24437071140731170, 49.52966884056655772 ) ) ;
#13310 = AXIS2_PLACEMENT_3D ( 'NONE', #15832, #34797, #27409 ) ;
#13311 = CARTESIAN_POINT ( 'NONE',  ( -12.56699215081136600, -20.45835600996747417, 71.92840931458714238 ) ) ;
#13312 = VERTEX_POINT ( 'NONE', #12041 ) ;
#13313 = CARTESIAN_POINT ( 'NONE',  ( -21.96667192285332604, -8.904124347047575938, 66.80116649577588817 ) ) ;
#13314 = B_SPLINE_CURVE_WITH_KNOTS ( 'NONE', 3,
 ( #32061, #47083, #8937, #42907, #13324, #38959, #20249, #1532, #16539, #46611 ),
 .UNSPECIFIED., .F., .F.,
 ( 4, 2, 2, 2, 4 ),
 ( 0.6272669072977246074, 0.7522669073147544294, 0.8772669073317842514, 1.002266907348813962, 1.127266907365843895 ),
 .UNSPECIFIED. ) ;
#13315 = VERTEX_POINT ( 'NONE', #23367 ) ;
#13316 = CARTESIAN_POINT ( 'NONE',  ( -13.52595587147657596, -21.15804559846413824, 65.09290550380976015 ) ) ;
#13317 =( BOUNDED_CURVE ( )  B_SPLINE_CURVE ( 3, ( #29951, #3348, #14393, #11233 ),
 .UNSPECIFIED., .F., .F. ) 
 B_SPLINE_CURVE_WITH_KNOTS ( ( 4, 4 ),
 ( 0.9074455897393632897, 1.000000000000000000 ),
 .UNSPECIFIED. ) 
 CURVE ( )  GEOMETRIC_REPRESENTATION_ITEM ( )  RATIONAL_B_SPLINE_CURVE ( ( 0.6983129098260950629, 0.7760317562606999786, 0.8765941196520016243, 1.000000000000000000 ) ) 
 REPRESENTATION_ITEM ( '' )  );
#13318 = ORIENTED_EDGE ( 'NONE', *, *, #41790, .F. ) ;
#13319 = CARTESIAN_POINT ( 'NONE',  ( -11.90871160445621868, -19.81768789853573054, 58.10495117216805738 ) ) ;
#13320 = PLANE ( 'NONE',  #33021 ) ;
#13321 = EDGE_CURVE ( 'NONE', #46319, #40340, #29557, .T. ) ;
#13322 = FACE_OUTER_BOUND ( 'NONE', #9047, .T. ) ;
#13323 = ORIENTED_EDGE ( 'NONE', *, *, #37392, .F. ) ;
#13324 = CARTESIAN_POINT ( 'NONE',  ( -24.26779606828610270, -17.75336464367330080, 62.59548250328385421 ) ) ;
#13325 = CARTESIAN_POINT ( 'NONE',  ( -24.70163917427996481, -16.40367249003021755, 59.26185880907539882 ) ) ;
#13326 = CARTESIAN_POINT ( 'NONE',  ( -45.55409385541306477, -13.72754205882879042, 70.96013658682592506 ) ) ;
#13327 = ADVANCED_FACE ( 'NONE', ( #16193 ), #1430, .F. ) ;
#13328 = CARTESIAN_POINT ( 'NONE',  ( -14.78754716229542865, -8.270772359302402066, 60.31996282000578447 ) ) ;
#13329 = LINE ( 'NONE', #9673, #23738 ) ;
#13330 = DIRECTION ( 'NONE',  ( 1.224646799147353207E-16, 1.000000000000000000, -1.912410701131276611E-32 ) ) ;
#13331 = ORIENTED_EDGE ( 'NONE', *, *, #28474, .F. ) ;
#13332 = CARTESIAN_POINT ( 'NONE',  ( -14.99687845949598319, -8.186362001186598292, 60.41176252006127356 ) ) ;
#13333 = CARTESIAN_POINT ( 'NONE',  ( -14.96223302779666398, -10.63593772014186278, 49.52966884056655772 ) ) ;
#13334 = CYLINDRICAL_SURFACE ( 'NONE', #38413, 0.1500000000000028533 ) ;
#13335 = DIRECTION ( 'NONE',  ( 0.8967515337576289491, -0.4425343904188010491, 9.546469656967252871E-09 ) ) ;
#13336 = CARTESIAN_POINT ( 'NONE',  ( -18.05534385759799321, -8.623186033802570094, 49.24843789510466507 ) ) ;
#13337 = CARTESIAN_POINT ( 'NONE',  ( -13.91784385650551670, -9.790100578890868377, 49.79778022625163203 ) ) ;
#13338 = ORIENTED_EDGE ( 'NONE', *, *, #12304, .T. ) ;
#13339 = CARTESIAN_POINT ( 'NONE',  ( -16.22041545928731310, -7.375544130475720550, 53.94122439512140943 ) ) ;
#13340 = DIRECTION ( 'NONE',  ( 2.866981220435666553E-17, -1.000000000000000000, -1.190614954331866791E-16 ) ) ;
#13341 = ORIENTED_EDGE ( 'NONE', *, *, #33515, .F. ) ;
#13342 = CARTESIAN_POINT ( 'NONE',  ( -9.973354012397450674, -14.79738236791871664, 71.44127436690867228 ) ) ;
#13343 = CARTESIAN_POINT ( 'NONE',  ( -10.13226805943771858, -16.33660356775173739, 71.49104427242312454 ) ) ;
#13344 = CARTESIAN_POINT ( 'NONE',  ( -14.58888777286794358, -8.408946862453658966, 64.08978847350323349 ) ) ;
#13345 = CARTESIAN_POINT ( 'NONE',  ( -14.72778340125292651, -21.32322296975913645, 58.46617885012762628 ) ) ;
#13346 = CARTESIAN_POINT ( 'NONE',  ( -23.78676187654788521, -10.93361199230012559, 73.54688693628270357 ) ) ;
#13347 = ORIENTED_EDGE ( 'NONE', *, *, #40612, .T. ) ;
#13348 = EDGE_CURVE ( 'NONE', #34852, #25804, #1186, .T. ) ;
#13349 = CARTESIAN_POINT ( 'NONE',  ( -23.76773510245185506, -11.84597926658418565, 63.14145293063592845 ) ) ;
#13350 = VECTOR ( 'NONE', #34925, 1000.000000000000000 ) ;
#13351 = EDGE_CURVE ( 'NONE', #17537, #17620, #16684, .T. ) ;
#13352 = LINE ( 'NONE', #31357, #26522 ) ;
#13353 = CARTESIAN_POINT ( 'NONE',  ( -23.74125327615269754, -17.82500477549296036, 59.00378426403860033 ) ) ;
#13354 = EDGE_CURVE ( 'NONE', #23394, #34714, #31237, .T. ) ;
#13355 = EDGE_CURVE ( 'NONE', #25477, #10558, #6778, .T. ) ;
#13356 = ADVANCED_FACE ( 'NONE', ( #38361 ), #30999, .F. ) ;
#13357 = VERTEX_POINT ( 'NONE', #1922 ) ;
#13358 = CARTESIAN_POINT ( 'NONE',  ( -19.04784696903935881, -9.816619457272706128, 49.52966884056655772 ) ) ;
#13359 = CARTESIAN_POINT ( 'NONE',  ( -15.90376647335224192, -7.921387445786724157, 70.70170099352583293 ) ) ;
#13360 = AXIS2_PLACEMENT_3D ( 'NONE', #20764, #32799, #29116 ) ;
#13361 = CARTESIAN_POINT ( 'NONE',  ( -50.42609385541305755, -14.80920654474421205, 67.95882352941174531 ) ) ;
#13362 = CARTESIAN_POINT ( 'NONE',  ( -21.15336504700141163, -20.73310185707507713, 69.05450185101547333 ) ) ;
#13363 = CARTESIAN_POINT ( 'NONE',  ( -47.17409385541305511, -14.80920654474410725, 70.50000000000000000 ) ) ;
#13364 = CARTESIAN_POINT ( 'NONE',  ( -10.12541953518153370, -16.30314513718451508, 71.59750380059928432 ) ) ;
#13365 = ORIENTED_EDGE ( 'NONE', *, *, #25374, .T. ) ;
#13366 = ORIENTED_EDGE ( 'NONE', *, *, #33378, .T. ) ;
#13367 = CARTESIAN_POINT ( 'NONE',  ( -16.44909385541304303, -8.112991634885936776, 51.74999426922421719 ) ) ;
#13368 = CARTESIAN_POINT ( 'NONE',  ( -10.78898398081525301, -17.19290454168847404, 61.44271037915215317 ) ) ;
#13369 = CARTESIAN_POINT ( 'NONE',  ( -15.43182990062313742, -8.046249867383863830, 74.36513541778452918 ) ) ;
#13370 = CARTESIAN_POINT ( 'NONE',  ( -14.23620588414828880, -8.577105282884037507, 70.72957618505992627 ) ) ;
#13371 = ADVANCED_FACE ( 'NONE', ( #31724 ), #39350, .F. ) ;
#13372 = DIRECTION ( 'NONE',  ( 1.000000000000000000, 0.000000000000000000, 0.000000000000000000 ) ) ;
#13373 = EDGE_LOOP ( 'NONE', ( #14681, #37541 ) ) ;
#13374 = AXIS2_PLACEMENT_3D ( 'NONE', #36626, #14448, #26548 ) ;
#13375 = CARTESIAN_POINT ( 'NONE',  ( -21.02145776008824996, -20.81426181449660717, 65.58453904424985126 ) ) ;
#13376 = CIRCLE ( 'NONE', #16515, 4.686499999999998778 ) ;
#13377 = CARTESIAN_POINT ( 'NONE',  ( -10.83683315258895519, -12.44108567723101899, 57.32857332099802505 ) ) ;
#13378 = EDGE_LOOP ( 'NONE', ( #39786, #2352, #47443, #8834 ) ) ;
#13379 = PLANE ( 'NONE',  #21799 ) ;
#13380 = CIRCLE ( 'NONE', #11827, 4.686499999999999666 ) ;
#13381 = CARTESIAN_POINT ( 'NONE',  ( -24.72409385541305582, -14.80920654474415699, 62.92941176470587550 ) ) ;
#13382 = ORIENTED_EDGE ( 'NONE', *, *, #240, .F. ) ;
#13383 = DIRECTION ( 'NONE',  ( 1.224646799147353207E-16, 1.000000000000000000, -1.912410701131276611E-32 ) ) ;
#13384 = CARTESIAN_POINT ( 'NONE',  ( -10.00731240618708462, -14.10555136595099945, 61.10316694600977172 ) ) ;
#13385 = EDGE_LOOP ( 'NONE', ( #6247, #22303, #12779, #25597 ) ) ;
#13386 = CARTESIAN_POINT ( 'NONE',  ( -12.32158608955787393, -9.943909642237139579, 60.57390139315987909 ) ) ;
#13387 = CARTESIAN_POINT ( 'NONE',  ( 10.57590614458695377, 3.140741878271521514, 50.53406581128081143 ) ) ;
#13388 = EDGE_CURVE ( 'NONE', #47374, #27443, #4477, .T. ) ;
#13389 = AXIS2_PLACEMENT_3D ( 'NONE', #37272, #22783, #12170 ) ;
#13390 = CARTESIAN_POINT ( 'NONE',  ( -14.99706828511980916, -21.85287925006270626, 65.29092110561946072 ) ) ;
#13391 = ORIENTED_EDGE ( 'NONE', *, *, #37268, .T. ) ;
#13392 = CARTESIAN_POINT ( 'NONE',  ( -22.28468842640967651, -19.91619389767071269, 65.98949666203347419 ) ) ;
#13393 = CARTESIAN_POINT ( 'NONE',  ( -11.22844613476422282, -11.44458948612160221, 64.43409918096024569 ) ) ;
#13394 = CARTESIAN_POINT ( 'NONE',  ( -21.52726260838264949, -9.076274878514672295, 70.13132538915753855 ) ) ;
#13395 = CARTESIAN_POINT ( 'NONE',  ( -24.84449963183508459, -13.71944596863515464, 54.27966884056654351 ) ) ;
#13396 = ITEM_DEFINED_TRANSFORMATION ( 'NONE', 'NONE', #2293,  #29031 ) ;
#13397 = CARTESIAN_POINT ( 'NONE',  ( -20.18792757799173287, -7.890760935853403879, 73.97742500291465717 ) ) ;
#13398 = DIRECTION ( 'NONE',  ( 2.403795750412638671E-06, 2.069898558110202305E-06, 0.9999999999949686913 ) ) ;
#13399 = CARTESIAN_POINT ( 'NONE',  ( -17.42409385541300182, -14.80920654474440745, 53.27966884056655061 ) ) ;
#13400 = PLANE ( 'NONE',  #36729 ) ;
#13401 = ORIENTED_EDGE ( 'NONE', *, *, #47941, .F. ) ;
#13402 = CARTESIAN_POINT ( 'NONE',  ( -13.87451016560426353, -8.259160067131549710, 74.29931037044663356 ) ) ;
#13403 =( BOUNDED_SURFACE ( )  B_SPLINE_SURFACE ( 3, 1, ( 
 ( #13825, #25421 ),
 ( #33023, #21720 ),
 ( #18749, #28866 ),
 ( #17764, #10881 ),
 ( #10412, #7206 ),
 ( #18252, #33260 ),
 ( #33502, #6473 ) ),
 .UNSPECIFIED., .T., .F., .F. ) 
 B_SPLINE_SURFACE_WITH_KNOTS ( ( 4, 3, 4 ),
 ( 2, 2 ),
 ( 0.000000000000000000, 0.5000000000000000000, 1.000000000000000000 ),
 ( 0.000000000000000000, 1.000000000000000000 ),
 .UNSPECIFIED. ) 
 GEOMETRIC_REPRESENTATION_ITEM ( )  RATIONAL_B_SPLINE_SURFACE ( (
 ( 1.000000000000000000, 1.000000000000000000),
 ( 0.3333333333333335369, 0.3333333333333330373),
 ( 0.3333333333333335369, 0.3333333333333330373),
 ( 1.000000000000000000, 1.000000000000000000),
 ( 0.3333333333333333703, 0.3333333333333333703),
 ( 0.3333333333333333703, 0.3333333333333333703),
 ( 1.000000000000000000, 1.000000000000000000) ) ) 
 REPRESENTATION_ITEM ( '' )  SURFACE ( )  );
#13404 = CARTESIAN_POINT ( 'NONE',  ( -14.22441497990486958, -8.081217732231424478, 67.44470516081543110 ) ) ;
#13405 = CARTESIAN_POINT ( 'NONE',  ( -24.72409385541305582, -14.80920654474416764, 63.03529411764704804 ) ) ;
#13406 = ORIENTED_EDGE ( 'NONE', *, *, #385, .T. ) ;
#13407 = CARTESIAN_POINT ( 'NONE',  ( -19.90583630033073703, -21.83377919204098205, 69.19128392610542733 ) ) ;
#13408 = AXIS2_PLACEMENT_3D ( 'NONE', #21329, #10484, #43988 ) ;
#13409 = ORIENTED_EDGE ( 'NONE', *, *, #16145, .F. ) ;
#13410 = ADVANCED_FACE ( 'NONE', ( #4905 ), #5988, .T. ) ;
#13411 = EDGE_CURVE ( 'NONE', #24967, #29446, #38262, .T. ) ;
#13412 = ORIENTED_EDGE ( 'NONE', *, *, #31188, .F. ) ;
#13413 = ORIENTED_EDGE ( 'NONE', *, *, #1877, .T. ) ;
#13415 = CARTESIAN_POINT ( 'NONE',  ( -18.75808540593367368, -7.479482988535800736, 70.54784884510475251 ) ) ;
#13414 = CIRCLE ( 'NONE', #46449, 1.999999999999999112 ) ;
#13416 = CARTESIAN_POINT ( 'NONE',  ( -23.17271708368352634, -18.80356169263502508, 65.82389479710441549 ) ) ;
#13417 = CARTESIAN_POINT ( 'NONE',  ( -10.99582121268164414, -11.91441617825094923, 74.70840195586961840 ) ) ;
#13418 = CARTESIAN_POINT ( 'NONE',  ( -24.72409385541305582, -14.90920654474421170, 67.95882352941174531 ) ) ;
#13419 = CIRCLE ( 'NONE', #23688, 0.4000000000000010214 ) ;
#13420 = ORIENTED_EDGE ( 'NONE', *, *, #18893, .T. ) ;
#13421 = VERTEX_POINT ( 'NONE', #8350 ) ;
#13422 = EDGE_CURVE ( 'NONE', #2461, #19324, #47950, .T. ) ;
#13423 = EDGE_CURVE ( 'NONE', #28434, #32331, #6589, .T. ) ;
#13424 = CARTESIAN_POINT ( 'NONE',  ( -18.78659385650551528, -9.302874398569244363, 51.68646062012417985 ) ) ;
#13425 = CARTESIAN_POINT ( 'NONE',  ( -20.54786284059405688, -21.13826946137156781, 62.25904375309657723 ) ) ;
#13426 = VECTOR ( 'NONE', #7583, 1000.000000000000000 ) ;
#13427 = CARTESIAN_POINT ( 'NONE',  ( -11.75774308769439180, -19.00384223356172697, 71.98685884781657762 ) ) ;
#13428 = CARTESIAN_POINT ( 'NONE',  ( -20.02409385650551599, -6.426201560718813433, 50.50509628382439331 ) ) ;
#13429 = B_SPLINE_CURVE_WITH_KNOTS ( 'NONE', 1,
 ( #18258, #11135 ),
 .UNSPECIFIED., .F., .F.,
 ( 2, 2 ),
 ( 0.000000000000000000, 1.000000000000000000 ),
 .UNSPECIFIED. ) ;
#13430 = VERTEX_POINT ( 'NONE', #36838 ) ;
#13431 = ADVANCED_FACE ( 'NONE', ( #32681 ), #16036, .T. ) ;
#13432 = DIRECTION ( 'NONE',  ( 0.8743548079231423520, 0.4852872034802500623, -5.778319183281911236E-08 ) ) ;
#13433 = AXIS2_PLACEMENT_3D ( 'NONE', #41822, #14948, #22361 ) ;
#13434 = CARTESIAN_POINT ( 'NONE',  ( -24.41553149706675896, -15.71832598455623398, 69.81835354388927328 ) ) ;
#13435 = ORIENTED_EDGE ( 'NONE', *, *, #1762, .F. ) ;
#13436 = CARTESIAN_POINT ( 'NONE',  ( -21.84079884060555088, -9.314189094968263305, 63.34153755726884327 ) ) ;
#13437 = CARTESIAN_POINT ( 'NONE',  ( -22.40388508455290761, -9.889599135513202910, 73.70834494508456203 ) ) ;
#13438 = CARTESIAN_POINT ( 'NONE',  ( -20.94465790601859467, -8.243431112063134947, 59.95629843672877257 ) ) ;
#13439 = CARTESIAN_POINT ( 'NONE',  ( -22.48430662296557614, -20.27711519517875516, 65.81926411519917508 ) ) ;
#13440 = AXIS2_PLACEMENT_3D ( 'NONE', #36110, #13458, #25295 ) ;
#13441 = ORIENTED_EDGE ( 'NONE', *, *, #33523, .T. ) ;
#13442 = CARTESIAN_POINT ( 'NONE',  ( -20.48780003469585154, -11.24700778661463829, 49.52966884056655772 ) ) ;
#13443 =( BOUNDED_SURFACE ( )  B_SPLINE_SURFACE ( 3, 1, ( 
 ( #13944, #29481 ),
 ( #28995, #22099 ),
 ( #10294, #21613 ),
 ( #7340, #32911 ),
 ( #44765, #36600 ),
 ( #34375, #11994 ),
 ( #41793, #26772 ) ),
 .UNSPECIFIED., .T., .F., .F. ) 
 B_SPLINE_SURFACE_WITH_KNOTS ( ( 4, 3, 4 ),
 ( 2, 2 ),
 ( 0.000000000000000000, 0.5000000000000000000, 1.000000000000000000 ),
 ( 0.000000000000000000, 1.000000000000000000 ),
 .UNSPECIFIED. ) 
 GEOMETRIC_REPRESENTATION_ITEM ( )  RATIONAL_B_SPLINE_SURFACE ( (
 ( 1.000000000000000000, 1.000000000000000000),
 ( 0.3333333333333335369, 0.3333333333333330373),
 ( 0.3333333333333335369, 0.3333333333333330373),
 ( 1.000000000000000000, 1.000000000000000000),
 ( 0.3333333333333333703, 0.3333333333333333703),
 ( 0.3333333333333333703, 0.3333333333333333703),
 ( 1.000000000000000000, 1.000000000000000000) ) ) 
 REPRESENTATION_ITEM ( '' )  SURFACE ( )  );
#13444 = CARTESIAN_POINT ( 'NONE',  ( -23.03380641475053281, -9.905658051014942345, 66.65526928932193584 ) ) ;
#13445 = CARTESIAN_POINT ( 'NONE',  ( -21.05063378830672249, -20.85509781831549958, 65.87894135078376223 ) ) ;
#13446 = ORIENTED_EDGE ( 'NONE', *, *, #29445, .T. ) ;
#13447 = CARTESIAN_POINT ( 'NONE',  ( -21.92090081525502399, -20.24368645090660124, 62.53439249721748183 ) ) ;
#13448 = AXIS2_PLACEMENT_3D ( 'NONE', #16041, #12127, #4491 ) ;
#13449 = ORIENTED_EDGE ( 'NONE', *, *, #30160, .T. ) ;
#13450 = CARTESIAN_POINT ( 'NONE',  ( -13.43921731646364925, -8.993429882417945720, 60.43950277494440826 ) ) ;
#13451 = CARTESIAN_POINT ( 'NONE',  ( -9.975093131592752016, -14.93635113986534257, 74.98274190467411415 ) ) ;
#13452 = ORIENTED_EDGE ( 'NONE', *, *, #8261, .F. ) ;
#13453 = CARTESIAN_POINT ( 'NONE',  ( -46.29409385541305966, -12.91120565595568692, 71.69928697514914973 ) ) ;
#13454 = PLANE ( 'NONE',  #22403 ) ;
#13455 = CARTESIAN_POINT ( 'NONE',  ( -16.94618458872839994, -7.374472604449730184, 74.00372349603880195 ) ) ;
#13456 = CARTESIAN_POINT ( 'NONE',  ( -22.68242755436546076, -10.18794509063480547, 70.02795139357954213 ) ) ;
#13457 = EDGE_LOOP ( 'NONE', ( #16756, #31938, #35524, #11626 ) ) ;
#13458 = DIRECTION ( 'NONE',  ( 0.8547111024021492032, 0.5191039697695417621, 7.472447835916433805E-08 ) ) ;
#13459 = AXIS2_PLACEMENT_3D ( 'NONE', #39120, #8863, #38641 ) ;
#13460 = UNCERTAINTY_MEASURE_WITH_UNIT (LENGTH_MEASURE( 1.000000000000000082E-05 ), #5412, 'distance_accuracy_value', 'NONE');
#13461 = CARTESIAN_POINT ( 'NONE',  ( -24.17966087195022595, -11.66819065304315117, 59.52589827039258097 ) ) ;
#13462 = CARTESIAN_POINT ( 'NONE',  ( -10.10502314809590274, -16.20379097455708006, 68.09112436593052564 ) ) ;
#13463 = VERTEX_POINT ( 'NONE', #28518 ) ;
#13464 = LINE ( 'NONE', #25527, #26310 ) ;
#13465 =( BOUNDED_SURFACE ( )  B_SPLINE_SURFACE ( 3, 1, ( 
 ( #48339, #17803 ),
 ( #47628, #37239 ),
 ( #18047, #43952 ),
 ( #40711, #21762 ),
 ( #22005, #21290 ),
 ( #7246, #3523 ),
 ( #26192, #22249 ) ),
 .UNSPECIFIED., .T., .F., .F. ) 
 B_SPLINE_SURFACE_WITH_KNOTS ( ( 4, 3, 4 ),
 ( 2, 2 ),
 ( 0.000000000000000000, 0.5000000000000000000, 1.000000000000000000 ),
 ( 0.000000000000000000, 1.000000000000000000 ),
 .UNSPECIFIED. ) 
 GEOMETRIC_REPRESENTATION_ITEM ( )  RATIONAL_B_SPLINE_SURFACE ( (
 ( 1.000000000000000000, 1.000000000000000000),
 ( 0.3333333333333335369, 0.3333333333333330373),
 ( 0.3333333333333335369, 0.3333333333333330373),
 ( 1.000000000000000000, 1.000000000000000000),
 ( 0.3333333333333333703, 0.3333333333333333703),
 ( 0.3333333333333333703, 0.3333333333333333703),
 ( 1.000000000000000000, 1.000000000000000000) ) ) 
 REPRESENTATION_ITEM ( '' )  SURFACE ( )  );
#13466 = CARTESIAN_POINT ( 'NONE',  ( -12.04811195874215812, -10.23604714248314629, 60.71485379904431312 ) ) ;
#13467 = EDGE_CURVE ( 'NONE', #5874, #37436, #8026, .T. ) ;
#13468 = ORIENTED_EDGE ( 'NONE', *, *, #1349, .T. ) ;
#13469 = ORIENTED_EDGE ( 'NONE', *, *, #40896, .F. ) ;
#13470 = CARTESIAN_POINT ( 'NONE',  ( -14.25466281091639686, -21.11075775427102030, 71.92607504337564706 ) ) ;
#13471 = CARTESIAN_POINT ( 'NONE',  ( -10.83536383905390998, -17.31742040078651357, 64.62739380450889826 ) ) ;
#13472 = CARTESIAN_POINT ( 'NONE',  ( -13.12744695462171407, -20.89546087334666069, 58.30296024829184631 ) ) ;
#13473 = CARTESIAN_POINT ( 'NONE',  ( -17.12409385650551741, -6.426201560718813433, 50.50509628382439331 ) ) ;
#13474 = DIRECTION ( 'NONE',  ( 0.9687793358424822143, -0.2479245821708672415, 0.000000000000000000 ) ) ;
#13475 = CARTESIAN_POINT ( 'NONE',  ( -12.62463572719220828, -19.97835019563962788, 72.10653721712196784 ) ) ;
#13476 = CARTESIAN_POINT ( 'NONE',  ( -12.34924355347848035, -19.63124190001923708, 61.68062031358459052 ) ) ;
#13477 = CARTESIAN_POINT ( 'NONE',  ( -12.80135276601915528, -20.13603490024450693, 68.22168825917964341 ) ) ;
#13478 = CARTESIAN_POINT ( 'NONE',  ( -16.69790031487229243, -22.22389832459700898, 68.83527298580068532 ) ) ;
#13479 = ORIENTED_EDGE ( 'NONE', *, *, #21839, .F. ) ;
#13480 = ORIENTED_EDGE ( 'NONE', *, *, #23328, .F. ) ;
#13481 = EDGE_CURVE ( 'NONE', #15587, #41843, #21086, .T. ) ;
#13483 = CARTESIAN_POINT ( 'NONE',  ( -24.82475139314513868, -15.66597149415626156, 73.11808456017074320 ) ) ;
#13482 = COLOUR_RGB ( '', 0.09019608, 0.27058824, 0.51372549) ;
#13484 = EDGE_CURVE ( 'NONE', #20349, #30644, #14662, .T. ) ;
#13485 = TOROIDAL_SURFACE ( 'NONE', #41810, 2.260000000000000675, 0.2399999999999998246 ) ;
#13486 = CARTESIAN_POINT ( 'NONE',  ( -17.42409385541299471, -14.80920654474435594, 52.02966884056656482 ) ) ;
#13487 = DIRECTION ( 'NONE',  ( -0.000000000000000000, -1.000000000000000000, -0.000000000000000000 ) ) ;
#13488 = CARTESIAN_POINT ( 'NONE',  ( -13.77528250856571645, -8.773395728905704516, 57.38456636527085664 ) ) ;
#13489 = CARTESIAN_POINT ( 'NONE',  ( -20.88128654865952427, -21.40856141908871635, 58.68829242887799325 ) ) ;
#13490 = EDGE_CURVE ( 'NONE', #1995, #1905, #23273, .T. ) ;
#13491 = CARTESIAN_POINT ( 'NONE',  ( -21.84909385650551528, -8.104110260919577868, 48.81699501597546487 ) ) ;
#13492 = ORIENTED_EDGE ( 'NONE', *, *, #43620, .F. ) ;
#13493 = CARTESIAN_POINT ( 'NONE',  ( -18.11396434131172128, -21.77512919714542150, 65.34532159443909904 ) ) ;
#13494 = DIRECTION ( 'NONE',  ( 4.267285103686815209E-17, -5.292884291094200710E-16, -1.000000000000000000 ) ) ;
#13495 = CYLINDRICAL_SURFACE ( 'NONE', #31581, 2.000000000000000000 ) ;
#13496 = CARTESIAN_POINT ( 'NONE',  ( -10.06841751317020872, -15.99566775706410482, 68.16423218926057359 ) ) ;
#13497 = VECTOR ( 'NONE', #2782, 1000.000000000000000 ) ;
#13498 = ORIENTED_EDGE ( 'NONE', *, *, #9521, .T. ) ;
#13499 = DIRECTION ( 'NONE',  ( -1.000000000000000000, -0.000000000000000000, -0.000000000000000000 ) ) ;
#13500 = CARTESIAN_POINT ( 'NONE',  ( -33.42409385541304800, -8.109206544743658540, 50.50000000000030553 ) ) ;
#13501 = CARTESIAN_POINT ( 'NONE',  ( -10.71342319306032564, -12.63657128681412800, 57.53677342537894646 ) ) ;
#13502 = CARTESIAN_POINT ( 'NONE',  ( -21.82233664355339542, -16.46178511230714037, 52.02966884056656482 ) ) ;
#13503 = CARTESIAN_POINT ( 'NONE',  ( -14.85912063279003092, -7.814622674645058886, 56.95725833468153354 ) ) ;
#13504 = DIRECTION ( 'NONE',  ( -0.1206048672277665601, 0.4306442452895119510, 0.8944271909999156334 ) ) ;
#13505 = VERTEX_POINT ( 'NONE', #17882 ) ;
#13506 = CARTESIAN_POINT ( 'NONE',  ( -20.95199127080493895, -20.85531950328408612, 65.58453983063536441 ) ) ;
#13507 = ORIENTED_EDGE ( 'NONE', *, *, #40077, .T. ) ;
#13508 = CARTESIAN_POINT ( 'NONE',  ( -20.92409385541305511, -10.10920654474410618, 81.99999999999998579 ) ) ;
#13509 = CARTESIAN_POINT ( 'NONE',  ( -11.29876324976417123, -19.04990965798615221, 68.41027957156066464 ) ) ;
#13510 = ORIENTED_EDGE ( 'NONE', *, *, #36767, .T. ) ;
#13511 = CARTESIAN_POINT ( 'NONE',  ( -18.50162202296811742, -21.72577595440482057, 72.28510940981611554 ) ) ;
#13512 = CARTESIAN_POINT ( 'NONE',  ( -12.56051219783612538, -20.45271961000943861, 71.85007761110178137 ) ) ;
#13513 = AXIS2_PLACEMENT_3D ( 'NONE', #40930, #48080, #44893 ) ;
#13514 = EDGE_LOOP ( 'NONE', ( #37887, #37625, #4423, #19913 ) ) ;
#13515 = DIRECTION ( 'NONE',  ( 0.9997277805376393323, -0.02333162706040292980, -9.101776391673710038E-09 ) ) ;
#13516 = EDGE_CURVE ( 'NONE', #11148, #47795, #9144, .T. ) ;
#13517 = CARTESIAN_POINT ( 'NONE',  ( -24.47654139670598994, -14.67568567259567303, 66.48292734092783007 ) ) ;
#13518 = CARTESIAN_POINT ( 'NONE',  ( -16.29760782986628342, -22.17363506107604110, 61.87072849596245305 ) ) ;
#13519 = ORIENTED_EDGE ( 'NONE', *, *, #33107, .T. ) ;
#13520 = CARTESIAN_POINT ( 'NONE',  ( -17.42409385541299471, -14.80920654474435771, 49.52966884056655772 ) ) ;
#13521 = LINE ( 'NONE', #4118, #39275 ) ;
#13522 = CARTESIAN_POINT ( 'NONE',  ( -23.29871437377730814, -10.22635856038569990, 59.71548043103533843 ) ) ;
#13523 = ORIENTED_EDGE ( 'NONE', *, *, #16755, .T. ) ;
#13524 = ORIENTED_EDGE ( 'NONE', *, *, #25240, .T. ) ;
#13525 = FACE_OUTER_BOUND ( 'NONE', #1363, .T. ) ;
#13526 = LINE ( 'NONE', #20204, #32088 ) ;
#13527 = VERTEX_POINT ( 'NONE', #6345 ) ;
#13528 = CYLINDRICAL_SURFACE ( 'NONE', #21769, 0.1500000000000057399 ) ;
#13529 = CARTESIAN_POINT ( 'NONE',  ( -19.27094073640459015, -21.56284686256307381, 62.18430764133905342 ) ) ;
#13530 = CARTESIAN_POINT ( 'NONE',  ( -19.51784385759799179, -6.860780111191487229, 51.02154966934377001 ) ) ;
#13531 = LINE ( 'NONE', #28578, #1445 ) ;
#13532 = CARTESIAN_POINT ( 'NONE',  ( -24.25002676646741051, -16.58726329047720327, 59.42332704469328064 ) ) ;
#13533 = CARTESIAN_POINT ( 'NONE',  ( -16.01003035779492834, -7.894338788008341545, 70.75422978485266867 ) ) ;
#13534 = ORIENTED_EDGE ( 'NONE', *, *, #17376, .F. ) ;
#13535 = CARTESIAN_POINT ( 'NONE',  ( -20.66848101912799862, -8.549761622307151754, 60.12653141481577990 ) ) ;
#13536 = CARTESIAN_POINT ( 'NONE',  ( -13.06519849244570430, -8.767408624477393886, 64.01672394663651744 ) ) ;
#13537 = EDGE_CURVE ( 'NONE', #30092, #32365, #18579, .T. ) ;
#13538 = B_SPLINE_CURVE_WITH_KNOTS ( 'NONE', 3,
 ( #11458, #26481, #30437, #23046, #7786, #41752, #19330, #37797, #34337, #45702 ),
 .UNSPECIFIED., .F., .F.,
 ( 4, 2, 2, 2, 4 ),
 ( 0.6272669072877815610, 0.7522669073072951740, 0.8772669073268086759, 1.002266907346322178, 1.127266907365835902 ),
 .UNSPECIFIED. ) ;
#13539 = PLANE ( 'NONE',  #41347 ) ;
#13540 = CARTESIAN_POINT ( 'NONE',  ( -10.48085350821551742, -13.91959267249018950, 57.44825035245948186 ) ) ;
#13541 = EDGE_CURVE ( 'NONE', #9944, #32131, #16172, .T. ) ;
#13542 = EDGE_LOOP ( 'NONE', ( #715, #30868, #4020, #20642, #33195 ) ) ;
#13543 = EDGE_CURVE ( 'NONE', #10107, #3267, #39092, .T. ) ;
#13544 = ORIENTED_EDGE ( 'NONE', *, *, #34007, .T. ) ;
#13545 = CARTESIAN_POINT ( 'NONE',  ( -17.92858306677455715, -7.769287621248931686, 63.69489771833700331 ) ) ;
#13546 = CARTESIAN_POINT ( 'NONE',  ( -22.53890663478593481, -10.03013475771905760, 70.08466598210137022 ) ) ;
#13547 = CARTESIAN_POINT ( 'NONE',  ( -10.01440787728688520, -14.03439562150409969, 61.03325889150411143 ) ) ;
#13548 = EDGE_CURVE ( 'NONE', #24671, #42423, #25308, .T. ) ;
#13549 = ORIENTED_EDGE ( 'NONE', *, *, #5782, .F. ) ;
#13550 = EDGE_CURVE ( 'NONE', #19851, #47529, #21843, .T. ) ;
#13551 = CARTESIAN_POINT ( 'NONE',  ( 25.57590614458706568, 1.890747609047893185, 50.53028072113869484 ) ) ;
#13552 = CARTESIAN_POINT ( 'NONE',  ( -36.42409385541304800, -6.859212275519750435, 50.50378509014258555 ) ) ;
#13553 = ORIENTED_EDGE ( 'NONE', *, *, #17654, .T. ) ;
#13554 = CARTESIAN_POINT ( 'NONE',  ( -11.29219319990544079, -18.28864530752396433, 57.82186711835544912 ) ) ;
#13555 = CARTESIAN_POINT ( 'NONE',  ( -24.46146587544552276, -14.38248120490118609, 66.46820668217904426 ) ) ;
#13556 = ORIENTED_EDGE ( 'NONE', *, *, #5463, .F. ) ;
#13557 = EDGE_LOOP ( 'NONE', ( #29413, #23710 ) ) ;
#13558 = CARTESIAN_POINT ( 'NONE',  ( -50.42609385541305755, -14.90920654474419038, 65.94705882352940307 ) ) ;
#13559 = EDGE_LOOP ( 'NONE', ( #2284, #40000 ) ) ;
#13560 = CARTESIAN_POINT ( 'NONE',  ( -24.87417961795293664, -14.80849281899037884, 59.42795564617806292 ) ) ;
#13561 = DIRECTION ( 'NONE',  ( 2.775557561562888984E-15, 0.000000000000000000, -1.000000000000000000 ) ) ;
#13562 = CARTESIAN_POINT ( 'NONE',  ( -10.41125311197691694, -14.08592688229884970, 60.91821313097471347 ) ) ;
#13563 = ORIENTED_EDGE ( 'NONE', *, *, #31060, .F. ) ;
#13564 = PLANE ( 'NONE',  #14387 ) ;
#13565 = CARTESIAN_POINT ( 'NONE',  ( -20.18028783932825476, -21.73079638842835948, 72.56512126044646038 ) ) ;
#13566 = CARTESIAN_POINT ( 'NONE',  ( -45.55409385541306477, -13.24559821555319239, 71.00222776205102093 ) ) ;
#13567 = ADVANCED_FACE ( 'NONE', ( #22330 ), #29720, .T. ) ;
#13568 = CARTESIAN_POINT ( 'NONE',  ( -20.01548349435434204, -21.36955285994420706, 69.14302430453618342 ) ) ;
#13569 = LINE ( 'NONE', #32066, #38647 ) ;
#13570 = CARTESIAN_POINT ( 'NONE',  ( -19.15858190565953123, -8.027436205280443104, 60.18766296741227961 ) ) ;
#13571 = ORIENTED_EDGE ( 'NONE', *, *, #6759, .T. ) ;
#13572 = CARTESIAN_POINT ( 'NONE',  ( -50.42609385541305755, -14.90920654474425433, 71.08235294117645253 ) ) ;
#13573 = CARTESIAN_POINT ( 'NONE',  ( -23.46260529264823802, -11.17067950781535579, 73.36193301757424479 ) ) ;
#13574 = CYLINDRICAL_SURFACE ( 'NONE', #18817, 0.1499999999999991618 ) ;
#13575 = DIRECTION ( 'NONE',  ( -1.184681380772507928E-05, -1.827615836447136132E-06, 0.9999999999281563579 ) ) ;
#13576 = CARTESIAN_POINT ( 'NONE',  ( -36.42409385541304800, -6.859212275519750435, 50.50378509014258555 ) ) ;
#13577 = DIRECTION ( 'NONE',  ( 0.2479245821708712660, 0.9687793358424811041, 0.000000000000000000 ) ) ;
#13578 = EDGE_LOOP ( 'NONE', ( #5932, #583, #11416, #17503 ) ) ;
#13579 = ORIENTED_EDGE ( 'NONE', *, *, #46154, .T. ) ;
#13580 = DIRECTION ( 'NONE',  ( -3.071710424422018668E-17, 6.404604876783312462E-16, 1.000000000000000000 ) ) ;
#13581 = CARTESIAN_POINT ( 'NONE',  ( -24.43827367352892210, -15.52193379869737377, 73.28831629023289906 ) ) ;
#13582 = ORIENTED_EDGE ( 'NONE', *, *, #20851, .F. ) ;
#13583 = CARTESIAN_POINT ( 'NONE',  ( -23.49605051889219709, -11.22618518380361152, 73.37665428612797314 ) ) ;
#13585 = CARTESIAN_POINT ( 'NONE',  ( -14.05371499411350023, -21.00138273984457982, 72.22607703579409133 ) ) ;
#13584 = CARTESIAN_POINT ( 'NONE',  ( -10.66160677810301038, -13.00123309306513697, 67.73832347541063825 ) ) ;
#13586 = DIRECTION ( 'NONE',  ( 3.413470714839332458E-33, -1.190614954331866791E-16, 1.000000000000000000 ) ) ;
#13587 = CARTESIAN_POINT ( 'NONE',  ( -11.82205746763155041, -9.897907871467767293, 64.07268414109491061 ) ) ;
#13588 = DIRECTION ( 'NONE',  ( -1.000000000000000000, 0.000000000000000000, 0.000000000000000000 ) ) ;
#13589 =( BOUNDED_SURFACE ( )  B_SPLINE_SURFACE ( 3, 1, ( 
 ( #12640, #26939 ),
 ( #27662, #5256 ),
 ( #42927, #23979 ),
 ( #9199, #34301 ),
 ( #24218, #25420 ),
 ( #35757, #9920 ),
 ( #2282, #28147 ) ),
 .UNSPECIFIED., .T., .F., .F. ) 
 B_SPLINE_SURFACE_WITH_KNOTS ( ( 4, 3, 4 ),
 ( 2, 2 ),
 ( 0.000000000000000000, 0.5000000000000000000, 1.000000000000000000 ),
 ( 0.000000000000000000, 1.000000000000000000 ),
 .UNSPECIFIED. ) 
 GEOMETRIC_REPRESENTATION_ITEM ( )  RATIONAL_B_SPLINE_SURFACE ( (
 ( 1.000000000000000000, 1.000000000000000000),
 ( 0.3333333333333335369, 0.3333333333333330373),
 ( 0.3333333333333335369, 0.3333333333333330373),
 ( 1.000000000000000000, 1.000000000000000000),
 ( 0.3333333333333333703, 0.3333333333333333703),
 ( 0.3333333333333333703, 0.3333333333333333703),
 ( 1.000000000000000000, 1.000000000000000000) ) ) 
 REPRESENTATION_ITEM ( '' )  SURFACE ( )  );
#13590 = ORIENTED_EDGE ( 'NONE', *, *, #1774, .T. ) ;
#13591 = EDGE_CURVE ( 'NONE', #27994, #41987, #37496, .T. ) ;
#13592 = CARTESIAN_POINT ( 'NONE',  ( -45.37196614242555626, -14.20920654474410760, 70.43449436244726769 ) ) ;
#13593 = DIRECTION ( 'NONE',  ( 0.000000000000000000, 0.000000000000000000, 1.000000000000000000 ) ) ;
#13594 = CARTESIAN_POINT ( 'NONE',  ( -14.87342360121920315, -7.809316307502902177, 56.97283086062095236 ) ) ;
#13595 = ORIENTED_EDGE ( 'NONE', *, *, #26603, .F. ) ;
#13596 = DIRECTION ( 'NONE',  ( -0.6607190350374009258, -0.7506333037770478445, 0.000000000000000000 ) ) ;
#13597 = CARTESIAN_POINT ( 'NONE',  ( -13.24891125353284949, -8.638936510823443271, 60.56233416867657127 ) ) ;
#13598 = CARTESIAN_POINT ( 'NONE',  ( -22.91296630721855720, -15.15889098507616950, 54.07175714974879099 ) ) ;
#13599 = PLANE ( 'NONE',  #43292 ) ;
#13600 =( BOUNDED_CURVE ( )  B_SPLINE_CURVE ( 3, ( #7676, #38408, #45106, #37933 ),
 .UNSPECIFIED., .F., .F. ) 
 B_SPLINE_CURVE_WITH_KNOTS ( ( 4, 4 ),
 ( 0.9074455897393690629, 1.000000000000000000 ),
 .UNSPECIFIED. ) 
 CURVE ( )  GEOMETRIC_REPRESENTATION_ITEM ( )  RATIONAL_B_SPLINE_CURVE ( ( 0.6983129098261066092, 0.7760317562607099706, 0.8765941196520077305, 1.000000000000000000 ) ) 
 REPRESENTATION_ITEM ( '' )  );
#13601 = DIRECTION ( 'NONE',  ( 7.652304183832323392E-06, 2.165757503891338892E-06, 0.9999999999683758523 ) ) ;
#13602 =( BOUNDED_CURVE ( )  B_SPLINE_CURVE ( 3, ( #7018, #48132, #6772, #37269 ),
 .UNSPECIFIED., .F., .F. ) 
 B_SPLINE_CURVE_WITH_KNOTS ( ( 4, 4 ),
 ( 1.570796326794896780, 1.780235837034217505 ),
 .UNSPECIFIED. ) 
 CURVE ( )  GEOMETRIC_REPRESENTATION_ITEM ( )  RATIONAL_B_SPLINE_CURVE ( ( 1.000000000000000000, 0.9963479302455154896, 0.9963479302455154896, 1.000000000000000000 ) ) 
 REPRESENTATION_ITEM ( '' )  );
#13603 = ORIENTED_EDGE ( 'NONE', *, *, #25441, .T. ) ;
#13604 = ORIENTED_EDGE ( 'NONE', *, *, #18660, .T. ) ;
#13605 = CARTESIAN_POINT ( 'NONE',  ( -18.53034385541304374, -6.857644439848013640, 49.98602051094139398 ) ) ;
#13606 = EDGE_CURVE ( 'NONE', #3011, #32538, #13812, .T. ) ;
#13607 = DIRECTION ( 'NONE',  ( -0.5652317888644005084, -0.8249321334856241084, 7.911723905267715079E-08 ) ) ;
#13608 = VECTOR ( 'NONE', #4811, 1000.000000000000114 ) ;
#13609 = EDGE_CURVE ( 'NONE', #32577, #23164, #26120, .T. ) ;
#13610 = CARTESIAN_POINT ( 'NONE',  ( -24.03066126544255354, -17.12310022511010388, 69.48627920760770849 ) ) ;
#13611 = EDGE_CURVE ( 'NONE', #14012, #14322, #42648, .T. ) ;
#13612 =( BOUNDED_CURVE ( )  B_SPLINE_CURVE ( 3, ( #24016, #28433, #9724, #24742 ),
 .UNSPECIFIED., .F., .F. ) 
 B_SPLINE_CURVE_WITH_KNOTS ( ( 4, 4 ),
 ( 0.000000000000000000, 0.4074455897279072869 ),
 .UNSPECIFIED. ) 
 CURVE ( )  GEOMETRIC_REPRESENTATION_ITEM ( )  RATIONAL_B_SPLINE_CURVE ( ( 1.000000000000000000, 0.4567392136965981453, 0.3561768502956821347, 0.6983129097972519128 ) ) 
 REPRESENTATION_ITEM ( '' )  );
#13613 = B_SPLINE_CURVE_WITH_KNOTS ( 'NONE', 3,
 ( #7426, #25401, #37424, #18727, #25882, #32774, #14511, #40412, #6683, #48044 ),
 .UNSPECIFIED., .F., .F.,
 ( 4, 2, 2, 2, 4 ),
 ( 0.6272669072877967711, 0.7522669073073094959, 0.8772669073268222206, 1.002266907346335056, 1.127266907365847670 ),
 .UNSPECIFIED. ) ;
#13614 = CARTESIAN_POINT ( 'NONE',  ( -15.87557863975121464, -7.931372594209567417, 67.14007279017359053 ) ) ;
#13615 = CARTESIAN_POINT ( 'NONE',  ( -24.43362379028604536, -14.05489247495133753, 73.12271507725591846 ) ) ;
#13616 = ORIENTED_EDGE ( 'NONE', *, *, #8345, .T. ) ;
#13617 = CARTESIAN_POINT ( 'NONE',  ( -13.18362795047878144, -8.683667697493742565, 60.62445659250467145 ) ) ;
#13618 = CARTESIAN_POINT ( 'NONE',  ( -12.41315146567208139, -9.850077947585075933, 57.08935532239182464 ) ) ;
#13619 = EDGE_LOOP ( 'NONE', ( #30892, #30914, #47739, #43239, #38796 ) ) ;
#13620 = DIRECTION ( 'NONE',  ( 6.816999858124113439E-06, 9.113320815582587851E-06, 0.9999999999352379154 ) ) ;
#13621 = ADVANCED_FACE ( 'NONE', ( #7570 ), #23079, .T. ) ;
#13622 = LINE ( 'NONE', #13381, #32979 ) ;
#13623 = ADVANCED_FACE ( 'NONE', ( #190 ), #41220, .T. ) ;
#13624 = VERTEX_POINT ( 'NONE', #30469 ) ;
#13625 = DIRECTION ( 'NONE',  ( -1.000000000000000000, 0.000000000000000000, 0.000000000000000000 ) ) ;
#13626 = CARTESIAN_POINT ( 'NONE',  ( -11.39216336840796373, -18.45920852072106300, 61.29182966166492719 ) ) ;
#13627 = ADVANCED_FACE ( 'NONE', ( #7080 ), #11492, .T. ) ;
#13629 = EDGE_CURVE ( 'NONE', #13641, #4739, #44117, .T. ) ;
#13628 = ORIENTED_EDGE ( 'NONE', *, *, #3961, .T. ) ;
#13630 = CARTESIAN_POINT ( 'NONE',  ( -13.92250310594754303, -20.92831230454754987, 68.75065321223313219 ) ) ;
#13631 = DIRECTION ( 'NONE',  ( 1.000000000000000000, -4.164305804376849788E-17, 1.614929280266638808E-16 ) ) ;
#13632 = CARTESIAN_POINT ( 'NONE',  ( -10.74628672884880132, -17.07053172313825939, 61.17215199736627795 ) ) ;
#13633 = CARTESIAN_POINT ( 'NONE',  ( -11.09396220476197037, -17.79742230095041577, 71.75821477588401365 ) ) ;
#13634 = ORIENTED_EDGE ( 'NONE', *, *, #5110, .F. ) ;
#13635 = CARTESIAN_POINT ( 'NONE',  ( -10.40277084706750621, -15.44444119821074679, 57.86792809062919218 ) ) ;
#13636 = CARTESIAN_POINT ( 'NONE',  ( -24.55871690389112061, -12.66422819002857558, 69.88747705124970366 ) ) ;
#13637 = CARTESIAN_POINT ( 'NONE',  ( -19.75993683595673289, -21.46115599289353781, 68.94042252247996316 ) ) ;
#13638 = CARTESIAN_POINT ( 'NONE',  ( -10.78271008354229465, -17.17492318853433986, 61.45183338995374811 ) ) ;
#13639 = DIRECTION ( 'NONE',  ( 1.000000000000000000, 0.000000000000000000, 0.000000000000000000 ) ) ;
#13640 = FACE_OUTER_BOUND ( 'NONE', #28559, .T. ) ;
#13641 = VERTEX_POINT ( 'NONE', #11010 ) ;
#13642 = CARTESIAN_POINT ( 'NONE',  ( -11.10300703817161327, -10.86615712478015539, 57.39398594787093089 ) ) ;
#13643 = CARTESIAN_POINT ( 'NONE',  ( -13.30358754779367025, -20.46953698742588301, 58.11820441233432177 ) ) ;
#13644 = VERTEX_POINT ( 'NONE', #48672 ) ;
#13645 = DIRECTION ( 'NONE',  ( 0.000000000000000000, 1.000000000000000000, -0.000000000000000000 ) ) ;
#13646 = ORIENTED_EDGE ( 'NONE', *, *, #5072, .F. ) ;
#13647 = EDGE_CURVE ( 'NONE', #19673, #8437, #34133, .T. ) ;
#13648 = ORIENTED_EDGE ( 'NONE', *, *, #23952, .T. ) ;
#13649 = ORIENTED_EDGE ( 'NONE', *, *, #24754, .F. ) ;
#13650 = FACE_OUTER_BOUND ( 'NONE', #12474, .T. ) ;
#13651 = CARTESIAN_POINT ( 'NONE',  ( -22.66727108289645543, -10.09628893573625064, 70.01178520457129650 ) ) ;
#13652 = B_SPLINE_CURVE_WITH_KNOTS ( 'NONE', 1,
 ( #33327, #26707 ),
 .UNSPECIFIED., .F., .F.,
 ( 2, 2 ),
 ( 0.000000000000000000, 1.000000000000000000 ),
 .UNSPECIFIED. ) ;
#13653 = DIRECTION ( 'NONE',  ( 1.000000000000000000, 2.866981220435666553E-17, 0.000000000000000000 ) ) ;
#13654 = ORIENTED_EDGE ( 'NONE', *, *, #2661, .T. ) ;
#13655 = ORIENTED_EDGE ( 'NONE', *, *, #2791, .T. ) ;
#13656 = CARTESIAN_POINT ( 'NONE',  ( -17.66159385650551528, -9.295667164867525756, 49.30633214617472504 ) ) ;
#13657 = EDGE_CURVE ( 'NONE', #16737, #11137, #17913, .T. ) ;
#13658 = EDGE_CURVE ( 'NONE', #20248, #44249, #8295, .T. ) ;
#13659 = DIRECTION ( 'NONE',  ( 0.000000000000000000, 0.000000000000000000, 1.000000000000000000 ) ) ;
#13660 = CARTESIAN_POINT ( 'NONE',  ( -18.11159385650551457, -6.922745924619793101, 51.69366785382590024 ) ) ;
#13661 = VECTOR ( 'NONE', #12928, 999.9999999999998863 ) ;
#13662 = ORIENTED_EDGE ( 'NONE', *, *, #34563, .F. ) ;
#13663 = FACE_OUTER_BOUND ( 'NONE', #21185, .T. ) ;
#13664 = VECTOR ( 'NONE', #25229, 1000.000000000000000 ) ;
#13665 = CARTESIAN_POINT ( 'NONE',  ( -50.42609385541305755, -14.80920654474428666, 74.09999999999998010 ) ) ;
#13666 = B_SPLINE_CURVE_WITH_KNOTS ( 'NONE', 3,
 ( #1080, #8241, #12648, #12883, #8472, #38988, #1311, #31614, #46392, #34560 ),
 .UNSPECIFIED., .F., .F.,
 ( 4, 2, 2, 2, 4 ),
 ( 0.1272669073657735350, 0.2522669073462773248, 0.3772669073267810314, 0.5022669073072848489, 0.6272669072877885554 ),
 .UNSPECIFIED. ) ;
#13667 = ORIENTED_EDGE ( 'NONE', *, *, #4646, .F. ) ;
#13668 = CARTESIAN_POINT ( 'NONE',  ( -12.41315160057549960, -9.850077812919039388, 57.23935532239169532 ) ) ;
#13669 = EDGE_CURVE ( 'NONE', #22665, #29528, #38299, .T. ) ;
#13670 = ORIENTED_EDGE ( 'NONE', *, *, #24110, .T. ) ;
#13671 = FACE_OUTER_BOUND ( 'NONE', #15137, .T. ) ;
#13672 = CYLINDRICAL_SURFACE ( 'NONE', #17104, 5.249999999999998224 ) ;
#13673 = EDGE_CURVE ( 'NONE', #30431, #14945, #35952, .T. ) ;
#13674 = ADVANCED_FACE ( 'NONE', ( #26999 ), #5711, .T. ) ;
#13675 = CARTESIAN_POINT ( 'NONE',  ( -19.24829632005326019, -7.991050106228435368, 67.04504941182814548 ) ) ;
#13676 = ORIENTED_EDGE ( 'NONE', *, *, #1937, .T. ) ;
#13677 = DIRECTION ( 'NONE',  ( 1.224646799147353207E-16, 1.000000000000000000, -1.912410701131276611E-32 ) ) ;
#13678 =( BOUNDED_SURFACE ( )  B_SPLINE_SURFACE ( 3, 1, ( 
 ( #15250, #30314 ),
 ( #19943, #46773 ),
 ( #43072, #4681 ),
 ( #30797, #19704 ),
 ( #12301, #12070 ),
 ( #28046, #12548 ),
 ( #38892, #19451 ) ),
 .UNSPECIFIED., .T., .F., .F. ) 
 B_SPLINE_SURFACE_WITH_KNOTS ( ( 4, 3, 4 ),
 ( 2, 2 ),
 ( 0.000000000000000000, 0.5000000000000000000, 1.000000000000000000 ),
 ( 0.000000000000000000, 1.000000000000000000 ),
 .UNSPECIFIED. ) 
 GEOMETRIC_REPRESENTATION_ITEM ( )  RATIONAL_B_SPLINE_SURFACE ( (
 ( 1.000000000000000000, 1.000000000000000000),
 ( 0.3333333333333335369, 0.3333333333333330373),
 ( 0.3333333333333335369, 0.3333333333333330373),
 ( 1.000000000000000000, 1.000000000000000000),
 ( 0.3333333333333333703, 0.3333333333333333703),
 ( 0.3333333333333333703, 0.3333333333333333703),
 ( 1.000000000000000000, 1.000000000000000000) ) ) 
 REPRESENTATION_ITEM ( '' )  SURFACE ( )  );
#13679 = DIRECTION ( 'NONE',  ( 0.000000000000000000, 0.9999954153791273948, 0.003028072113819836077 ) ) ;
#13680 = CARTESIAN_POINT ( 'NONE',  ( -10.44157451558128358, -15.80814149404359981, 68.06948097726898084 ) ) ;
#13681 = ORIENTED_EDGE ( 'NONE', *, *, #21011, .F. ) ;
#13682 = DIRECTION ( 'NONE',  ( -4.734277553319870270E-07, 1.363385191780837012E-06, 0.9999999999989586108 ) ) ;
#13683 = FACE_OUTER_BOUND ( 'NONE', #43141, .T. ) ;
#13684 = ORIENTED_EDGE ( 'NONE', *, *, #14822, .T. ) ;
#13685 = CARTESIAN_POINT ( 'NONE',  ( -15.03427660820159950, -21.44211488324610926, 65.12068745241758450 ) ) ;
#13686 = EDGE_CURVE ( 'NONE', #32298, #3630, #45739, .T. ) ;
#13687 = ADVANCED_FACE ( 'NONE', ( #16387 ), #12222, .T. ) ;
#13688 = CARTESIAN_POINT ( 'NONE',  ( -9.975950761882481643, -15.00625170120774321, 74.91123542948268721 ) ) ;
#13689 = B_SPLINE_CURVE_WITH_KNOTS ( 'NONE', 1,
 ( #42727, #13384 ),
 .UNSPECIFIED., .F., .F.,
 ( 2, 2 ),
 ( 0.000000000000000000, 1.000000000000000000 ),
 .UNSPECIFIED. ) ;
#13690 = VERTEX_POINT ( 'NONE', #39041 ) ;
#13691 = DIRECTION ( 'NONE',  ( 6.291559634385637730E-07, -1.530398238691524640E-06, 0.9999999999986310950 ) ) ;
#13692 = PLANE ( 'NONE',  #42835 ) ;
#13693 = CYLINDRICAL_SURFACE ( 'NONE', #6098, 1.249999999999998668 ) ;
#13694 = DIRECTION ( 'NONE',  ( 1.224646799147353207E-16, 1.000000000000000000, -1.912410701131276611E-32 ) ) ;
#13695 = EDGE_LOOP ( 'NONE', ( #42580, #24740 ) ) ;
#13696 = CARTESIAN_POINT ( 'NONE',  ( -12.82854046268865034, -13.89041861240101028, 52.02966884056656482 ) ) ;
#13697 = CARTESIAN_POINT ( 'NONE',  ( -19.04725004413522882, -7.538051835607980422, 67.07884570001746738 ) ) ;
#13698 = DIRECTION ( 'NONE',  ( -0.9345716196833626643, 0.3557750520798445559, 2.412542607589989711E-09 ) ) ;
#13699 = ORIENTED_EDGE ( 'NONE', *, *, #18088, .F. ) ;
#13700 = CARTESIAN_POINT ( 'NONE',  ( -23.97576963128622651, -17.42270779624378108, 62.47360993958987763 ) ) ;
#13701 = CIRCLE ( 'NONE', #34166, 2.000000000000000888 ) ;
#13702 = CARTESIAN_POINT ( 'NONE',  ( -24.25486363958986757, -13.06355980472538292, 63.11792038370487035 ) ) ;
#13703 = EDGE_CURVE ( 'NONE', #37795, #42591, #24170, .T. ) ;
#13704 = AXIS2_PLACEMENT_3D ( 'NONE', #17761, #26151, #45121 ) ;
#13705 = ORIENTED_EDGE ( 'NONE', *, *, #30019, .T. ) ;
#13706 = ORIENTED_EDGE ( 'NONE', *, *, #22841, .F. ) ;
#13707 = CARTESIAN_POINT ( 'NONE',  ( -46.48223616206310993, -14.19714313411900619, 70.52197034960447297 ) ) ;
#13708 = CARTESIAN_POINT ( 'NONE',  ( -15.55273166284925246, -8.063985742959628666, 70.71875758216351926 ) ) ;
#13709 = CARTESIAN_POINT ( 'NONE',  ( -10.02491569571532715, -15.67798101985274073, 61.23800248293585469 ) ) ;
#13710 = CARTESIAN_POINT ( 'NONE',  ( -23.42532328873747005, -19.22384396101403681, 62.46911485589509994 ) ) ;
#13711 = CARTESIAN_POINT ( 'NONE',  ( 18.46573386768564973, 3.114729847419841047, 50.78398819077492732 ) ) ;
#13712 = CARTESIAN_POINT ( 'NONE',  ( -11.33476867595667770, -19.10151316506851416, 68.40185013497388411 ) ) ;
#13713 = CARTESIAN_POINT ( 'NONE',  ( -13.03244867582903943, -9.358201799085602346, 67.48828719236378504 ) ) ;
#13714 = CARTESIAN_POINT ( 'NONE',  ( -16.71219879347879100, -22.22520166962337740, 68.81065243885818461 ) ) ;
#13715 = ORIENTED_EDGE ( 'NONE', *, *, #33182, .T. ) ;
#13716 = EDGE_LOOP ( 'NONE', ( #45980, #38731 ) ) ;
#13717 = CARTESIAN_POINT ( 'NONE',  ( -35.32409385541306079, -25.10920654474410441, 48.79999999999998295 ) ) ;
#13718 = CARTESIAN_POINT ( 'NONE',  ( -19.85066507975247063, -8.243252523173408619, 73.91199902895934315 ) ) ;
#13719 = CARTESIAN_POINT ( 'NONE',  ( -21.36489355414517632, -8.963473290115421932, 73.90128753234840531 ) ) ;
#13720 = CARTESIAN_POINT ( 'NONE',  ( -10.97672171568423671, -17.53854784295387503, 71.79547974970954272 ) ) ;
#13721 = DIRECTION ( 'NONE',  ( 3.549360974554993999E-17, -6.371834667797928663E-18, -1.000000000000000000 ) ) ;
#13722 = CARTESIAN_POINT ( 'NONE',  ( -19.71159385650551599, -6.922745924619793101, 51.69366785382590024 ) ) ;
#13723 = ORIENTED_EDGE ( 'NONE', *, *, #31158, .T. ) ;
#13724 = B_SPLINE_CURVE_WITH_KNOTS ( 'NONE', 3,
 ( #25434, #2296, #17779, #17303, #40445, #32353, #47372, #28648, #39971, #32807 ),
 .UNSPECIFIED., .F., .F.,
 ( 4, 2, 2, 2, 4 ),
 ( 0.000000000000000000, 0.2500000000000000000, 0.5000000000000000000, 0.7500000000000000000, 1.000000000000000000 ),
 .UNSPECIFIED. ) ;
#13725 = CARTESIAN_POINT ( 'NONE',  ( -12.66750632023469514, -20.01285372994693290, 68.63657439664891058 ) ) ;
#13726 = CARTESIAN_POINT ( 'NONE',  ( -14.42683419600288985, -8.428067575814651491, 67.55975083869262221 ) ) ;
#13727 = CARTESIAN_POINT ( 'NONE',  ( -11.17067368074822120, -18.85886670308036273, 64.88673749957456494 ) ) ;
#13728 =( BOUNDED_CURVE ( )  B_SPLINE_CURVE ( 3, ( #5895, #10555, #18167, #29020 ),
 .UNSPECIFIED., .F., .F. ) 
 B_SPLINE_CURVE_WITH_KNOTS ( ( 4, 4 ),
 ( 0.4074455897393691739, 0.5000000000000000000 ),
 .UNSPECIFIED. ) 
 CURVE ( )  GEOMETRIC_REPRESENTATION_ITEM ( )  RATIONAL_B_SPLINE_CURVE ( ( 0.6983129098260982826, 0.7760317562607088604, 0.8765941196520110612, 1.000000000000009548 ) ) 
 REPRESENTATION_ITEM ( '' )  );
#13729 = ORIENTED_EDGE ( 'NONE', *, *, #27618, .F. ) ;
#13730 = CARTESIAN_POINT ( 'NONE',  ( -10.59456938016190541, -16.34492539027162650, 71.52038324560433580 ) ) ;
#13731 = CARTESIAN_POINT ( 'NONE',  ( -12.73501256528857617, -9.611849834345010279, 74.42808954951277656 ) ) ;
#13732 = ADVANCED_FACE ( 'NONE', ( #4591 ), #22378, .T. ) ;
#13733 = VECTOR ( 'NONE', #12206, 1000.000000000000000 ) ;
#13734 = LINE ( 'NONE', #13971, #37525 ) ;
#13735 = CARTESIAN_POINT ( 'NONE',  ( -12.14425506381237341, -10.13739722748950811, 64.32914326607962607 ) ) ;
#13736 = ORIENTED_EDGE ( 'NONE', *, *, #9551, .T. ) ;
#13737 = DIRECTION ( 'NONE',  ( 0.9757441136919973168, 0.2189141945955502822, 0.000000000000000000 ) ) ;
#13738 =( BOUNDED_CURVE ( )  B_SPLINE_CURVE ( 3, ( #8137, #46534, #20167, #30546 ),
 .UNSPECIFIED., .F., .F. ) 
 B_SPLINE_CURVE_WITH_KNOTS ( ( 4, 4 ),
 ( 0.000000000000000000, 0.4074455897393669535 ),
 .UNSPECIFIED. ) 
 CURVE ( )  GEOMETRIC_REPRESENTATION_ITEM ( )  RATIONAL_B_SPLINE_CURVE ( ( 1.000000000000000000, 0.4567392136813293035, 0.3561768502900293232, 0.6983129098261000589 ) ) 
 REPRESENTATION_ITEM ( '' )  );
#13739 = ORIENTED_EDGE ( 'NONE', *, *, #27206, .F. ) ;
#13740 = FACE_OUTER_BOUND ( 'NONE', #37412, .T. ) ;
#13741 = EDGE_CURVE ( 'NONE', #12408, #47772, #4842, .T. ) ;
#13742 = EDGE_CURVE ( 'NONE', #29199, #31757, #5290, .T. ) ;
#13743 = CARTESIAN_POINT ( 'NONE',  ( -19.25584931519960463, -7.587732789139183254, 63.57055898488500389 ) ) ;
#13744 = VERTEX_POINT ( 'NONE', #9259 ) ;
#13745 = LINE ( 'NONE', #2680, #28131 ) ;
#13746 = EDGE_CURVE ( 'NONE', #10431, #32365, #42515, .T. ) ;
#13747 = CARTESIAN_POINT ( 'NONE',  ( -14.68034385650551599, -6.424090610841176385, 49.80797279389978627 ) ) ;
#13748 = VERTEX_POINT ( 'NONE', #5577 ) ;
#13749 = LINE ( 'NONE', #28792, #36225 ) ;
#13750 = EDGE_CURVE ( 'NONE', #27631, #14412, #42812, .T. ) ;
#13751 = CYLINDRICAL_SURFACE ( 'NONE', #10995, 2.500000000000002220 ) ;
#13752 = CARTESIAN_POINT ( 'NONE',  ( -20.10030204730919223, -21.76202525863913451, 72.51983304728076973 ) ) ;
#13753 = VERTEX_POINT ( 'NONE', #7455 ) ;
#13754 = CARTESIAN_POINT ( 'NONE',  ( -13.46024608985845994, -21.11736968229694611, 65.12595554403661424 ) ) ;
#13755 = CARTESIAN_POINT ( 'NONE',  ( -17.08147026401541524, -7.366339275741904835, 70.60380589010705421 ) ) ;
#13756 = CARTESIAN_POINT ( 'NONE',  ( 18.62590614458706995, 1.904976371434334181, 48.53033133619892681 ) ) ;
#13757 = CARTESIAN_POINT ( 'NONE',  ( -23.34189317711797429, -10.28335673940103590, 59.64557479084083269 ) ) ;
#13758 = EDGE_CURVE ( 'NONE', #13276, #22004, #47425, .T. ) ;
#13759 = VERTEX_POINT ( 'NONE', #43977 ) ;
#13760 = ORIENTED_EDGE ( 'NONE', *, *, #30299, .F. ) ;
#13761 = B_SPLINE_CURVE_WITH_KNOTS ( 'NONE', 3,
 ( #32787, #21714, #22206, #33016 ),
 .UNSPECIFIED., .F., .F.,
 ( 4, 4 ),
 ( 0.001310108020964423923, 0.002761379516307285557 ),
 .UNSPECIFIED. ) ;
#13762 = CARTESIAN_POINT ( 'NONE',  ( -23.81387519531508445, -18.64000541993103610, 72.88555444462819821 ) ) ;
#13763 = CARTESIAN_POINT ( 'NONE',  ( -24.23813412381375088, -12.99935709875259526, 66.31718868320673721 ) ) ;
#13764 = ORIENTED_EDGE ( 'NONE', *, *, #46869, .F. ) ;
#13765 = CARTESIAN_POINT ( 'NONE',  ( -20.73640204290083489, -8.136034802137729116, 63.51132713554439846 ) ) ;
#13766 = CARTESIAN_POINT ( 'NONE',  ( -19.96784385759798752, -9.357632978295830739, 49.97845033065684106 ) ) ;
#13767 = CARTESIAN_POINT ( 'NONE',  ( -23.59778322581706789, -11.38860327479983603, 63.10785482661193413 ) ) ;
#13768 = CARTESIAN_POINT ( 'NONE',  ( -13.76968405657925487, -21.30219918833402204, 72.11263056552699879 ) ) ;
#13769 = CARTESIAN_POINT ( 'NONE',  ( -12.41631181157024066, -9.915882637312337877, 60.66991079537774567 ) ) ;
#13770 = AXIS2_PLACEMENT_3D ( 'NONE', #32400, #47419, #20824 ) ;
#13771 = EDGE_LOOP ( 'NONE', ( #33078, #9023 ) ) ;
#13772 = FACE_OUTER_BOUND ( 'NONE', #17064, .T. ) ;
#13773 = VECTOR ( 'NONE', #5080, 1000.000000000000341 ) ;
#13774 = CARTESIAN_POINT ( 'NONE',  ( -19.24190786459753610, -7.584296138276666710, 63.54593947706258206 ) ) ;
#13775 = CARTESIAN_POINT ( 'NONE',  ( -24.47432067347917695, -14.77756146504815327, 59.52828185648635184 ) ) ;
#13776 = DIRECTION ( 'NONE',  ( -0.8507615431891570879, 0.5255518971808580408, 6.876821558984483597E-08 ) ) ;
#13777 = EDGE_LOOP ( 'NONE', ( #16716, #19045, #40274, #26511, #29823 ) ) ;
#13778 = ORIENTED_EDGE ( 'NONE', *, *, #28776, .T. ) ;
#13779 = CARTESIAN_POINT ( 'NONE',  ( -24.47999924015074669, -14.97998867148549351, 62.85729180369179403 ) ) ;
#13780 = CARTESIAN_POINT ( 'NONE',  ( -17.02409385541305653, -14.80920654474410725, 48.99999999999997868 ) ) ;
#13781 = ADVANCED_FACE ( 'NONE', ( #47892 ), #2149, .F. ) ;
#13782 = ORIENTED_EDGE ( 'NONE', *, *, #28710, .F. ) ;
#13783 = CARTESIAN_POINT ( 'NONE',  ( -22.02670722051955465, -15.75340237016373202, 49.52966884056655772 ) ) ;
#13784 = CARTESIAN_POINT ( 'NONE',  ( -23.75797280549784318, -17.78947120508452429, 59.30378417803890301 ) ) ;
#13785 = EDGE_CURVE ( 'NONE', #16929, #15929, #15746, .T. ) ;
#13786 = ORIENTED_EDGE ( 'NONE', *, *, #31263, .T. ) ;
#13787 = DIRECTION ( 'NONE',  ( 1.000000000000000000, -4.164305804376849172E-17, 1.614929280266638808E-16 ) ) ;
#13788 = CARTESIAN_POINT ( 'NONE',  ( -12.23220172533775063, -19.57856247689574403, 57.92682373937842044 ) ) ;
#13789 = CARTESIAN_POINT ( 'NONE',  ( -22.98865756656685022, -9.855479763439479512, 70.12683098403445570 ) ) ;
#13790 = ORIENTED_EDGE ( 'NONE', *, *, #25703, .T. ) ;
#13791 = DIRECTION ( 'NONE',  ( -0.4468359692653126602, 0.01837434545035235636, 0.8944271909999157444 ) ) ;
#13792 = AXIS2_PLACEMENT_3D ( 'NONE', #40382, #21673, #40865 ) ;
#13793 = ORIENTED_EDGE ( 'NONE', *, *, #26722, .F. ) ;
#13794 = CARTESIAN_POINT ( 'NONE',  ( -27.42409385541305511, -25.10920654474410441, 54.99999999999997868 ) ) ;
#13795 = DIRECTION ( 'NONE',  ( 0.9687793358424821033, -0.2479245821708677133, 0.000000000000000000 ) ) ;
#13796 = DIRECTION ( 'NONE',  ( -1.006957036272130273E-05, 6.253991260048532259E-06, 0.9999999999297456421 ) ) ;
#13797 = ORIENTED_EDGE ( 'NONE', *, *, #25302, .T. ) ;
#13798 = LINE ( 'NONE', #48276, #21515 ) ;
#13799 = DIRECTION ( 'NONE',  ( 0.5589780652556124441, -0.8291824422665291516, 7.938832475108296738E-08 ) ) ;
#13800 = EDGE_CURVE ( 'NONE', #19337, #44272, #35587, .T. ) ;
#13801 = CARTESIAN_POINT ( 'NONE',  ( -23.17409385650551457, -9.792211528768504536, 50.49490371617623197 ) ) ;
#13802 = EDGE_CURVE ( 'NONE', #44542, #43576, #7588, .T. ) ;
#13803 = CARTESIAN_POINT ( 'NONE',  ( -14.57821615407322291, -8.355182602927943236, 60.52816311995014331 ) ) ;
#13804 = CARTESIAN_POINT ( 'NONE',  ( 18.07590614458695200, 0.7915096701590282890, 50.27695098796855433 ) ) ;
#13805 = CARTESIAN_POINT ( 'NONE',  ( -19.14472750395669465, -8.023971105352707411, 60.06978972629352853 ) ) ;
#13806 = ORIENTED_EDGE ( 'NONE', *, *, #15123, .F. ) ;
#13807 = CARTESIAN_POINT ( 'NONE',  ( 25.57590614458706568, 1.876874565721113663, 52.48023137145496264 ) ) ;
#13808 = CARTESIAN_POINT ( 'NONE',  ( -24.67073143307269589, -13.07968201635391914, 62.97230848449754603 ) ) ;
#13809 = CARTESIAN_POINT ( 'NONE',  ( -22.69143476767070311, -20.07792998486722880, 69.29605258592428640 ) ) ;
#13810 = CARTESIAN_POINT ( 'NONE',  ( -13.35818949714929360, -21.05197827947291955, 61.70141596610112344 ) ) ;
#13811 = EDGE_CURVE ( 'NONE', #47972, #19236, #30888, .T. ) ;
#13812 = B_SPLINE_CURVE_WITH_KNOTS ( 'NONE', 1,
 ( #37573, #33896 ),
 .UNSPECIFIED., .F., .F.,
 ( 2, 2 ),
 ( 0.000000000000000000, 1.000000000000000000 ),
 .UNSPECIFIED. ) ;
#13813 = CARTESIAN_POINT ( 'NONE',  ( -10.81980138738203223, -12.48416433311569129, 60.98780598612082571 ) ) ;
#13814 = CARTESIAN_POINT ( 'NONE',  ( -13.46784385650551741, -6.428312510596451368, 51.20221977374900035 ) ) ;
#13815 = ORIENTED_EDGE ( 'NONE', *, *, #6199, .T. ) ;
#13816 = EDGE_LOOP ( 'NONE', ( #16952, #13917 ) ) ;
#13817 = CARTESIAN_POINT ( 'NONE',  ( -21.63336539757928634, -9.153348366551478321, 66.94677872351418557 ) ) ;
#13818 = CARTESIAN_POINT ( 'NONE',  ( -24.84033948030421968, -15.52542097194404569, 73.11648385888869939 ) ) ;
#13819 = ORIENTED_EDGE ( 'NONE', *, *, #33522, .F. ) ;
#13820 = CARTESIAN_POINT ( 'NONE',  ( -15.49415775405465645, -8.028509947901662613, 74.37985659017797957 ) ) ;
#13822 = CARTESIAN_POINT ( 'NONE',  ( -12.66943518016813996, -20.01945279446396952, 65.07494931179483899 ) ) ;
#13821 = CARTESIAN_POINT ( 'NONE',  ( -17.65006842549283306, -20.30456235612523841, 53.49899999999994549 ) ) ;
#13823 = CARTESIAN_POINT ( 'NONE',  ( -14.58890586778976584, -8.408938977662566927, 63.78978847347087111 ) ) ;
#13824 = CARTESIAN_POINT ( 'NONE',  ( -19.62595585458452163, -8.103479577873935469, 60.10526007146324901 ) ) ;
#13825 = CARTESIAN_POINT ( 'NONE',  ( -21.94242186726961208, -9.397052521110282441, 60.00699132926281010 ) ) ;
#13826 = ADVANCED_FACE ( 'NONE', ( #13650 ), #2821, .F. ) ;
#13827 = DIRECTION ( 'NONE',  ( 0.4439273849576848563, 0.8960627639203804229, 1.004702157337987228E-17 ) ) ;
#13828 = FACE_OUTER_BOUND ( 'NONE', #25677, .T. ) ;
#13829 = CARTESIAN_POINT ( 'NONE',  ( -46.47622156840087371, -14.20920654474410760, 70.13000000000000966 ) ) ;
#13830 = CARTESIAN_POINT ( 'NONE',  ( -11.46167752593530942, -19.27618730729482266, 71.80873093914522087 ) ) ;
#13831 = CARTESIAN_POINT ( 'NONE',  ( -20.95545100651803594, -20.91135505560678354, 65.59926067308570907 ) ) ;
#13832 = EDGE_LOOP ( 'NONE', ( #3639, #15910, #11007, #17724, #29496 ) ) ;
#13833 = DIRECTION ( 'NONE',  ( 0.8394943004421988597, -0.3114503813636535501, 0.4452504682462422592 ) ) ;
#13834 = CARTESIAN_POINT ( 'NONE',  ( -11.54077142481382268, -18.60227312804761723, 61.34998797001519932 ) ) ;
#13835 = CARTESIAN_POINT ( 'NONE',  ( -10.40127070788197017, -12.32249518151173895, 57.51352764219546998 ) ) ;
#13836 = CARTESIAN_POINT ( 'NONE',  ( -24.18037300165767434, -17.94870813986570113, 59.18873840842728384 ) ) ;
#13837 = CARTESIAN_POINT ( 'NONE',  ( -10.73343087151675590, -11.53221169192942597, 71.34506790255136366 ) ) ;
#13838 = ORIENTED_EDGE ( 'NONE', *, *, #31669, .F. ) ;
#13839 = AXIS2_PLACEMENT_3D ( 'NONE', #1158, #31203, #5108 ) ;
#13840 = EDGE_LOOP ( 'NONE', ( #44469, #30409, #18958, #1110, #34509, #24882 ) ) ;
#13841 = AXIS2_PLACEMENT_3D ( 'NONE', #14798, #19996, #23212 ) ;
#13842 = CARTESIAN_POINT ( 'NONE',  ( -19.03659385541304516, -8.995762431863214559, 51.38120296130585274 ) ) ;
#13843 = CARTESIAN_POINT ( 'NONE',  ( -24.01131036459814183, -17.17762702439318900, 69.42842272742100818 ) ) ;
#13844 = EDGE_CURVE ( 'NONE', #39405, #44032, #46165, .T. ) ;
#13845 = B_SPLINE_CURVE_WITH_KNOTS ( 'NONE', 1,
 ( #11324, #27067 ),
 .UNSPECIFIED., .F., .F.,
 ( 2, 2 ),
 ( 0.000000000000000000, 1.000000000000000000 ),
 .UNSPECIFIED. ) ;
#13846 = CARTESIAN_POINT ( 'NONE',  ( -24.61986767591916347, -12.87896034533829237, 66.44213403754470448 ) ) ;
#13847 = CARTESIAN_POINT ( 'NONE',  ( -15.99552465959851233, -21.71601670177824417, 58.70074462513652236 ) ) ;
#13848 = ORIENTED_EDGE ( 'NONE', *, *, #47434, .F. ) ;
#13849 = CARTESIAN_POINT ( 'NONE',  ( -11.00778200170179133, -11.02323315455921815, 60.77862143039379106 ) ) ;
#13850 = CARTESIAN_POINT ( 'NONE',  ( -21.13453391143521287, -20.81317186429504673, 62.27038425631170782 ) ) ;
#13851 = B_SPLINE_CURVE_WITH_KNOTS ( 'NONE', 3,
 ( #17407, #40311, #32439, #47462, #13697, #43772, #10026, #44264, #25052, #2633 ),
 .UNSPECIFIED., .F., .F.,
 ( 4, 2, 2, 2, 4 ),
 ( 0.1272669073658256045, 0.2522669073463177924, 0.3772669073268100082, 0.5022669073073021684, 0.6272669072877943286 ),
 .UNSPECIFIED. ) ;
#13852 = ORIENTED_EDGE ( 'NONE', *, *, #39426, .T. ) ;
#13853 = CARTESIAN_POINT ( 'NONE',  ( -18.92057448382017526, -7.919863665830076727, 67.20071783788056052 ) ) ;
#13854 = CARTESIAN_POINT ( 'NONE',  ( -18.31357640787765462, -21.80286941108919763, 68.81514702304139064 ) ) ;
#13855 = ORIENTED_EDGE ( 'NONE', *, *, #9324, .F. ) ;
#13856 = CARTESIAN_POINT ( 'NONE',  ( -11.08846142298070880, -18.82290330472913098, 54.27966884056657904 ) ) ;
#13857 = LINE ( 'NONE', #36511, #37556 ) ;
#13858 = ORIENTED_EDGE ( 'NONE', *, *, #13844, .T. ) ;
#13859 = CARTESIAN_POINT ( 'NONE',  ( -11.94599784085152372, -19.85827745584209580, 58.02658751082835664 ) ) ;
#13860 = EDGE_CURVE ( 'NONE', #17712, #43339, #48529, .T. ) ;
#13861 = CARTESIAN_POINT ( 'NONE',  ( -24.39459507417318562, -17.43899346222085711, 69.66985698250167047 ) ) ;
#13862 =( BOUNDED_CURVE ( )  B_SPLINE_CURVE ( 3, ( #41349, #26584, #27065, #37646 ),
 .UNSPECIFIED., .F., .F. ) 
 B_SPLINE_CURVE_WITH_KNOTS ( ( 4, 4 ),
 ( 0.4074455897393670645, 0.5000000000000000000 ),
 .UNSPECIFIED. ) 
 CURVE ( )  GEOMETRIC_REPRESENTATION_ITEM ( )  RATIONAL_B_SPLINE_CURVE ( ( 0.6983129098260947298, 0.7760317562606947606, 0.8765941196519950740, 0.9999999999999923395 ) ) 
 REPRESENTATION_ITEM ( '' )  );
#13863 = DIRECTION ( 'NONE',  ( -0.3688590060343653887, 0.9294853595766531251, 0.000000000000000000 ) ) ;
#13864 = CARTESIAN_POINT ( 'NONE',  ( -22.19982498210932675, -20.00606685933203366, 58.92009921125114857 ) ) ;
#13865 = ORIENTED_EDGE ( 'NONE', *, *, #41740, .F. ) ;
#13866 = CARTESIAN_POINT ( 'NONE',  ( -22.38280345442485242, -20.36932031849321589, 62.27793240076999126 ) ) ;
#13867 = CARTESIAN_POINT ( 'NONE',  ( -24.18470913683765389, -12.80901137141652768, 69.78715111652664405 ) ) ;
#13868 = VECTOR ( 'NONE', #31780, 1000.000000000000000 ) ;
#13869 = CIRCLE ( 'NONE', #47709, 0.5000000000000004441 ) ;
#13870 = CARTESIAN_POINT ( 'NONE',  ( -7.413536378130524795, -16.17550971119529990, 54.49999999999995026 ) ) ;
#13871 = EDGE_CURVE ( 'NONE', #8571, #33331, #41169, .T. ) ;
#13872 = FACE_OUTER_BOUND ( 'NONE', #11238, .T. ) ;
#13873 = CARTESIAN_POINT ( 'NONE',  ( -22.52409385650551954, -6.426201560718812544, 50.50509628382439331 ) ) ;
#13874 = CARTESIAN_POINT ( 'NONE',  ( -16.84865286310842336, -21.83598151670433296, 68.98088545748413480 ) ) ;
#13875 = ORIENTED_EDGE ( 'NONE', *, *, #17645, .T. ) ;
#13876 = DIRECTION ( 'NONE',  ( -3.071710424422018668E-17, 6.404604876783312462E-16, 1.000000000000000000 ) ) ;
#13877 = EDGE_CURVE ( 'NONE', #47795, #11148, #17396, .T. ) ;
#13878 = CIRCLE ( 'NONE', #28831, 3.982850737850967437 ) ;
#13879 = PLANE ( 'NONE',  #5400 ) ;
#13880 = CARTESIAN_POINT ( 'NONE',  ( -10.00761947527410634, -15.51609109068450465, 57.75288224187332276 ) ) ;
#13881 = ORIENTED_EDGE ( 'NONE', *, *, #11020, .T. ) ;
#13882 =( BOUNDED_CURVE ( )  B_SPLINE_CURVE ( 3, ( #8414, #30355, #8187, #38189 ),
 .UNSPECIFIED., .F., .F. ) 
 B_SPLINE_CURVE_WITH_KNOTS ( ( 4, 4 ),
 ( 0.5000000000000000000, 0.9074455897393690629 ),
 .UNSPECIFIED. ) 
 CURVE ( )  GEOMETRIC_REPRESENTATION_ITEM ( )  RATIONAL_B_SPLINE_CURVE ( ( 1.000000000000022871, 0.4567392136813371861, 0.3561768502900161115, 0.6983129098260846268 ) ) 
 REPRESENTATION_ITEM ( '' )  );
#13883 = LINE ( 'NONE', #14844, #42031 ) ;
#13884 = ORIENTED_EDGE ( 'NONE', *, *, #12913, .F. ) ;
#13885 = VERTEX_POINT ( 'NONE', #785 ) ;
#13886 = ORIENTED_EDGE ( 'NONE', *, *, #22218, .F. ) ;
#13887 = CARTESIAN_POINT ( 'NONE',  ( -13.96006710246513549, -20.89348392225634754, 71.99778020514392551 ) ) ;
#13888 = CARTESIAN_POINT ( 'NONE',  ( -13.11945872550529835, -9.225962324091906197, 67.67942785705487552 ) ) ;
#13889 = LINE ( 'NONE', #28933, #36155 ) ;
#13890 = EDGE_CURVE ( 'NONE', #2810, #27599, #39863, .T. ) ;
#13891 = CARTESIAN_POINT ( 'NONE',  ( -12.91576191806997542, -9.388722997169708151, 71.13453240065665284 ) ) ;
#13892 =( BOUNDED_SURFACE ( )  B_SPLINE_SURFACE ( 3, 1, ( 
 ( #12014, #27026 ),
 ( #42049, #8321 ),
 ( #23335, #4618 ),
 ( #15926, #20616 ),
 ( #25274, #35846 ),
 ( #24559, #25027 ),
 ( #32179, #28486 ) ),
 .UNSPECIFIED., .T., .F., .F. ) 
 B_SPLINE_SURFACE_WITH_KNOTS ( ( 4, 3, 4 ),
 ( 2, 2 ),
 ( 0.000000000000000000, 0.5000000000000000000, 1.000000000000000000 ),
 ( 0.000000000000000000, 1.000000000000000000 ),
 .UNSPECIFIED. ) 
 GEOMETRIC_REPRESENTATION_ITEM ( )  RATIONAL_B_SPLINE_SURFACE ( (
 ( 1.000000000000000000, 1.000000000000000000),
 ( 0.3333333333333335369, 0.3333333333333330373),
 ( 0.3333333333333335369, 0.3333333333333330373),
 ( 1.000000000000000000, 1.000000000000000000),
 ( 0.3333333333333333703, 0.3333333333333333703),
 ( 0.3333333333333333703, 0.3333333333333333703),
 ( 1.000000000000000000, 1.000000000000000000) ) ) 
 REPRESENTATION_ITEM ( '' )  SURFACE ( )  );
#13893 = EDGE_CURVE ( 'NONE', #42385, #18335, #38187, .T. ) ;
#13894 = ORIENTED_EDGE ( 'NONE', *, *, #16079, .F. ) ;
#13895 = ORIENTED_EDGE ( 'NONE', *, *, #29866, .F. ) ;
#13896 = CARTESIAN_POINT ( 'NONE',  ( -19.51784385650551457, -9.790100578890868377, 49.79778022625163203 ) ) ;
#13897 = EDGE_CURVE ( 'NONE', #43519, #43657, #18624, .T. ) ;
#13898 = CARTESIAN_POINT ( 'NONE',  ( -6.424093855413058662, -6.859206544744110623, 52.99999999999998579 ) ) ;
#13899 = CARTESIAN_POINT ( 'NONE',  ( -11.32469277870022850, -18.34471304272907588, 58.10714594244493725 ) ) ;
#13900 = CARTESIAN_POINT ( 'NONE',  ( -17.04284385650551670, -8.811426318492348031, 52.18089403414751359 ) ) ;
#13901 = VECTOR ( 'NONE', #19486, 1000.000000000000000 ) ;
#13902 = AXIS2_PLACEMENT_3D ( 'NONE', #21003, #5980, #28638 ) ;
#13903 = ORIENTED_EDGE ( 'NONE', *, *, #17197, .F. ) ;
#13904 = DIRECTION ( 'NONE',  ( -4.664556984129884891E-06, 8.285185772962303489E-06, -0.9999999999547988239 ) ) ;
#13905 = DIRECTION ( 'NONE',  ( 0.3667195576449455152, -0.9303315355510074491, -1.591455084066187253E-08 ) ) ;
#13906 = VECTOR ( 'NONE', #15374, 1000.000000000000000 ) ;
#13907 = ORIENTED_EDGE ( 'NONE', *, *, #22282, .T. ) ;
#13908 = CARTESIAN_POINT ( 'NONE',  ( -16.97946104448713101, -21.84517140583366057, 72.46543221429990922 ) ) ;
#13909 = ORIENTED_EDGE ( 'NONE', *, *, #4121, .T. ) ;
#13910 = FACE_OUTER_BOUND ( 'NONE', #9256, .T. ) ;
#13911 = CARTESIAN_POINT ( 'NONE',  ( -21.41863048803932656, -8.999699081277377388, 73.61600897546567523 ) ) ;
#13912 = CARTESIAN_POINT ( 'NONE',  ( -21.57785772703445559, -20.99377414531294406, 72.72435196568677895 ) ) ;
#13913 = ORIENTED_EDGE ( 'NONE', *, *, #40227, .F. ) ;
#13914 = CARTESIAN_POINT ( 'NONE',  ( -19.30271930833434979, -8.014115225907463724, 60.11092997145157568 ) ) ;
#13915 = DIRECTION ( 'NONE',  ( 0.9999889394985580493, 0.004703284017506803583, -7.734398264755851970E-09 ) ) ;
#13916 = FACE_OUTER_BOUND ( 'NONE', #20291, .T. ) ;
#13917 = ORIENTED_EDGE ( 'NONE', *, *, #1030, .T. ) ;
#13918 = CARTESIAN_POINT ( 'NONE',  ( -24.83005653327608897, -15.61813750885534979, 73.10280114214759806 ) ) ;
#13919 = DIRECTION ( 'NONE',  ( -3.549360974551883545E-17, 6.371834667872732552E-18, 1.000000000000000000 ) ) ;
#13920 = ORIENTED_EDGE ( 'NONE', *, *, #28577, .F. ) ;
#13921 = CARTESIAN_POINT ( 'NONE',  ( -13.60236376389480384, -20.73382277062339085, 61.80174179654961364 ) ) ;
#13923 = ADVANCED_FACE ( 'NONE', ( #4724 ), #8184, .T. ) ;
#13922 = ORIENTED_EDGE ( 'NONE', *, *, #32918, .T. ) ;
#13924 = CARTESIAN_POINT ( 'NONE',  ( -13.19071075504626478, -8.678814667849811926, 60.54611945450858457 ) ) ;
#13925 = CARTESIAN_POINT ( 'NONE',  ( -13.82689732469268229, -20.87277619789260186, 68.47097268802275494 ) ) ;
#13926 = FACE_OUTER_BOUND ( 'NONE', #8663, .T. ) ;
#13927 = EDGE_CURVE ( 'NONE', #41894, #39596, #45617, .T. ) ;
#13928 = DIRECTION ( 'NONE',  ( 3.141253923644155253E-07, -8.288700512985352896E-07, 0.9999999999996072031 ) ) ;
#13929 = VERTEX_POINT ( 'NONE', #41407 ) ;
#13930 = DIRECTION ( 'NONE',  ( 4.133538118270764137E-06, -2.214839422975871337E-07, 0.9999999999914324089 ) ) ;
#13931 = CARTESIAN_POINT ( 'NONE',  ( -11.35974425695043699, -11.20802616635808313, 64.56370858977317084 ) ) ;
#13932 = CARTESIAN_POINT ( 'NONE',  ( -24.26595263201846109, -13.32969024507516309, 59.66267925069213618 ) ) ;
#13933 = ORIENTED_EDGE ( 'NONE', *, *, #14015, .T. ) ;
#13934 = CARTESIAN_POINT ( 'NONE',  ( -10.16587528726038414, -13.12915031972860902, 71.33015799040107652 ) ) ;
#13935 = AXIS2_PLACEMENT_3D ( 'NONE', #30373, #3512, #18526 ) ;
#13936 = CARTESIAN_POINT ( 'NONE',  ( -19.59334240102641544, -21.51721888655241699, 65.46486226986607448 ) ) ;
#13937 = ORIENTED_EDGE ( 'NONE', *, *, #23854, .F. ) ;
#13938 = EDGE_LOOP ( 'NONE', ( #28721, #22146, #3070, #17445 ) ) ;
#13939 = DIRECTION ( 'NONE',  ( -3.071710424422018668E-17, 6.404604876783312462E-16, 1.000000000000000000 ) ) ;
#13940 = CIRCLE ( 'NONE', #28146, 2.499999999999999556 ) ;
#13941 = FACE_OUTER_BOUND ( 'NONE', #25923, .T. ) ;
#13942 = FACE_OUTER_BOUND ( 'NONE', #23847, .T. ) ;
#13943 = CARTESIAN_POINT ( 'NONE',  ( -13.08910764958623574, -9.312959504979252401, 67.39445176332881715 ) ) ;
#13944 = CARTESIAN_POINT ( 'NONE',  ( -22.56207008003183745, -19.63703213565221262, 72.92928497383269359 ) ) ;
#13945 = AXIS2_PLACEMENT_3D ( 'NONE', #24463, #13340, #39468 ) ;
#13946 = ADVANCED_FACE ( 'NONE', ( #15532 ), #26897, .T. ) ;
#13947 = ORIENTED_EDGE ( 'NONE', *, *, #46888, .T. ) ;
#13948 = ORIENTED_EDGE ( 'NONE', *, *, #23986, .F. ) ;
#13949 = CYLINDRICAL_SURFACE ( 'NONE', #37524, 1.249999999999998668 ) ;
#13950 = EDGE_CURVE ( 'NONE', #39081, #22354, #40341, .T. ) ;
#13951 = EDGE_CURVE ( 'NONE', #9874, #39514, #45362, .T. ) ;
#13952 = EDGE_CURVE ( 'NONE', #12573, #9562, #25731, .T. ) ;
#13953 = CARTESIAN_POINT ( 'NONE',  ( -19.85131540638528591, -8.243492900160722670, 73.82982733467895287 ) ) ;
#13954 = CARTESIAN_POINT ( 'NONE',  ( -12.74141321320493958, -14.42442407569615170, 52.02966884056656482 ) ) ;
#13955 = DIRECTION ( 'NONE',  ( -3.071710424422018668E-17, 6.404604876783312462E-16, 1.000000000000000000 ) ) ;
#13956 = DIRECTION ( 'NONE',  ( 0.000000000000000000, 0.000000000000000000, 1.000000000000000000 ) ) ;
#13957 = CARTESIAN_POINT ( 'NONE',  ( -18.47409385650551528, -9.792211528768504536, 50.49490371617623197 ) ) ;
#13958 = ORIENTED_EDGE ( 'NONE', *, *, #44753, .T. ) ;
#13959 = DIRECTION ( 'NONE',  ( -3.413470714839332458E-33, 1.190614954331866791E-16, -1.000000000000000000 ) ) ;
#13960 = FACE_OUTER_BOUND ( 'NONE', #9668, .T. ) ;
#13961 = CARTESIAN_POINT ( 'NONE',  ( -17.42409385541299471, -14.80920654474435771, 49.52966884056655772 ) ) ;
#13962 = AXIS2_PLACEMENT_3D ( 'NONE', #44721, #18343, #26000 ) ;
#13963 = CARTESIAN_POINT ( 'NONE',  ( -10.01366804335076210, -15.58332129913256381, 61.22444385224647334 ) ) ;
#13964 = VERTEX_POINT ( 'NONE', #11616 ) ;
#13965 = CIRCLE ( 'NONE', #44702, 1.999999999999999334 ) ;
#13966 = VECTOR ( 'NONE', #393, 1000.000000000000114 ) ;
#13967 = CARTESIAN_POINT ( 'NONE',  ( -13.42824119710918573, -20.62712141855529779, 65.13062048310476371 ) ) ;
#13968 = CARTESIAN_POINT ( 'NONE',  ( -20.19231657184298356, -8.325423463105360966, 70.25100341277898508 ) ) ;
#13969 = EDGE_CURVE ( 'NONE', #9242, #17387, #18928, .T. ) ;
#13970 = AXIS2_PLACEMENT_3D ( 'NONE', #18240, #25408, #2744 ) ;
#13971 = CARTESIAN_POINT ( 'NONE',  ( -50.42609385541305755, -14.90920654474419038, 65.04705882352939739 ) ) ;
#13972 = CARTESIAN_POINT ( 'NONE',  ( -10.82146677850202465, -17.29089146116874076, 68.18901905820221998 ) ) ;
#13973 = ORIENTED_EDGE ( 'NONE', *, *, #24140, .F. ) ;
#13974 = CARTESIAN_POINT ( 'NONE',  ( -23.05503254776601096, -18.96763528207466720, 58.99296609845764294 ) ) ;
#13975 = VECTOR ( 'NONE', #47225, 1000.000000000000000 ) ;
#13976 = EDGE_LOOP ( 'NONE', ( #696, #10848, #2266, #17316 ) ) ;
#13977 = DIRECTION ( 'NONE',  ( -0.6607190350374017029, -0.7506333037770471783, 0.000000000000000000 ) ) ;
#13978 = CARTESIAN_POINT ( 'NONE',  ( -14.84909385759799072, -8.112991634885936776, 51.74999426922421719 ) ) ;
#13979 = ORIENTED_EDGE ( 'NONE', *, *, #47323, .F. ) ;
#13980 = CARTESIAN_POINT ( 'NONE',  ( -20.41456109077558168, -8.424717559663436717, 66.78663853121041427 ) ) ;
#13981 = CARTESIAN_POINT ( 'NONE',  ( -15.18659385650551386, -9.302874398569244363, 51.68646062012417985 ) ) ;
#13982 = EDGE_CURVE ( 'NONE', #45729, #17630, #34014, .T. ) ;
#13983 = ORIENTED_EDGE ( 'NONE', *, *, #29935, .F. ) ;
#13984 = CARTESIAN_POINT ( 'NONE',  ( -24.72409385541305582, -14.80920654474427423, 73.09411764705880898 ) ) ;
#13985 = CARTESIAN_POINT ( 'NONE',  ( -20.19053640067075506, -7.838066347919499854, 53.49999999999994316 ) ) ;
#13986 = CARTESIAN_POINT ( 'NONE',  ( -23.89279295945009096, -11.11331726805715725, 69.93564813258274171 ) ) ;
#13987 = VERTEX_POINT ( 'NONE', #308 ) ;
#13988 = CARTESIAN_POINT ( 'NONE',  ( -30.42409385541305156, -6.859206544744110623, 47.99999999999997868 ) ) ;
#13989 = DIRECTION ( 'NONE',  ( -3.071710424422018668E-17, 6.404604876783312462E-16, 1.000000000000000000 ) ) ;
#13990 = CARTESIAN_POINT ( 'NONE',  ( -12.02825722964846022, -10.34976005852228020, 67.49896853033064303 ) ) ;
#13991 = ORIENTED_EDGE ( 'NONE', *, *, #18032, .F. ) ;
#13992 = ORIENTED_EDGE ( 'NONE', *, *, #47634, .T. ) ;
#13993 = CYLINDRICAL_SURFACE ( 'NONE', #22023, 0.1500000000000060729 ) ;
#13994 = CARTESIAN_POINT ( 'NONE',  ( -16.89979169948162863, -10.14008855580012458, 52.02966884056656482 ) ) ;
#13995 = ORIENTED_EDGE ( 'NONE', *, *, #9932, .F. ) ;
#13996 = CARTESIAN_POINT ( 'NONE',  ( -16.70534385759799179, -7.595227055684746986, 51.75156210489594599 ) ) ;
#13997 = AXIS2_PLACEMENT_3D ( 'NONE', #17419, #14183, #40547 ) ;
#13998 = CARTESIAN_POINT ( 'NONE',  ( -12.79154865046270473, -8.973695691655201756, 67.49287406301634462 ) ) ;
#13999 = CARTESIAN_POINT ( 'NONE',  ( -20.56498907581264390, -8.053615130811071054, 66.97442378999858192 ) ) ;
#14000 = AXIS2_PLACEMENT_3D ( 'NONE', #19601, #35342, #1858 ) ;
#14001 = AXIS2_PLACEMENT_3D ( 'NONE', #38344, #12026, #12971 ) ;
#14002 = CARTESIAN_POINT ( 'NONE',  ( -24.72409385541305582, -14.90920654474423124, 69.97058823529410176 ) ) ;
#14003 = ORIENTED_EDGE ( 'NONE', *, *, #38654, .T. ) ;
#14004 = FACE_OUTER_BOUND ( 'NONE', #17865, .T. ) ;
#14005 = ADVANCED_FACE ( 'NONE', ( #45129 ), #4509, .T. ) ;
#14006 = EDGE_CURVE ( 'NONE', #41870, #45990, #2236, .T. ) ;
#14007 = CARTESIAN_POINT ( 'NONE',  ( -13.51031400108801428, -20.61338249540413869, 61.53263022144881234 ) ) ;
#14008 =( BOUNDED_CURVE ( )  B_SPLINE_CURVE ( 3, ( #1904, #40534, #10516, #25521 ),
 .UNSPECIFIED., .F., .F. ) 
 B_SPLINE_CURVE_WITH_KNOTS ( ( 4, 4 ),
 ( 0.4074455897393691739, 0.5000000000000000000 ),
 .UNSPECIFIED. ) 
 CURVE ( )  GEOMETRIC_REPRESENTATION_ITEM ( )  RATIONAL_B_SPLINE_CURVE ( ( 0.6983129098261000589, 0.7760317562606808828, 0.8765941196519739798, 0.9999999999999630296 ) ) 
 REPRESENTATION_ITEM ( '' )  );
#14009 = ORIENTED_EDGE ( 'NONE', *, *, #8985, .F. ) ;
#14010 = ADVANCED_FACE ( 'NONE', ( #37953 ), #6988, .T. ) ;
#14011 = EDGE_CURVE ( 'NONE', #3943, #445, #15447, .T. ) ;
#14012 = VERTEX_POINT ( 'NONE', #9145 ) ;
#14013 = CARTESIAN_POINT ( 'NONE',  ( -20.56934712877496807, -8.555617018170707411, 59.95011231546465069 ) ) ;
#14014 = CARTESIAN_POINT ( 'NONE',  ( -12.46122051107220230, -19.81685944811288635, 64.88146935704573082 ) ) ;
#14015 = EDGE_CURVE ( 'NONE', #18357, #2135, #32034, .T. ) ;
#14016 = CARTESIAN_POINT ( 'NONE',  ( -23.88856641767997857, -11.10584043512839791, 70.01397978569940506 ) ) ;
#14017 = CARTESIAN_POINT ( 'NONE',  ( -14.23827708255551627, -10.77544123782542229, 49.52966884056655772 ) ) ;
#14018 = VERTEX_POINT ( 'NONE', #42649 ) ;
#14019 =( BOUNDED_SURFACE ( )  B_SPLINE_SURFACE ( 3, 1, ( 
 ( #45940, #27220 ),
 ( #42246, #27458 ),
 ( #8506, #23538 ),
 ( #8766, #38536 ),
 ( #32132, #21044 ),
 ( #28193, #35804 ),
 ( #14282, #39754 ) ),
 .UNSPECIFIED., .T., .F., .F. ) 
 B_SPLINE_SURFACE_WITH_KNOTS ( ( 4, 3, 4 ),
 ( 2, 2 ),
 ( 0.000000000000000000, 0.5000000000000000000, 1.000000000000000000 ),
 ( 0.000000000000000000, 1.000000000000000000 ),
 .UNSPECIFIED. ) 
 GEOMETRIC_REPRESENTATION_ITEM ( )  RATIONAL_B_SPLINE_SURFACE ( (
 ( 1.000000000000000000, 1.000000000000000000),
 ( 0.3333333333333335369, 0.3333333333333330373),
 ( 0.3333333333333335369, 0.3333333333333330373),
 ( 1.000000000000000000, 1.000000000000000000),
 ( 0.3333333333333333703, 0.3333333333333333703),
 ( 0.3333333333333333703, 0.3333333333333333703),
 ( 1.000000000000000000, 1.000000000000000000) ) ) 
 REPRESENTATION_ITEM ( '' )  SURFACE ( )  );
#14020 = CARTESIAN_POINT ( 'NONE',  ( -24.25719323842812258, -13.28918340244882224, 59.66267871176336968 ) ) ;
#14021 = CARTESIAN_POINT ( 'NONE',  ( -13.92409385541305511, -25.10920654474410441, 78.99999999999998579 ) ) ;
#14022 = EDGE_CURVE ( 'NONE', #19972, #26269, #24163, .T. ) ;
#14023 = ORIENTED_EDGE ( 'NONE', *, *, #27323, .F. ) ;
#14024 = FACE_OUTER_BOUND ( 'NONE', #25566, .T. ) ;
#14025 = VECTOR ( 'NONE', #24452, 1000.000000000000114 ) ;
#14026 = CARTESIAN_POINT ( 'NONE',  ( -17.84029708445064344, -21.79726103445669239, 61.89152536399645044 ) ) ;
#14027 = CIRCLE ( 'NONE', #10126, 5.249999999999998224 ) ;
#14028 = CARTESIAN_POINT ( 'NONE',  ( -23.33225598143976498, -10.27063514773017516, 59.76236756523886129 ) ) ;
#14029 = EDGE_LOOP ( 'NONE', ( #25070, #14570 ) ) ;
#14030 = FACE_OUTER_BOUND ( 'NONE', #37935, .T. ) ;
#14031 = AXIS2_PLACEMENT_3D ( 'NONE', #27423, #4782, #23988 ) ;
#14032 = AXIS2_PLACEMENT_3D ( 'NONE', #8452, #23734, #19289 ) ;
#14033 = ORIENTED_EDGE ( 'NONE', *, *, #45555, .F. ) ;
#14034 = CARTESIAN_POINT ( 'NONE',  ( -24.31883679440356261, -17.63164986302842152, 66.20003142906764992 ) ) ;
#14035 = CYLINDRICAL_SURFACE ( 'NONE', #35394, 0.1500000000000034084 ) ;
#14036 = CARTESIAN_POINT ( 'NONE',  ( -11.29134393598116937, -11.33126488396075260, 64.16354160640879911 ) ) ;
#14037 = ORIENTED_EDGE ( 'NONE', *, *, #25735, .F. ) ;
#14038 = CARTESIAN_POINT ( 'NONE',  ( -16.21670493413017766, -7.863214532617857522, 60.49468660818079968 ) ) ;
#14039 = DIRECTION ( 'NONE',  ( 2.161108583753623267E-06, 4.147204431722191678E-06, 0.9999999999890650804 ) ) ;
#14040 = CARTESIAN_POINT ( 'NONE',  ( -10.52215041504658188, -13.37196039468858011, 74.97817647370040106 ) ) ;
#14041 = DIRECTION ( 'NONE',  ( 2.872222170658504970E-06, -2.507089450317157248E-06, -0.9999999999927324801 ) ) ;
#14042 = CARTESIAN_POINT ( 'NONE',  ( -13.08575159502176177, -11.85263988192353324, 50.77966884056655772 ) ) ;
#14043 = ORIENTED_EDGE ( 'NONE', *, *, #18187, .T. ) ;
#14044 = CARTESIAN_POINT ( 'NONE',  ( -12.26099810431060533, -10.00863248521528703, 60.85918089305128831 ) ) ;
#14045 = CARTESIAN_POINT ( 'NONE',  ( -9.995623895585607599, -14.24219643007072023, 64.64449787557668969 ) ) ;
#14046 = LINE ( 'NONE', #25168, #25872 ) ;
#14047 = CARTESIAN_POINT ( 'NONE',  ( -23.74619244455239198, -11.68933966055485207, 63.25218278636740621 ) ) ;
#14048 = CARTESIAN_POINT ( 'NONE',  ( -10.81980145280015115, -12.48416413777423806, 60.90926616978132557 ) ) ;
#14049 = CARTESIAN_POINT ( 'NONE',  ( -24.22177711603362482, -13.13842781680106420, 62.83264177645653348 ) ) ;
#14050 = EDGE_LOOP ( 'NONE', ( #19777, #30275, #23714, #11039, #12923 ) ) ;
#14051 = ORIENTED_EDGE ( 'NONE', *, *, #46170, .T. ) ;
#14052 = CARTESIAN_POINT ( 'NONE',  ( -21.12380683100872858, -21.27649256055507365, 65.77109308171978341 ) ) ;
#14053 = CARTESIAN_POINT ( 'NONE',  ( -10.83536388074712598, -17.31742051234312640, 64.92739380450886699 ) ) ;
#14054 = ORIENTED_EDGE ( 'NONE', *, *, #35991, .F. ) ;
#14056 = CARTESIAN_POINT ( 'NONE',  ( -23.56138404952065812, -11.33988834032953008, 70.19210750372964469 ) ) ;
#14055 = CARTESIAN_POINT ( 'NONE',  ( -19.23866564181064831, -21.62168251543363695, 58.82507384655652771 ) ) ;
#14057 = CARTESIAN_POINT ( 'NONE',  ( -36.42409385541304800, -8.109206544743658540, 50.50000000000030553 ) ) ;
#14058 = CARTESIAN_POINT ( 'NONE',  ( -13.67448191250337430, -20.77955027102393615, 64.99188703928707866 ) ) ;
#14059 = LINE ( 'NONE', #48298, #40736 ) ;
#14060 = EDGE_CURVE ( 'NONE', #30297, #15772, #32282, .T. ) ;
#14061 = CARTESIAN_POINT ( 'NONE',  ( -24.78768057424481341, -16.32668859419483454, 53.76227901944321275 ) ) ;
#14062 = CARTESIAN_POINT ( 'NONE',  ( -24.38111619087839799, -15.96880572012975286, 62.47839786477943136 ) ) ;
#14063 = DIRECTION ( 'NONE',  ( -1.000000000000000000, 3.159776991290051445E-16, -3.534154189880001717E-15 ) ) ;
#14064 = CARTESIAN_POINT ( 'NONE',  ( -10.42297871322231551, -14.76125519756164017, 74.86949220091082680 ) ) ;
#14065 = CARTESIAN_POINT ( 'NONE',  ( -14.79922817013080483, -7.836842635312091687, 57.03495431467663224 ) ) ;
#14066 = ADVANCED_FACE ( 'NONE', ( #47303 ), #17037, .T. ) ;
#14067 = EDGE_LOOP ( 'NONE', ( #45732, #45564, #26504, #30846, #28818 ) ) ;
#14068 = CARTESIAN_POINT ( 'NONE',  ( -10.74628672884880132, -17.07053172313825939, 61.17215199736627795 ) ) ;
#14069 = CARTESIAN_POINT ( 'NONE',  ( -23.91439714532632621, -17.43141235356291574, 65.94357239632037704 ) ) ;
#14070 = AXIS2_PLACEMENT_3D ( 'NONE', #23648, #16216, #35429 ) ;
#14071 = CARTESIAN_POINT ( 'NONE',  ( -50.42409385541305511, -14.80920654474410547, 56.99999999999998579 ) ) ;
#14072 = AXIS2_PLACEMENT_3D ( 'NONE', #35083, #19593, #8770 ) ;
#14073 = CARTESIAN_POINT ( 'NONE',  ( -12.68381401182790569, -19.95991009262169413, 68.33657438305763776 ) ) ;
#14074 = VECTOR ( 'NONE', #54, 1000.000000000000114 ) ;
#14075 = AXIS2_PLACEMENT_3D ( 'NONE', #6459, #28852, #22199 ) ;
#14076 = VERTEX_POINT ( 'NONE', #5209 ) ;
#14077 = ORIENTED_EDGE ( 'NONE', *, *, #25022, .T. ) ;
#14078 = CARTESIAN_POINT ( 'NONE',  ( -17.91159385541304161, -8.990409506049200417, 49.61344411288074951 ) ) ;
#14079 = ADVANCED_FACE ( 'NONE', ( #5700 ), #20213, .F. ) ;
#14080 = EDGE_LOOP ( 'NONE', ( #32552, #40754, #28210, #1723 ) ) ;
#14081 = CARTESIAN_POINT ( 'NONE',  ( -17.35252955274262732, -7.359423945522111765, 67.19756513320511715 ) ) ;
#14082 = EDGE_CURVE ( 'NONE', #6974, #8589, #1252, .T. ) ;
#14083 = CARTESIAN_POINT ( 'NONE',  ( -11.80131277442636240, -10.54314289786156777, 67.65463988879716339 ) ) ;
#14084 = AXIS2_PLACEMENT_3D ( 'NONE', #31286, #12575, #45839 ) ;
#14085 = ADVANCED_FACE ( 'NONE', ( #13053 ), #382, .T. ) ;
#14086 = CARTESIAN_POINT ( 'NONE',  ( -20.02409385759798965, -9.359200813967568422, 50.49621490985803263 ) ) ;
#14087 = CARTESIAN_POINT ( 'NONE',  ( -42.41905675134066200, -14.90920654474417972, 63.04029683257916616 ) ) ;
#14088 = ORIENTED_EDGE ( 'NONE', *, *, #25612, .F. ) ;
#14089 = CARTESIAN_POINT ( 'NONE',  ( -10.98855013657561841, -11.05570324207465660, 60.83919106357873829 ) ) ;
#14090 = CARTESIAN_POINT ( 'NONE',  ( -20.89788161767221197, -20.94431024770144489, 62.39999296070408974 ) ) ;
#14091 = ADVANCED_FACE ( 'NONE', ( #40607 ), #32967, .T. ) ;
#14092 = ORIENTED_EDGE ( 'NONE', *, *, #7783, .T. ) ;
#14093 = CARTESIAN_POINT ( 'NONE',  ( -17.03658212107600889, -14.90837637761275403, 53.27966884056655061 ) ) ;
#14094 = CARTESIAN_POINT ( 'NONE',  ( -18.37786432726835883, -21.79469297182707521, 69.10042588711679912 ) ) ;
#14095 = EDGE_LOOP ( 'NONE', ( #41961, #19214, #43951, #44655, #39946 ) ) ;
#14096 = LINE ( 'NONE', #14816, #41755 ) ;
#14097 = CARTESIAN_POINT ( 'NONE',  ( -12.97364571557156232, -9.395203622806569399, 49.41430056510258595 ) ) ;
#14098 = CARTESIAN_POINT ( 'NONE',  ( -16.47989802999360265, -19.41181990985090877, 49.52966884056656482 ) ) ;
#14099 = ORIENTED_EDGE ( 'NONE', *, *, #2914, .F. ) ;
#14100 = CARTESIAN_POINT ( 'NONE',  ( -20.20277394004996196, -7.896613096357342876, 73.86063200510004378 ) ) ;
#14101 = CARTESIAN_POINT ( 'NONE',  ( -12.84719963800786502, -9.512789006345032661, 74.31923006385322594 ) ) ;
#14102 = VECTOR ( 'NONE', #24613, 1000.000000000000000 ) ;
#14103 = CARTESIAN_POINT ( 'NONE',  ( -13.38462506958126319, -20.58719851387657940, 58.04650077714654088 ) ) ;
#14104 = FACE_OUTER_BOUND ( 'NONE', #33484, .T. ) ;
#14105 = VERTEX_POINT ( 'NONE', #21194 ) ;
#14106 = DIRECTION ( 'NONE',  ( -3.071710424422018668E-17, 6.404604876783312462E-16, 1.000000000000000000 ) ) ;
#14107 = LINE ( 'NONE', #18544, #13664 ) ;
#14108 = CARTESIAN_POINT ( 'NONE',  ( -19.19606018965890115, -19.75113282002397597, 49.52966884056656482 ) ) ;
#14109 = CARTESIAN_POINT ( 'NONE',  ( -21.81933826130772047, -16.43558560955401049, 52.02966884056656482 ) ) ;
#14110 = DIRECTION ( 'NONE',  ( 3.597453744745084160E-07, 4.264980248628041219E-06, -0.9999999999908402160 ) ) ;
#14111 = CARTESIAN_POINT ( 'NONE',  ( -17.42409385541299471, -14.80920654474435594, 52.02966884056656482 ) ) ;
#14112 = VERTEX_POINT ( 'NONE', #47537 ) ;
#14113 = CARTESIAN_POINT ( 'NONE',  ( -45.92409385541306222, -14.20920654474410760, 70.50000000000000000 ) ) ;
#14114 = DIRECTION ( 'NONE',  ( 3.395021121731789346E-32, 0.9999954153791273948, 0.003028072113822188795 ) ) ;
#14115 = CARTESIAN_POINT ( 'NONE',  ( -24.31482301288783532, -13.31912224170856796, 59.66267924674056644 ) ) ;
#14116 = EDGE_CURVE ( 'NONE', #9892, #7972, #40621, .T. ) ;
#14117 = ORIENTED_EDGE ( 'NONE', *, *, #16754, .F. ) ;
#14118 = CARTESIAN_POINT ( 'NONE',  ( -19.82413079548422274, -21.27835043604049403, 47.99999999999994316 ) ) ;
#14119 = VERTEX_POINT ( 'NONE', #21907 ) ;
#14120 = ORIENTED_EDGE ( 'NONE', *, *, #45025, .T. ) ;
#14121 = ORIENTED_EDGE ( 'NONE', *, *, #26891, .T. ) ;
#14122 = CARTESIAN_POINT ( 'NONE',  ( -21.32599660273145759, -20.68102258270527471, 72.52446460307699283 ) ) ;
#14123 = CARTESIAN_POINT ( 'NONE',  ( -10.99586753834015695, -11.04334891231907534, 60.86381058728009208 ) ) ;
#14124 = FACE_OUTER_BOUND ( 'NONE', #27016, .T. ) ;
#14125 = CARTESIAN_POINT ( 'NONE',  ( -12.68656345882633296, -9.059469911947932275, 70.89279414395181789 ) ) ;
#14126 = ORIENTED_EDGE ( 'NONE', *, *, #27817, .T. ) ;
#14127 = ORIENTED_EDGE ( 'NONE', *, *, #31002, .T. ) ;
#14128 = CARTESIAN_POINT ( 'NONE',  ( -20.02409385650551599, -6.426201560718813433, 50.50509628382439331 ) ) ;
#14129 = EDGE_CURVE ( 'NONE', #30553, #37645, #1330, .T. ) ;
#14130 = VECTOR ( 'NONE', #18917, 1000.000000000000000 ) ;
#14131 = DIRECTION ( 'NONE',  ( 0.9687793358424821033, -0.2479245821708677133, 0.000000000000000000 ) ) ;
#14132 = DIRECTION ( 'NONE',  ( -0.6538427738826437796, -0.7566304428460742804, 5.916677973164435741E-08 ) ) ;
#14133 = AXIS2_PLACEMENT_3D ( 'NONE', #30560, #8152, #995 ) ;
#14134 = EDGE_CURVE ( 'NONE', #1251, #47122, #34498, .T. ) ;
#14135 = CARTESIAN_POINT ( 'NONE',  ( -18.33659385650551243, -6.915538690918075382, 49.31353937987644542 ) ) ;
#14136 = CIRCLE ( 'NONE', #56, 4.686499999999998778 ) ;
#14137 = EDGE_LOOP ( 'NONE', ( #16472, #38137, #9172, #9120, #11739 ) ) ;
#14138 = ADVANCED_FACE ( 'NONE', ( #14004 ), #7145, .T. ) ;
#14139 = CARTESIAN_POINT ( 'NONE',  ( -10.79785091779906381, -12.40172372778942034, 57.32857331700826364 ) ) ;
#14140 = CARTESIAN_POINT ( 'NONE',  ( -24.80769047312930553, -15.80232199467591947, 69.71802767292497549 ) ) ;
#14141 = VECTOR ( 'NONE', #23339, 1000.000000000000227 ) ;
#14142 = ADVANCED_FACE ( 'NONE', ( #13772 ), #2474, .T. ) ;
#14143 =( BOUNDED_CURVE ( )  B_SPLINE_CURVE ( 3, ( #36603, #14191, #17169, #40092 ),
 .UNSPECIFIED., .F., .F. ) 
 B_SPLINE_CURVE_WITH_KNOTS ( ( 4, 4 ),
 ( 0.9074455897393687298, 1.000000000000000000 ),
 .UNSPECIFIED. ) 
 CURVE ( )  GEOMETRIC_REPRESENTATION_ITEM ( )  RATIONAL_B_SPLINE_CURVE ( ( 0.6983129098261082746, 0.7760317562607114139, 0.8765941196520086187, 1.000000000000000000 ) ) 
 REPRESENTATION_ITEM ( '' )  );
#14144 = ORIENTED_EDGE ( 'NONE', *, *, #18721, .F. ) ;
#14145 = CARTESIAN_POINT ( 'NONE',  ( -17.00326681110915672, -21.84667578895833628, 72.46543211950746866 ) ) ;
#14146 = EDGE_CURVE ( 'NONE', #39884, #26221, #3190, .T. ) ;
#14147 = ORIENTED_EDGE ( 'NONE', *, *, #12314, .F. ) ;
#14148 = DIRECTION ( 'NONE',  ( 0.2696806815386222911, -0.9629498065864410261, 2.003044183322984602E-16 ) ) ;
#14149 = DIRECTION ( 'NONE',  ( 0.8467008005855422015, -0.3141239757129651311, -0.4294460177601863160 ) ) ;
#14150 = LINE ( 'NONE', #40516, #19717 ) ;
#14151 = CARTESIAN_POINT ( 'NONE',  ( -17.04413539470109740, -21.84925844046378174, 72.45071136019464575 ) ) ;
#14152 = ORIENTED_EDGE ( 'NONE', *, *, #47238, .T. ) ;
#14153 = CARTESIAN_POINT ( 'NONE',  ( -12.36756753426621813, -9.896138138887707214, 57.37463480816234096 ) ) ;
#14154 = CARTESIAN_POINT ( 'NONE',  ( -22.83563034752066656, -10.36892392777437522, 63.08688399054229734 ) ) ;
#14155 = CARTESIAN_POINT ( 'NONE',  ( -10.45859239952313224, -15.89938452881993847, 64.79299464097340433 ) ) ;
#14156 = ORIENTED_EDGE ( 'NONE', *, *, #10767, .T. ) ;
#14157 = CARTESIAN_POINT ( 'NONE',  ( -12.75497586646876691, -15.33350870067573801, 52.02966884056656482 ) ) ;
#14158 = CARTESIAN_POINT ( 'NONE',  ( -21.53550107051403018, -9.078485192726875042, 74.01617645989524874 ) ) ;
#14159 =( BOUNDED_CURVE ( )  B_SPLINE_CURVE ( 3, ( #4243, #19254, #540, #23203 ),
 .UNSPECIFIED., .F., .F. ) 
 B_SPLINE_CURVE_WITH_KNOTS ( ( 4, 4 ),
 ( 0.5000000000000000000, 0.9074455897393671755 ),
 .UNSPECIFIED. ) 
 CURVE ( )  GEOMETRIC_REPRESENTATION_ITEM ( )  RATIONAL_B_SPLINE_CURVE ( ( 1.000000000000001776, 0.4567392136813420156, 0.3561768502900327649, 0.6983129098260758560 ) ) 
 REPRESENTATION_ITEM ( '' )  );
#14160 = CARTESIAN_POINT ( 'NONE',  ( -12.54253442593986456, -19.82621537833410841, 64.86674886820043184 ) ) ;
#14161 = EDGE_LOOP ( 'NONE', ( #27587, #6586, #31323, #4220, #2718 ) ) ;
#14162 = CARTESIAN_POINT ( 'NONE',  ( -13.73970650151387751, -20.76112128469266693, 64.98628881673506896 ) ) ;
#14163 = VERTEX_POINT ( 'NONE', #18201 ) ;
#14164 = CARTESIAN_POINT ( 'NONE',  ( -13.23632661096056928, -8.647559330782417675, 60.54676144413815564 ) ) ;
#14165 = CARTESIAN_POINT ( 'NONE',  ( -14.01118748589248320, -10.49619482288619920, 53.49999999999995026 ) ) ;
#14166 = DIRECTION ( 'NONE',  ( 1.000000000000000000, -4.164305804376849172E-17, 1.614929280266638808E-16 ) ) ;
#14167 = CARTESIAN_POINT ( 'NONE',  ( -10.40174263535760524, -17.29725023780839166, 61.34238537770443855 ) ) ;
#14168 = ORIENTED_EDGE ( 'NONE', *, *, #8575, .F. ) ;
#14169 = CYLINDRICAL_SURFACE ( 'NONE', #13440, 0.1499999999999979128 ) ;
#14170 = CARTESIAN_POINT ( 'NONE',  ( -24.23802539630901265, -11.79523892523793371, 59.66890987421792403 ) ) ;
#14171 = EDGE_CURVE ( 'NONE', #20165, #30692, #7291, .T. ) ;
#14172 = CARTESIAN_POINT ( 'NONE',  ( -23.38272234930034088, -18.48272619114020188, 69.40257884200109118 ) ) ;
#14173 = ORIENTED_EDGE ( 'NONE', *, *, #4548, .F. ) ;
#14174 = CARTESIAN_POINT ( 'NONE',  ( -11.22559363225283491, -18.94243559922078646, 64.88560521426357752 ) ) ;
#14175 = VECTOR ( 'NONE', #17611, 1000.000000000000114 ) ;
#14176 =( BOUNDED_SURFACE ( )  B_SPLINE_SURFACE ( 3, 1, ( 
 ( #47252, #25327 ),
 ( #28774, #17442 ),
 ( #47496, #17906 ),
 ( #21398, #17673 ),
 ( #43807, #13496 ),
 ( #36619, #32236 ),
 ( #33171, #5887 ) ),
 .UNSPECIFIED., .T., .F., .F. ) 
 B_SPLINE_SURFACE_WITH_KNOTS ( ( 4, 3, 4 ),
 ( 2, 2 ),
 ( 0.000000000000000000, 0.5000000000000000000, 1.000000000000000000 ),
 ( 0.000000000000000000, 1.000000000000000000 ),
 .UNSPECIFIED. ) 
 GEOMETRIC_REPRESENTATION_ITEM ( )  RATIONAL_B_SPLINE_SURFACE ( (
 ( 1.000000000000000000, 1.000000000000000000),
 ( 0.3333333333333335369, 0.3333333333333330373),
 ( 0.3333333333333335369, 0.3333333333333330373),
 ( 1.000000000000000000, 1.000000000000000000),
 ( 0.3333333333333333703, 0.3333333333333333703),
 ( 0.3333333333333333703, 0.3333333333333333703),
 ( 1.000000000000000000, 1.000000000000000000) ) ) 
 REPRESENTATION_ITEM ( '' )  SURFACE ( )  );
#14177 = CARTESIAN_POINT ( 'NONE',  ( -24.76540221579651302, -16.07765826482591365, 66.17829537637275905 ) ) ;
#14178 = ORIENTED_EDGE ( 'NONE', *, *, #13758, .F. ) ;
#14179 = ORIENTED_EDGE ( 'NONE', *, *, #26539, .T. ) ;
#14180 = CARTESIAN_POINT ( 'NONE',  ( -15.06305009558132646, -21.87596932251961590, 65.21941411614068329 ) ) ;
#14181 = CARTESIAN_POINT ( 'NONE',  ( -10.02748777283063220, -15.69962750030634524, 61.23777819939896006 ) ) ;
#14182 = VECTOR ( 'NONE', #9523, 1000.000000000000000 ) ;
#14183 = DIRECTION ( 'NONE',  ( 1.224646799147353207E-16, 1.000000000000000000, -1.912410701131276611E-32 ) ) ;
#14184 = CARTESIAN_POINT ( 'NONE',  ( -19.45445856626800918, -21.50841060167162055, 61.99503609350492184 ) ) ;
#14185 = DIRECTION ( 'NONE',  ( -0.9410372374137780938, -0.3383029970317210644, -1.029646047569396398E-09 ) ) ;
#14186 = CARTESIAN_POINT ( 'NONE',  ( -11.15036096168905821, -11.58527761980847970, 64.35701831376418625 ) ) ;
#14187 = EDGE_CURVE ( 'NONE', #7578, #3868, #20528, .T. ) ;
#14188 = CARTESIAN_POINT ( 'NONE',  ( -14.75426735376592013, -21.76440006487333179, 61.73626185728981142 ) ) ;
#14189 = ORIENTED_EDGE ( 'NONE', *, *, #15458, .F. ) ;
#14190 = ORIENTED_EDGE ( 'NONE', *, *, #31508, .F. ) ;
#14191 = CARTESIAN_POINT ( 'NONE',  ( -22.90827110196059735, -10.37898438100278575, 63.37185973727753208 ) ) ;
#14192 = VECTOR ( 'NONE', #29109, 1000.000000000000000 ) ;
#14193 = DIRECTION ( 'NONE',  ( -2.866981220435666553E-17, 1.000000000000000000, 1.190614954331866791E-16 ) ) ;
#14194 = DIRECTION ( 'NONE',  ( 0.000000000000000000, 1.000000000000000000, -0.000000000000000000 ) ) ;
#14195 = PLANE ( 'NONE',  #42940 ) ;
#14196 = CARTESIAN_POINT ( 'NONE',  ( -18.60850724411298529, -7.453946191617336403, 73.94090162317939985 ) ) ;
#14197 = EDGE_LOOP ( 'NONE', ( #29501, #5478, #31803, #6914, #27665 ) ) ;
#14198 = B_SPLINE_CURVE_WITH_KNOTS ( 'NONE', 3,
 ( #3247, #51, #44161, #30098, #29847, #10410, #33757, #21491, #47820, #6704 ),
 .UNSPECIFIED., .F., .F.,
 ( 4, 2, 2, 2, 4 ),
 ( 0.000000000000000000, 0.2500000000000000000, 0.5000000000000000000, 0.7500000000000000000, 1.000000000000000000 ),
 .UNSPECIFIED. ) ;
#14199 = CARTESIAN_POINT ( 'NONE',  ( -21.06159385650551741, -9.295667164867525756, 49.30633214617472504 ) ) ;
#14200 = EDGE_LOOP ( 'NONE', ( #4264, #20517, #4712, #8003, #29044 ) ) ;
#14201 = ADVANCED_FACE ( 'NONE', ( #14480 ), #48486, .F. ) ;
#14202 = AXIS2_PLACEMENT_3D ( 'NONE', #25321, #26046, #11273 ) ;
#14203 = CARTESIAN_POINT ( 'NONE',  ( -24.33635500431102017, -15.92417168687779494, 69.64380670067536983 ) ) ;
#14204 = PLANE ( 'NONE',  #16649 ) ;
#14205 = EDGE_CURVE ( 'NONE', #30144, #5852, #7396, .T. ) ;
#14206 = AXIS2_PLACEMENT_3D ( 'NONE', #45534, #11791, #14960 ) ;
#14207 = CARTESIAN_POINT ( 'NONE',  ( -23.19948571119275726, -18.85291137746750323, 65.83861571032234394 ) ) ;
#14208 = CARTESIAN_POINT ( 'NONE',  ( -10.02191638112385697, -15.65273889608829982, 61.15293747381159761 ) ) ;
#14209 = ORIENTED_EDGE ( 'NONE', *, *, #19149, .T. ) ;
#14210 = B_SPLINE_CURVE_WITH_KNOTS ( 'NONE', 1,
 ( #18052, #29397 ),
 .UNSPECIFIED., .F., .F.,
 ( 2, 2 ),
 ( 0.000000000000000000, 1.000000000000000000 ),
 .UNSPECIFIED. ) ;
#14211 = CARTESIAN_POINT ( 'NONE',  ( -13.53189383941936264, -21.16172133628754892, 65.02982926591782586 ) ) ;
#14212 = CARTESIAN_POINT ( 'NONE',  ( -15.77653169993974558, -7.543659789509001179, 67.33996046129556134 ) ) ;
#14213 = AXIS2_PLACEMENT_3D ( 'NONE', #37399, #263, #7896 ) ;
#14214 = DIRECTION ( 'NONE',  ( -0.5562740912439653185, -0.8309988781043535777, -7.851267778718615459E-08 ) ) ;
#14215 = EDGE_CURVE ( 'NONE', #24671, #44110, #33697, .T. ) ;
#14216 = CARTESIAN_POINT ( 'NONE',  ( -24.11345430931175926, -12.58310556425532312, 73.24225580887585352 ) ) ;
#14217 = VERTEX_POINT ( 'NONE', #41111 ) ;
#14218 = CYLINDRICAL_SURFACE ( 'NONE', #24410, 0.1500000000000071554 ) ;
#14219 = EDGE_CURVE ( 'NONE', #35817, #33222, #20800, .T. ) ;
#14220 = VERTEX_POINT ( 'NONE', #11321 ) ;
#14221 = CARTESIAN_POINT ( 'NONE',  ( -23.84953956799437691, -11.90778598363859686, 59.48795493759783426 ) ) ;
#14222 = CARTESIAN_POINT ( 'NONE',  ( -24.87179831301899924, -14.62392340704838745, 62.91285274408475914 ) ) ;
#14223 = VERTEX_POINT ( 'NONE', #29793 ) ;
#14224 = EDGE_CURVE ( 'NONE', #16499, #45977, #4188, .T. ) ;
#14225 = EDGE_CURVE ( 'NONE', #19018, #41432, #13862, .T. ) ;
#14226 = CARTESIAN_POINT ( 'NONE',  ( -22.39682231837810988, -19.80670998913449665, 69.47417992432380629 ) ) ;
#14227 = VECTOR ( 'NONE', #2728, 1000.000000000000114 ) ;
#14228 = CARTESIAN_POINT ( 'NONE',  ( -20.24469333105209046, -8.402151907256357077, 70.26716930211884460 ) ) ;
#14229 = ORIENTED_EDGE ( 'NONE', *, *, #10924, .F. ) ;
#14230 = DIRECTION ( 'NONE',  ( -2.866981220435666553E-17, 1.000000000000000000, 1.190614954331866791E-16 ) ) ;
#14231 = CARTESIAN_POINT ( 'NONE',  ( -11.10871725088146356, -18.76147163815154784, 61.45427695282393898 ) ) ;
#14232 = CARTESIAN_POINT ( 'NONE',  ( -40.92409385541305511, -14.80920654474410725, 74.99999999999998579 ) ) ;
#14233 = ORIENTED_EDGE ( 'NONE', *, *, #46363, .F. ) ;
#14234 = B_SPLINE_CURVE_WITH_KNOTS ( 'NONE', 3,
 ( #44124, #29321, #32530, #6670, #44355, #21689, #47555, #36444, #35966, #3213 ),
 .UNSPECIFIED., .F., .F.,
 ( 4, 2, 2, 2, 4 ),
 ( 0.1272669073658234118, 0.2522669073463141287, 0.3772669073268049011, 0.5022669073072956181, 0.6272669072877863350 ),
 .UNSPECIFIED. ) ;
#14235 = CARTESIAN_POINT ( 'NONE',  ( -13.47975436313424957, -21.12944577273253088, 65.17967206052510676 ) ) ;
#14236 = CARTESIAN_POINT ( 'NONE',  ( -10.22687501107677477, -12.88500788934134889, 67.88832345126935763 ) ) ;
#14237 = DIRECTION ( 'NONE',  ( 0.8201047403141396019, -0.5722134347551369737, -7.883065731092009224E-08 ) ) ;
#14238 = VERTEX_POINT ( 'NONE', #44824 ) ;
#14239 = VERTEX_POINT ( 'NONE', #3940 ) ;
#14240 = VECTOR ( 'NONE', #9196, 1000.000000000000227 ) ;
#14241 = CARTESIAN_POINT ( 'NONE',  ( -12.79111265990729507, -9.490472886863006607, 71.05745174362085947 ) ) ;
#14242 = DIRECTION ( 'NONE',  ( 3.071710424422018668E-17, -6.404604876783312462E-16, -1.000000000000000000 ) ) ;
#14243 = PLANE ( 'NONE',  #35915 ) ;
#14244 = CARTESIAN_POINT ( 'NONE',  ( -14.51159385759799214, -8.990409506049202193, 49.61344411288074951 ) ) ;
#14245 = CARTESIAN_POINT ( 'NONE',  ( -23.77487038158592014, -11.74745262826995607, 62.96690348473899235 ) ) ;
#14246 = CARTESIAN_POINT ( 'NONE',  ( -13.38504989191835826, -9.021193483636507082, 67.52375889928833885 ) ) ;
#14247 = CARTESIAN_POINT ( 'NONE',  ( -15.03263910315855512, -8.176888424288378587, 56.86472059657746314 ) ) ;
#14248 = CARTESIAN_POINT ( 'NONE',  ( -16.51307038081223766, -22.20334437192797949, 65.41902708460563076 ) ) ;
#14249 = EDGE_LOOP ( 'NONE', ( #29559, #24533, #35513, #805, #13973 ) ) ;
#14250 = CARTESIAN_POINT ( 'NONE',  ( -21.00642299473589247, -8.276168789376990631, 60.02780591114678543 ) ) ;
#14251 = EDGE_CURVE ( 'NONE', #30525, #21614, #20987, .T. ) ;
#14252 = AXIS2_PLACEMENT_3D ( 'NONE', #37787, #31132, #19320 ) ;
#14253 = CYLINDRICAL_SURFACE ( 'NONE', #13792, 0.1499999999999992173 ) ;
#14254 = CARTESIAN_POINT ( 'NONE',  ( -19.74200936563729769, -21.46758226568296024, 68.94954551542706156 ) ) ;
#14255 = ORIENTED_EDGE ( 'NONE', *, *, #44739, .F. ) ;
#14256 = ORIENTED_EDGE ( 'NONE', *, *, #42541, .T. ) ;
#14257 = CARTESIAN_POINT ( 'NONE',  ( -16.95219942996303786, -7.374113640801781777, 74.15292427101722694 ) ) ;
#14258 = CIRCLE ( 'NONE', #3291, 1.999999999999999112 ) ;
#14259 = CARTESIAN_POINT ( 'NONE',  ( -22.52885229756875773, -10.01948407182677592, 70.12064572036962318 ) ) ;
#14260 = CARTESIAN_POINT ( 'NONE',  ( -11.41497442304007670, -19.21309820834011362, 71.80190602235010999 ) ) ;
#14261 = B_SPLINE_CURVE_WITH_KNOTS ( 'NONE', 3,
 ( #15140, #45221, #11463, #41504, #19839, #8763, #20315, #16606, #38273, #30925 ),
 .UNSPECIFIED., .F., .F.,
 ( 4, 2, 2, 2, 4 ),
 ( 0.000000000000000000, 0.2500000000000000000, 0.5000000000000000000, 0.7500000000000000000, 1.000000000000000000 ),
 .UNSPECIFIED. ) ;
#14262 = ORIENTED_EDGE ( 'NONE', *, *, #24021, .F. ) ;
#14263 = CARTESIAN_POINT ( 'NONE',  ( -23.94361510234960733, -17.49256946932371548, 65.94916996934229303 ) ) ;
#14264 = CARTESIAN_POINT ( 'NONE',  ( -23.82024019063151243, -17.65337816030916684, 59.11264479274999672 ) ) ;
#14265 = VERTEX_POINT ( 'NONE', #18948 ) ;
#14266 = VECTOR ( 'NONE', #25915, 1000.000000000000000 ) ;
#14267 = FACE_BOUND ( 'NONE', #18614, .T. ) ;
#14268 = CARTESIAN_POINT ( 'NONE',  ( -10.43073328261085386, -14.50439875238632403, 67.85800126138448718 ) ) ;
#14269 = B_SPLINE_CURVE_WITH_KNOTS ( 'NONE', 3,
 ( #41172, #22715, #40674, #26395, #6955, #14539, #30354, #7212, #37452, #26161 ),
 .UNSPECIFIED., .F., .F.,
 ( 4, 2, 2, 2, 4 ),
 ( 0.1272669073658406202, 0.2522669073463340572, 0.3772669073268274387, 0.5022669073073209312, 0.6272669072878143126 ),
 .UNSPECIFIED. ) ;
#14270 = CARTESIAN_POINT ( 'NONE',  ( -23.30016224357493826, -19.38910683590379236, 59.14056577394535452 ) ) ;
#14271 = ORIENTED_EDGE ( 'NONE', *, *, #39426, .F. ) ;
#14272 = CARTESIAN_POINT ( 'NONE',  ( -14.60783717270099835, -21.70648693424663378, 58.35113322083577003 ) ) ;
#14273 = ORIENTED_EDGE ( 'NONE', *, *, #1459, .F. ) ;
#14274 = CARTESIAN_POINT ( 'NONE',  ( -10.47425561207849753, -17.49314520081206936, 64.81234810402725088 ) ) ;
#14275 = CARTESIAN_POINT ( 'NONE',  ( -19.45183578605709940, -21.56134185002573744, 62.29503624138732221 ) ) ;
#14276 = VERTEX_POINT ( 'NONE', #26335 ) ;
#14277 = CARTESIAN_POINT ( 'NONE',  ( -24.17003186015574201, -17.97068590651718267, 59.20367199723977336 ) ) ;
#14278 = EDGE_CURVE ( 'NONE', #19672, #20573, #33960, .T. ) ;
#14279 = ADVANCED_FACE ( 'NONE', ( #3682 ), #7642, .T. ) ;
#14280 = CARTESIAN_POINT ( 'NONE',  ( -19.40609653032597492, -21.57490932759623092, 61.99503665003788910 ) ) ;
#14281 = DIRECTION ( 'NONE',  ( 3.395770063048969188E-06, 1.105252680118079259E-06, -0.9999999999936236561 ) ) ;
#14282 = CARTESIAN_POINT ( 'NONE',  ( -21.79028809537168243, -9.273590339475653366, 63.47681654923867711 ) ) ;
#14283 = DIRECTION ( 'NONE',  ( 0.000000000000000000, 0.000000000000000000, 1.000000000000000000 ) ) ;
#14284 = FACE_OUTER_BOUND ( 'NONE', #20597, .T. ) ;
#14285 = EDGE_LOOP ( 'NONE', ( #4327, #11728 ) ) ;
#14286 = CARTESIAN_POINT ( 'NONE',  ( -24.87105361238793932, -14.59201401153533340, 62.89013408101026670 ) ) ;
#14287 = CARTESIAN_POINT ( 'NONE',  ( -10.78978129946085929, -12.42417050351721919, 57.47857332104950956 ) ) ;
#14288 = CARTESIAN_POINT ( 'NONE',  ( -46.29409385541305966, -14.20920654474410760, 70.91501325280044910 ) ) ;
#14289 = ADVANCED_FACE ( 'NONE', ( #18686 ), #30291, .T. ) ;
#14290 = EDGE_CURVE ( 'NONE', #1066, #48422, #22908, .T. ) ;
#14291 = DIRECTION ( 'NONE',  ( -0.2843796944294934015, -0.9587117342539338560, -5.205739956168919862E-08 ) ) ;
#14292 = CARTESIAN_POINT ( 'NONE',  ( -16.16379340615718618, -22.15191857530921382, 58.47080845268740035 ) ) ;
#14293 = CARTESIAN_POINT ( 'NONE',  ( -24.26335575918792742, -16.30820562957639197, 62.70401880319807475 ) ) ;
#14294 = EDGE_LOOP ( 'NONE', ( #30749, #40581, #27372, #16307 ) ) ;
#14295 = VERTEX_POINT ( 'NONE', #23375 ) ;
#14296 = CARTESIAN_POINT ( 'NONE',  ( -24.02580441457500982, -11.35651424597849690, 66.67860437913579119 ) ) ;
#14297 = CARTESIAN_POINT ( 'NONE',  ( -9.975806665192521905, -14.64185444168544947, 71.48929178254144290 ) ) ;
#14298 = ORIENTED_EDGE ( 'NONE', *, *, #31234, .F. ) ;
#14300 = DIRECTION ( 'NONE',  ( -1.000000000000000000, -2.866981220435666553E-17, 0.000000000000000000 ) ) ;
#14299 = CARTESIAN_POINT ( 'NONE',  ( -23.81302322525746362, -11.80978145726242978, 66.56647414731462220 ) ) ;
#14301 = LINE ( 'NONE', #36477, #42034 ) ;
#14302 = DIRECTION ( 'NONE',  ( 1.224646799147353207E-16, 1.000000000000000000, -1.912410701131276611E-32 ) ) ;
#14303 = CARTESIAN_POINT ( 'NONE',  ( -14.60783614669699304, -21.70648650955843806, 58.35113213314874514 ) ) ;
#14304 =( BOUNDED_CURVE ( )  B_SPLINE_CURVE ( 3, ( #19168, #15444, #24082, #34173 ),
 .UNSPECIFIED., .F., .F. ) 
 B_SPLINE_CURVE_WITH_KNOTS ( ( 4, 4 ),
 ( 1.570796326794896780, 1.780235837034223945 ),
 .UNSPECIFIED. ) 
 CURVE ( )  GEOMETRIC_REPRESENTATION_ITEM ( )  RATIONAL_B_SPLINE_CURVE ( ( 1.000000000000000000, 0.9963479302455153785, 0.9963479302455153785, 1.000000000000000000 ) ) 
 REPRESENTATION_ITEM ( '' )  );
#14305 = CARTESIAN_POINT ( 'NONE',  ( -20.94465790601859467, -8.243431112063134947, 59.95629843672877257 ) ) ;
#14306 = CARTESIAN_POINT ( 'NONE',  ( -12.14862823326899743, -9.548716677428323862, 57.19661362441988928 ) ) ;
#14307 = CARTESIAN_POINT ( 'NONE',  ( -23.32103368030945489, -19.36207380375006082, 59.03410639999821541 ) ) ;
#14308 = CARTESIAN_POINT ( 'NONE',  ( -21.01123981933952223, -20.87838139577334573, 65.73453944496496604 ) ) ;
#14309 = ADVANCED_FACE ( 'NONE', ( #45074 ), #37900, .T. ) ;
#14310 = ORIENTED_EDGE ( 'NONE', *, *, #44962, .T. ) ;
#14311 = CARTESIAN_POINT ( 'NONE',  ( -14.19282086353638661, -8.542981675383003903, 71.01485553001869278 ) ) ;
#14312 = LINE ( 'NONE', #26162, #25840 ) ;
#14313 = CARTESIAN_POINT ( 'NONE',  ( -16.92014803599858652, -22.24222107688192196, 72.42189142509964483 ) ) ;
#14314 = LINE ( 'NONE', #33772, #25596 ) ;
#14315 = DIRECTION ( 'NONE',  ( 0.000000000000000000, 1.000000000000000000, -0.000000000000000000 ) ) ;
#14316 = CARTESIAN_POINT ( 'NONE',  ( -15.03764954898300488, -21.45148416623199594, 58.32185190926050211 ) ) ;
#14317 = CARTESIAN_POINT ( 'NONE',  ( -16.09577467286060681, -7.881796084464274266, 67.23187563413577550 ) ) ;
#14318 =( BOUNDED_SURFACE ( )  B_SPLINE_SURFACE ( 3, 1, ( 
 ( #1082, #41971 ),
 ( #42211, #19554 ),
 ( #8243, #23503 ),
 ( #23259, #34565 ),
 ( #38504, #4786 ),
 ( #19812, #34811 ),
 ( #16083, #31123 ) ),
 .UNSPECIFIED., .T., .F., .F. ) 
 B_SPLINE_SURFACE_WITH_KNOTS ( ( 4, 3, 4 ),
 ( 2, 2 ),
 ( 0.000000000000000000, 0.5000000000000000000, 1.000000000000000000 ),
 ( 0.000000000000000000, 1.000000000000000000 ),
 .UNSPECIFIED. ) 
 GEOMETRIC_REPRESENTATION_ITEM ( )  RATIONAL_B_SPLINE_SURFACE ( (
 ( 1.000000000000000000, 1.000000000000000000),
 ( 0.3333333333333335369, 0.3333333333333330373),
 ( 0.3333333333333335369, 0.3333333333333330373),
 ( 1.000000000000000000, 1.000000000000000000),
 ( 0.3333333333333333703, 0.3333333333333333703),
 ( 0.3333333333333333703, 0.3333333333333333703),
 ( 1.000000000000000000, 1.000000000000000000) ) ) 
 REPRESENTATION_ITEM ( '' )  SURFACE ( )  );
#14319 = ORIENTED_EDGE ( 'NONE', *, *, #2872, .T. ) ;
#14320 = ORIENTED_EDGE ( 'NONE', *, *, #42686, .T. ) ;
#14321 = CARTESIAN_POINT ( 'NONE',  ( -15.83034385541304623, -6.857644439848013640, 49.98602051094139398 ) ) ;
#14322 = VERTEX_POINT ( 'NONE', #45556 ) ;
#14323 = CARTESIAN_POINT ( 'NONE',  ( -23.57241774487040331, -19.01643176791860412, 66.02378197632246781 ) ) ;
#14324 = CARTESIAN_POINT ( 'NONE',  ( -20.36159385759798823, -7.228003583438117552, 51.38655588711986155 ) ) ;
#14325 = CARTESIAN_POINT ( 'NONE',  ( -15.54431827633925778, -7.600127216965169019, 70.78706699909608346 ) ) ;
#14326 = ORIENTED_EDGE ( 'NONE', *, *, #15039, .T. ) ;
#14327 = CARTESIAN_POINT ( 'NONE',  ( -15.37556480380028745, -25.39340727801265984, 54.49999999999995026 ) ) ;
#14328 = ORIENTED_EDGE ( 'NONE', *, *, #40359, .T. ) ;
#14329 = DIRECTION ( 'NONE',  ( -3.071710424422018668E-17, 6.404604876783312462E-16, 1.000000000000000000 ) ) ;
#14330 = CARTESIAN_POINT ( 'NONE',  ( -12.33606046264216083, -19.68942273586096547, 61.40238395048532283 ) ) ;
#14331 = ORIENTED_EDGE ( 'NONE', *, *, #18547, .F. ) ;
#14332 = CARTESIAN_POINT ( 'NONE',  ( -10.52483499103918874, -17.62059296423454313, 68.35367848399930324 ) ) ;
#14333 = CARTESIAN_POINT ( 'NONE',  ( -11.05753694418977773, -11.89913863384178683, 74.85840159189888254 ) ) ;
#14334 = CARTESIAN_POINT ( 'NONE',  ( -9.978978019336247840, -14.53486877964845192, 68.01833503670710002 ) ) ;
#14335 = ORIENTED_EDGE ( 'NONE', *, *, #14584, .T. ) ;
#14336 = CARTESIAN_POINT ( 'NONE',  ( -42.16821150247188399, -14.80920654474418896, 65.04705882352939739 ) ) ;
#14337 = ADVANCED_FACE ( 'NONE', ( #11812 ), #3833, .T. ) ;
#14338 = FACE_OUTER_BOUND ( 'NONE', #26268, .T. ) ;
#14339 = CARTESIAN_POINT ( 'NONE',  ( -19.30706890485013005, -22.01740903849647069, 58.64011989901568711 ) ) ;
#14340 = CARTESIAN_POINT ( 'NONE',  ( -22.17253171379126897, -20.54993857985014216, 59.02088830234949057 ) ) ;
#14341 = ORIENTED_EDGE ( 'NONE', *, *, #550, .F. ) ;
#14342 = CARTESIAN_POINT ( 'NONE',  ( 18.57590614458695200, 3.149984814396855182, 50.78409494584673922 ) ) ;
#14343 = CARTESIAN_POINT ( 'NONE',  ( -15.35564863419042858, -21.49796178713217287, 72.11745751386041547 ) ) ;
#14344 = CARTESIAN_POINT ( 'NONE',  ( -23.23311957587295495, -18.80921362937865382, 69.70860875969677295 ) ) ;
#14345 = EDGE_CURVE ( 'NONE', #20165, #8795, #46987, .T. ) ;
#14346 = CARTESIAN_POINT ( 'NONE',  ( -22.07409385650551670, -9.792211528768504536, 50.49490371617623197 ) ) ;
#14348 = EDGE_CURVE ( 'NONE', #10974, #8357, #1196, .T. ) ;
#14347 = VERTEX_POINT ( 'NONE', #24105 ) ;
#14349 = CARTESIAN_POINT ( 'NONE',  ( -20.78451513435706133, -21.00713107796517320, 62.12943504870421663 ) ) ;
#14350 = CARTESIAN_POINT ( 'NONE',  ( -22.78151503426583702, -19.98625364524674097, 72.75905110386234753 ) ) ;
#14351 = EDGE_LOOP ( 'NONE', ( #47690, #10525, #46604, #23705, #42663 ) ) ;
#14352 = DIRECTION ( 'NONE',  ( -3.071710424422018668E-17, 6.404604876783312462E-16, 1.000000000000000000 ) ) ;
#14353 = EDGE_CURVE ( 'NONE', #5443, #32972, #27308, .T. ) ;
#14354 = CARTESIAN_POINT ( 'NONE',  ( -22.55072583747034543, -9.969711375825740518, 73.48161092416185625 ) ) ;
#14355 = CARTESIAN_POINT ( 'NONE',  ( -18.86321414053259105, -7.899510124550229051, 73.98497555292401273 ) ) ;
#14356 = EDGE_LOOP ( 'NONE', ( #33731, #28649 ) ) ;
#14357 = CARTESIAN_POINT ( 'NONE',  ( -24.38391064099431915, -14.06024038319858960, 73.42271507915008044 ) ) ;
#14358 = ORIENTED_EDGE ( 'NONE', *, *, #38328, .T. ) ;
#14359 = B_SPLINE_CURVE_WITH_KNOTS ( 'NONE', 3,
 ( #19022, #14081, #29132, #36981, #6967, #3760, #10662, #21743, #11153, #44408 ),
 .UNSPECIFIED., .F., .F.,
 ( 4, 2, 2, 2, 4 ),
 ( 0.6272669072877655738, 0.7522669073072847379, 0.8772669073268037909, 1.002266907346323066, 1.127266907365842119 ),
 .UNSPECIFIED. ) ;
#14360 = ORIENTED_EDGE ( 'NONE', *, *, #23381, .F. ) ;
#14361 = ADVANCED_FACE ( 'NONE', ( #31733 ), #23981, .T. ) ;
#14362 = ORIENTED_EDGE ( 'NONE', *, *, #34209, .F. ) ;
#14363 = TOROIDAL_SURFACE ( 'NONE', #5772, 1.700000000000000178, 0.2500000000000000000 ) ;
#14364 = CARTESIAN_POINT ( 'NONE',  ( -16.67409385650551812, -9.792211528768504536, 50.49490371617623197 ) ) ;
#14365 = CARTESIAN_POINT ( 'NONE',  ( -18.82742234287504601, -7.492519652536670627, 70.56406355907934369 ) ) ;
#14366 = CARTESIAN_POINT ( 'NONE',  ( -12.35277332135121675, -20.26681466537264242, 68.45162004874669037 ) ) ;
#14367 = CARTESIAN_POINT ( 'NONE',  ( -13.12596155740353154, -8.723179898376328012, 60.55294873703923031 ) ) ;
#14368 = ORIENTED_EDGE ( 'NONE', *, *, #28510, .T. ) ;
#14369 = VERTEX_POINT ( 'NONE', #20654 ) ;
#14370 = CARTESIAN_POINT ( 'NONE',  ( -16.64909385650551599, -8.104110260919579645, 48.81699501597546487 ) ) ;
#14371 = CARTESIAN_POINT ( 'NONE',  ( -16.87780900865216438, -10.15465445929086208, 49.52966884056655772 ) ) ;
#14372 = CARTESIAN_POINT ( 'NONE',  ( -17.99909385650551741, -8.114302828567740988, 52.18300498402516041 ) ) ;
#14373 = ORIENTED_EDGE ( 'NONE', *, *, #21809, .F. ) ;
#14374 = B_SPLINE_CURVE_WITH_KNOTS ( 'NONE', 3,
 ( #42779, #27507, #19392, #8560, #23585, #38831, #23102, #5351, #46480, #35129 ),
 .UNSPECIFIED., .F., .F.,
 ( 4, 2, 2, 2, 4 ),
 ( 0.6272669072877817831, 0.7522669073072956181, 0.8772669073268095641, 1.002266907346323510, 1.127266907365837234 ),
 .UNSPECIFIED. ) ;
#14375 = DIRECTION ( 'NONE',  ( -3.071710424422018668E-17, 6.404604876783312462E-16, 1.000000000000000000 ) ) ;
#14376 = CYLINDRICAL_SURFACE ( 'NONE', #28384, 1.249999999999998668 ) ;
#14377 =( BOUNDED_SURFACE ( )  B_SPLINE_SURFACE ( 3, 1, ( 
 ( #2468, #48008 ),
 ( #29294, #33203 ),
 ( #14713, #11072 ),
 ( #21662, #40858 ),
 ( #25839, #29786 ),
 ( #17477, #32506 ),
 ( #2934, #44331 ) ),
 .UNSPECIFIED., .T., .F., .F. ) 
 B_SPLINE_SURFACE_WITH_KNOTS ( ( 4, 3, 4 ),
 ( 2, 2 ),
 ( 0.000000000000000000, 0.5000000000000000000, 1.000000000000000000 ),
 ( 0.000000000000000000, 1.000000000000000000 ),
 .UNSPECIFIED. ) 
 GEOMETRIC_REPRESENTATION_ITEM ( )  RATIONAL_B_SPLINE_SURFACE ( (
 ( 1.000000000000000000, 1.000000000000000000),
 ( 0.3333333333333335369, 0.3333333333333330373),
 ( 0.3333333333333335369, 0.3333333333333330373),
 ( 1.000000000000000000, 1.000000000000000000),
 ( 0.3333333333333333703, 0.3333333333333333703),
 ( 0.3333333333333333703, 0.3333333333333333703),
 ( 1.000000000000000000, 1.000000000000000000) ) ) 
 REPRESENTATION_ITEM ( '' )  SURFACE ( )  );
#14378 = CARTESIAN_POINT ( 'NONE',  ( -10.13265761198657167, -13.28029711567731397, 74.87828850252731172 ) ) ;
#14379 = EDGE_CURVE ( 'NONE', #19087, #33339, #5743, .T. ) ;
#14380 = VERTEX_POINT ( 'NONE', #4915 ) ;
#14381 = LINE ( 'NONE', #21576, #46143 ) ;
#14382 = ORIENTED_EDGE ( 'NONE', *, *, #36587, .F. ) ;
#14383 = CARTESIAN_POINT ( 'NONE',  ( -19.48659385541296274, -7.222650657624008375, 49.61879703869468017 ) ) ;
#14384 = CARTESIAN_POINT ( 'NONE',  ( -10.11997142774249880, -16.27652841963017138, 71.64088708844454345 ) ) ;
#14385 = CARTESIAN_POINT ( 'NONE',  ( -9.989611971821876324, -14.32602191216411569, 64.52657349001064802 ) ) ;
#14386 = ADVANCED_FACE ( 'NONE', ( #1695 ), #45695, .T. ) ;
#14387 = AXIS2_PLACEMENT_3D ( 'NONE', #13084, #28118, #16292 ) ;
#14388 = VERTEX_POINT ( 'NONE', #31969 ) ;
#14389 = CARTESIAN_POINT ( 'NONE',  ( -10.62096356601691660, -12.92974252456203743, 60.95420737114066156 ) ) ;
#14390 = CARTESIAN_POINT ( 'NONE',  ( -15.31846949587358431, -21.95558135219415163, 72.22388224403276524 ) ) ;
#14391 = LINE ( 'NONE', #44729, #42579 ) ;
#14392 = EDGE_LOOP ( 'NONE', ( #12985, #47503, #12996, #10050 ) ) ;
#14393 = CARTESIAN_POINT ( 'NONE',  ( -10.37424879026167979, -14.74379641705365174, 71.62222930935075738 ) ) ;
#14394 = CARTESIAN_POINT ( 'NONE',  ( -44.67409385541304800, -15.80920654474410725, 70.50000000000000000 ) ) ;
#14395 = CARTESIAN_POINT ( 'NONE',  ( -21.47456293661849713, -9.038556783377254433, 70.41660404402310292 ) ) ;
#14396 = ORIENTED_EDGE ( 'NONE', *, *, #29317, .T. ) ;
#14397 = CARTESIAN_POINT ( 'NONE',  ( -19.17604249790256077, -21.63836284480991878, 58.53979515915469278 ) ) ;
#14398 = ORIENTED_EDGE ( 'NONE', *, *, #7729, .T. ) ;
#14399 = DIRECTION ( 'NONE',  ( -0.9979768094191905359, -0.06357898915123237626, -3.501668460141644652E-17 ) ) ;
#14400 = CYLINDRICAL_SURFACE ( 'NONE', #17146, 2.000000000000000000 ) ;
#14401 = EDGE_CURVE ( 'NONE', #37972, #43339, #43328, .T. ) ;
#14402 = CARTESIAN_POINT ( 'NONE',  ( -14.29154966128864857, -8.493214084104669936, 70.73517404774455031 ) ) ;
#14403 = EDGE_LOOP ( 'NONE', ( #13865, #5098 ) ) ;
#14404 = CARTESIAN_POINT ( 'NONE',  ( -24.15060978519040091, -18.01196315242050261, 59.26024333157867119 ) ) ;
#14405 = ADVANCED_FACE ( 'NONE', ( #20891 ), #10033, .T. ) ;
#14406 = ORIENTED_EDGE ( 'NONE', *, *, #19430, .T. ) ;
#14407 = CARTESIAN_POINT ( 'NONE',  ( -10.96142808812597735, -11.10142881709785101, 64.33537400591416144 ) ) ;
#14408 = CARTESIAN_POINT ( 'NONE',  ( -15.55648817577099585, -8.010769314271311003, 74.09457776258329886 ) ) ;
#14409 = ORIENTED_EDGE ( 'NONE', *, *, #7580, .F. ) ;
#14410 = ADVANCED_FACE ( 'NONE', ( #10535 ), #13949, .T. ) ;
#14411 = CARTESIAN_POINT ( 'NONE',  ( -19.61601346313181082, -21.50980264518277707, 65.46486213821819433 ) ) ;
#14412 = VERTEX_POINT ( 'NONE', #2886 ) ;
#14413 = ORIENTED_EDGE ( 'NONE', *, *, #38380, .T. ) ;
#14414 = CARTESIAN_POINT ( 'NONE',  ( -14.21171452256333012, -10.65672306833168115, 49.52966884056655772 ) ) ;
#14415 = DIRECTION ( 'NONE',  ( 0.5497669574358331479, -0.8353180786453389128, -7.898837270956392542E-08 ) ) ;
#14416 = CARTESIAN_POINT ( 'NONE',  ( -17.42409385541299471, -14.80920654474435594, 52.02966884056656482 ) ) ;
#14418 = ADVANCED_FACE ( 'NONE', ( #28998 ), #6835, .T. ) ;
#14417 = CARTESIAN_POINT ( 'NONE',  ( -16.92050523043788957, -21.84918965566402704, 65.38131313066115524 ) ) ;
#14419 = CARTESIAN_POINT ( 'NONE',  ( -14.84266674508882744, -8.302458032430561019, 60.61996277900374253 ) ) ;
#14420 = CARTESIAN_POINT ( 'NONE',  ( -24.72409385541305582, -14.80920654474419962, 66.95294117647057419 ) ) ;
#14421 = CARTESIAN_POINT ( 'NONE',  ( -17.83878094755516486, -7.370707184827939074, 60.27399068567451934 ) ) ;
#14422 = VERTEX_POINT ( 'NONE', #29247 ) ;
#14423 = ORIENTED_EDGE ( 'NONE', *, *, #31751, .T. ) ;
#14424 = FACE_OUTER_BOUND ( 'NONE', #44926, .T. ) ;
#14425 = CARTESIAN_POINT ( 'NONE',  ( -19.91954111600424326, -8.269053586180861615, 74.00631301559766939 ) ) ;
#14426 = DIRECTION ( 'NONE',  ( -4.556087730354191539E-06, 5.696494007380787447E-06, -0.9999999999733960587 ) ) ;
#14427 = CARTESIAN_POINT ( 'NONE',  ( -12.74141321320493958, -14.42442407569615348, 49.52966884056655772 ) ) ;
#14428 = CARTESIAN_POINT ( 'NONE',  ( -18.63018970549565978, -7.457396494496333794, 73.95569010969242640 ) ) ;
#14429 = VERTEX_POINT ( 'NONE', #18142 ) ;
#14430 =( BOUNDED_CURVE ( )  B_SPLINE_CURVE ( 3, ( #30612, #42167, #45633, #8430 ),
 .UNSPECIFIED., .F., .F. ) 
 B_SPLINE_CURVE_WITH_KNOTS ( ( 4, 4 ),
 ( 0.000000000000000000, 0.4074455897393691739 ),
 .UNSPECIFIED. ) 
 CURVE ( )  GEOMETRIC_REPRESENTATION_ITEM ( )  RATIONAL_B_SPLINE_CURVE ( ( 1.000000000000000000, 0.4567392136813301917, 0.3561768502900296562, 0.6983129098260982826 ) ) 
 REPRESENTATION_ITEM ( '' )  );
#14431 = CARTESIAN_POINT ( 'NONE',  ( -17.91159385650551528, -6.922745924619793101, 51.69366785382590024 ) ) ;
#14432 = ORIENTED_EDGE ( 'NONE', *, *, #36572, .T. ) ;
#14433 = CARTESIAN_POINT ( 'NONE',  ( -24.34625421034940018, -15.85315431188110225, 69.81690982159123848 ) ) ;
#14434 = CARTESIAN_POINT ( 'NONE',  ( -19.74200936563729769, -21.46758226568296024, 68.94954551542706156 ) ) ;
#14435 = CARTESIAN_POINT ( 'NONE',  ( -10.78905007119639059, -17.04131871017208155, 61.17359741050059796 ) ) ;
#14436 = CARTESIAN_POINT ( 'NONE',  ( -11.19252025440407472, -18.89210953133327919, 64.94718283645474344 ) ) ;
#14437 = ADVANCED_FACE ( 'NONE', ( #36134 ), #44048, .T. ) ;
#14438 = ORIENTED_EDGE ( 'NONE', *, *, #5156, .T. ) ;
#14439 =( BOUNDED_SURFACE ( )  B_SPLINE_SURFACE ( 3, 1, ( 
 ( #11196, #41465 ),
 ( #37764, #42201 ),
 ( #30404, #19303 ),
 ( #45420, #11673 ),
 ( #23021, #15841 ),
 ( #3804, #27180 ),
 ( #19545, #34305 ) ),
 .UNSPECIFIED., .T., .F., .F. ) 
 B_SPLINE_SURFACE_WITH_KNOTS ( ( 4, 3, 4 ),
 ( 2, 2 ),
 ( 0.000000000000000000, 0.5000000000000000000, 1.000000000000000000 ),
 ( 0.000000000000000000, 1.000000000000000000 ),
 .UNSPECIFIED. ) 
 GEOMETRIC_REPRESENTATION_ITEM ( )  RATIONAL_B_SPLINE_SURFACE ( (
 ( 1.000000000000000000, 1.000000000000000000),
 ( 0.3333333333333335369, 0.3333333333333330373),
 ( 0.3333333333333335369, 0.3333333333333330373),
 ( 1.000000000000000000, 1.000000000000000000),
 ( 0.3333333333333333703, 0.3333333333333333703),
 ( 0.3333333333333333703, 0.3333333333333333703),
 ( 1.000000000000000000, 1.000000000000000000) ) ) 
 REPRESENTATION_ITEM ( '' )  SURFACE ( )  );
#14440 = DIRECTION ( 'NONE',  ( 7.340779720199402358E-07, -8.195271891664201640E-07, 0.9999999999993947064 ) ) ;
#14441 = CARTESIAN_POINT ( 'NONE',  ( -21.65477688667505518, -9.232350752012335349, 66.66149992610201025 ) ) ;
#14442 = B_SPLINE_CURVE_WITH_KNOTS ( 'NONE', 3,
 ( #23488, #8458, #5251, #34547, #12388, #19796, #585, #26694, #15580, #1069 ),
 .UNSPECIFIED., .F., .F.,
 ( 4, 2, 2, 2, 4 ),
 ( 0.000000000000000000, 0.2500000000000000000, 0.5000000000000000000, 0.7500000000000000000, 1.000000000000000000 ),
 .UNSPECIFIED. ) ;
#14443 = ORIENTED_EDGE ( 'NONE', *, *, #10422, .F. ) ;
#14444 = CARTESIAN_POINT ( 'NONE',  ( -15.55910223978619200, -7.596364071707596644, 70.80263970476339352 ) ) ;
#14445 = CARTESIAN_POINT ( 'NONE',  ( -10.13546849559099883, -16.35223934790467837, 71.60783702123018202 ) ) ;
#14446 = ORIENTED_EDGE ( 'NONE', *, *, #23462, .F. ) ;
#14447 = EDGE_CURVE ( 'NONE', #34717, #3552, #28992, .T. ) ;
#14448 = DIRECTION ( 'NONE',  ( 0.3566357048164924826, -0.9342435303763380050, 8.054691247936225743E-09 ) ) ;
#14449 =( BOUNDED_CURVE ( )  B_SPLINE_CURVE ( 3, ( #37498, #26688, #41451, #16062 ),
 .UNSPECIFIED., .F., .F. ) 
 B_SPLINE_CURVE_WITH_KNOTS ( ( 4, 4 ),
 ( 0.4074455897393585713, 0.5000000000000000000 ),
 .UNSPECIFIED. ) 
 CURVE ( )  GEOMETRIC_REPRESENTATION_ITEM ( )  RATIONAL_B_SPLINE_CURVE ( ( 0.6983129098260824064, 0.7760317562606839914, 0.8765941196519885237, 0.9999999999999921174 ) ) 
 REPRESENTATION_ITEM ( '' )  );
#14450 = ORIENTED_EDGE ( 'NONE', *, *, #23807, .T. ) ;
#14451 = VECTOR ( 'NONE', #33262, 1000.000000000000227 ) ;
#14452 = CARTESIAN_POINT ( 'NONE',  ( -18.89533436007378597, -9.769568524266551535, 52.02966884056656482 ) ) ;
#14453 = ORIENTED_EDGE ( 'NONE', *, *, #44169, .F. ) ;
#14454 = CARTESIAN_POINT ( 'NONE',  ( -23.96969171478034610, -17.42802645644465542, 66.24357243629151526 ) ) ;
#14455 = AXIS2_PLACEMENT_3D ( 'NONE', #29035, #6636, #29286 ) ;
#14456 = CARTESIAN_POINT ( 'NONE',  ( -22.07805708657739885, -20.69058616546009333, 54.27966884056654351 ) ) ;
#14457 = ADVANCED_FACE ( 'NONE', ( #14424 ), #47484, .T. ) ;
#14458 = VERTEX_POINT ( 'NONE', #13717 ) ;
#14459 = CARTESIAN_POINT ( 'NONE',  ( -23.37999588001404661, -18.58199455739222827, 69.57899840282863124 ) ) ;
#14460 = CARTESIAN_POINT ( 'NONE',  ( -11.09242024638942148, -18.73509009507580458, 61.37687196085482810 ) ) ;
#14461 = B_SPLINE_CURVE_WITH_KNOTS ( 'NONE', 3,
 ( #23966, #2027, #5245, #35269, #28619, #39214, #16551, #9187, #24205, #20513 ),
 .UNSPECIFIED., .F., .F.,
 ( 4, 2, 2, 2, 4 ),
 ( 0.1272669073658570793, 0.2522669073463328360, 0.3772669073268085649, 0.5022669073072844048, 0.6272669072877601337 ),
 .UNSPECIFIED. ) ;
#14462 = B_SPLINE_CURVE_WITH_KNOTS ( 'NONE', 3,
 ( #18255, #44883, #10417, #14064, #29113, #25426, #29357, #47597, #18502, #44388 ),
 .UNSPECIFIED., .F., .F.,
 ( 4, 2, 2, 2, 4 ),
 ( 0.000000000000000000, 0.2500000000000000000, 0.5000000000000000000, 0.7500000000000000000, 1.000000000000000000 ),
 .UNSPECIFIED. ) ;
#14463 = ORIENTED_EDGE ( 'NONE', *, *, #2901, .F. ) ;
#14464 = CARTESIAN_POINT ( 'NONE',  ( -9.990623027812100432, -14.31192454061599229, 64.57299275950818185 ) ) ;
#14465 = EDGE_CURVE ( 'NONE', #14468, #47695, #22096, .T. ) ;
#14466 = DIRECTION ( 'NONE',  ( -0.09332174201254901658, -0.9956360040033422898, 0.000000000000000000 ) ) ;
#14467 = DIRECTION ( 'NONE',  ( 0.9687793358424821033, -0.2479245821708677133, 0.000000000000000000 ) ) ;
#14468 = VERTEX_POINT ( 'NONE', #21852 ) ;
#14469 = ORIENTED_EDGE ( 'NONE', *, *, #12879, .T. ) ;
#14470 = CARTESIAN_POINT ( 'NONE',  ( -23.39277566991647817, -10.35052415317939278, 59.74170096327360113 ) ) ;
#14471 = CARTESIAN_POINT ( 'NONE',  ( -24.69852180232685157, -16.41745880042978101, 59.30827708941524889 ) ) ;
#14472 = LINE ( 'NONE', #2466, #48502 ) ;
#14473 = EDGE_CURVE ( 'NONE', #27084, #46946, #36846, .T. ) ;
#14474 = CARTESIAN_POINT ( 'NONE',  ( -15.80534385759798965, -7.595227055684746986, 51.75156210489594599 ) ) ;
#14475 = DIRECTION ( 'NONE',  ( -0.3478314405900310158, -0.9375570856950865561, 0.000000000000000000 ) ) ;
#14476 = DIRECTION ( 'NONE',  ( 0.000000000000000000, 0.000000000000000000, -1.000000000000000000 ) ) ;
#14477 = CARTESIAN_POINT ( 'NONE',  ( -14.28659385759798894, -7.222650657624104298, 49.61879703869476543 ) ) ;
#14478 = CARTESIAN_POINT ( 'NONE',  ( -10.66703338591908690, -12.79807911521252883, 64.41836111017862265 ) ) ;
#14479 = VERTEX_POINT ( 'NONE', #40327 ) ;
#14480 = FACE_OUTER_BOUND ( 'NONE', #25428, .T. ) ;
#14481 =( LENGTH_UNIT ( ) NAMED_UNIT ( * ) SI_UNIT ( .MILLI., .METRE. ) );
#14482 = CARTESIAN_POINT ( 'NONE',  ( -24.87385082706414607, -14.87839859077033822, 59.49946141495512819 ) ) ;
#14483 = CARTESIAN_POINT ( 'NONE',  ( -13.57788212914492476, -8.959029760704318335, 60.51120652236025421 ) ) ;
#14484 = EDGE_CURVE ( 'NONE', #43727, #24972, #45978, .T. ) ;
#14485 = ORIENTED_EDGE ( 'NONE', *, *, #30763, .F. ) ;
#14486 = EDGE_CURVE ( 'NONE', #26903, #2787, #14143, .T. ) ;
#14487 = AXIS2_PLACEMENT_3D ( 'NONE', #12711, #9755, #43492 ) ;
#14488 = ORIENTED_EDGE ( 'NONE', *, *, #20934, .F. ) ;
#14489 = ADVANCED_FACE ( 'NONE', ( #10768 ), #34021, .T. ) ;
#14490 = CARTESIAN_POINT ( 'NONE',  ( -11.19706266256277694, -11.50303319689152737, 67.63336710488009373 ) ) ;
#14491 = CIRCLE ( 'NONE', #7491, 0.3999999999999975797 ) ;
#14492 = DIRECTION ( 'NONE',  ( -0.9930145540378111368, 0.1179919296777755672, 4.526730167978065139E-08 ) ) ;
#14493 = CARTESIAN_POINT ( 'NONE',  ( -10.00963232195547903, -14.08228650966967876, 61.01797661620253166 ) ) ;
#14494 = CARTESIAN_POINT ( 'NONE',  ( -11.64235247690698571, -18.84330696305777408, 68.51689631558762983 ) ) ;
#14495 = ORIENTED_EDGE ( 'NONE', *, *, #34287, .F. ) ;
#14496 = CARTESIAN_POINT ( 'NONE',  ( -24.47628618758622210, -12.40716135712818868, 73.34887263294206150 ) ) ;
#14497 = CARTESIAN_POINT ( 'NONE',  ( -13.06825169942196752, -9.255684228991221119, 74.46356075877366720 ) ) ;
#14498 = ORIENTED_EDGE ( 'NONE', *, *, #45151, .F. ) ;
#14499 = CARTESIAN_POINT ( 'NONE',  ( -21.51080377022508472, -17.10312989180208731, 52.02966884056656482 ) ) ;
#14500 = CARTESIAN_POINT ( 'NONE',  ( -23.06636451794179976, -10.57604847539621851, 63.37186202593429130 ) ) ;
#14501 = CARTESIAN_POINT ( 'NONE',  ( -16.98261445675647963, -21.79527095473675402, 72.46543221550747660 ) ) ;
#14502 = ORIENTED_EDGE ( 'NONE', *, *, #17968, .T. ) ;
#14503 = ORIENTED_EDGE ( 'NONE', *, *, #24110, .F. ) ;
#14504 = CARTESIAN_POINT ( 'NONE',  ( -23.79119299285383349, -10.94096587987842639, 73.46854977554494326 ) ) ;
#14505 = CARTESIAN_POINT ( 'NONE',  ( -24.39022378835582927, -14.12080876765324078, 69.87948639740776002 ) ) ;
#14506 = ORIENTED_EDGE ( 'NONE', *, *, #34445, .F. ) ;
#14507 = CARTESIAN_POINT ( 'NONE',  ( -16.26183769579148475, -7.855670737815882987, 60.50028478907628937 ) ) ;
#14508 = CARTESIAN_POINT ( 'NONE',  ( -24.17147434587301191, -12.75550446831573126, 73.65714286828524848 ) ) ;
#14509 = CARTESIAN_POINT ( 'NONE',  ( -22.38659385650551670, -9.302874398569244363, 51.68646062012417985 ) ) ;
#14510 = LINE ( 'NONE', #6922, #22868 ) ;
#14511 = CARTESIAN_POINT ( 'NONE',  ( -10.05522069275589736, -15.90572865272950409, 64.60747954325734099 ) ) ;
#14512 = CARTESIAN_POINT ( 'NONE',  ( -22.96481576609224717, -19.16891988936071556, 58.89882756593014790 ) ) ;
#14513 = DIRECTION ( 'NONE',  ( 0.3996021513128669711, 0.9166886716143756164, 9.834836654444491158E-09 ) ) ;
#14514 = ORIENTED_EDGE ( 'NONE', *, *, #34637, .T. ) ;
#14515 = CARTESIAN_POINT ( 'NONE',  ( -16.94392004664433671, -22.24372332546570163, 72.36554421717424646 ) ) ;
#14516 = CARTESIAN_POINT ( 'NONE',  ( -17.42409385541300892, -14.80920654474439502, 75.49999999999994316 ) ) ;
#14517 = CARTESIAN_POINT ( 'NONE',  ( -14.48623784902251899, -7.962796613987291217, 63.96791570607779676 ) ) ;
#14518 = AXIS2_PLACEMENT_3D ( 'NONE', #47171, #28466, #35588 ) ;
#14519 = FACE_OUTER_BOUND ( 'NONE', #41995, .T. ) ;
#14520 = EDGE_CURVE ( 'NONE', #44357, #25391, #37098, .T. ) ;
#14521 = FACE_OUTER_BOUND ( 'NONE', #14080, .T. ) ;
#14522 = DIRECTION ( 'NONE',  ( -0.1240347345892086200, 1.145860353393066553E-16, -0.9922778767136676281 ) ) ;
#14523 = AXIS2_PLACEMENT_3D ( 'NONE', #9911, #43654, #13577 ) ;
#14524 = ORIENTED_EDGE ( 'NONE', *, *, #26409, .T. ) ;
#14525 = ORIENTED_EDGE ( 'NONE', *, *, #2181, .F. ) ;
#14526 = CARTESIAN_POINT ( 'NONE',  ( -18.30727046116018286, -21.75326869042403288, 69.11514702556002021 ) ) ;
#14527 = DIRECTION ( 'NONE',  ( -0.000000000000000000, -1.000000000000000000, 0.000000000000000000 ) ) ;
#14528 = VERTEX_POINT ( 'NONE', #19373 ) ;
#14530 = CARTESIAN_POINT ( 'NONE',  ( -14.09390608941906819, -21.02325857983911561, 72.22047898906316732 ) ) ;
#14529 = CARTESIAN_POINT ( 'NONE',  ( -17.72612443559818018, -7.765381109175947927, 60.36588690973874094 ) ) ;
#14531 = CARTESIAN_POINT ( 'NONE',  ( -13.40146611816620847, -9.019296439419454359, 60.73390453098559050 ) ) ;
#14532 = CARTESIAN_POINT ( 'NONE',  ( -20.69509153224808173, -8.115601224564374050, 63.49616927690831858 ) ) ;
#14533 = CARTESIAN_POINT ( 'NONE',  ( -12.32278866559117780, -19.67576434477648917, 61.41150688479135766 ) ) ;
#14534 = CARTESIAN_POINT ( 'NONE',  ( -24.30164805153987473, -16.37256343635084477, 63.00817566860099106 ) ) ;
#14535 = CARTESIAN_POINT ( 'NONE',  ( -45.55409385541306477, -14.20920654474410760, 71.05212771298751306 ) ) ;
#14536 = CARTESIAN_POINT ( 'NONE',  ( -11.46592951257400905, -19.28193112475830873, 71.82539333254983660 ) ) ;
#14537 = CARTESIAN_POINT ( 'NONE',  ( -16.71067917923000579, -21.77319752884913129, 68.71177304229871652 ) ) ;
#14538 = ORIENTED_EDGE ( 'NONE', *, *, #7295, .F. ) ;
#14539 = CARTESIAN_POINT ( 'NONE',  ( -24.11691640979936224, -11.53669002245029951, 63.14556576031020541 ) ) ;
#14540 = CARTESIAN_POINT ( 'NONE',  ( -10.48085305489969521, -13.91959585118948617, 57.74825035244229809 ) ) ;
#14541 = CARTESIAN_POINT ( 'NONE',  ( -24.71633098454773148, -13.28334072004885869, 59.52414474877395634 ) ) ;
#14542 = CARTESIAN_POINT ( 'NONE',  ( -24.29424039954640691, -13.46050364628763063, 59.43438299228309774 ) ) ;
#14543 = CARTESIAN_POINT ( 'NONE',  ( -24.13185811504778755, -12.61356036044664464, 66.45813649863244166 ) ) ;
#14544 = FACE_OUTER_BOUND ( 'NONE', #22056, .T. ) ;
#14545 = CARTESIAN_POINT ( 'NONE',  ( -15.93879930885702656, -7.917138641544857691, 67.15479422225767792 ) ) ;
#14547 = ORIENTED_EDGE ( 'NONE', *, *, #42919, .F. ) ;
#14546 = EDGE_CURVE ( 'NONE', #31797, #7279, #23344, .T. ) ;
#14548 = ORIENTED_EDGE ( 'NONE', *, *, #1487, .T. ) ;
#14549 = CARTESIAN_POINT ( 'NONE',  ( -14.19909385541304125, -8.105421454601382081, 49.25000573077640098 ) ) ;
#14550 = VERTEX_POINT ( 'NONE', #18387 ) ;
#14551 = EDGE_CURVE ( 'NONE', #26197, #39806, #39733, .T. ) ;
#14552 = ADVANCED_FACE ( 'NONE', ( #48433 ), #27700, .T. ) ;
#14553 = CARTESIAN_POINT ( 'NONE',  ( -45.92409385541306222, -13.51240245935757578, 68.09574468085106957 ) ) ;
#14554 = CARTESIAN_POINT ( 'NONE',  ( -11.68672781637937419, -10.05669048882576533, 67.68392176937598492 ) ) ;
#14555 = B_SPLINE_CURVE_WITH_KNOTS ( 'NONE', 3,
 ( #7992, #45405, #12147, #15332, #30148, #27168, #37751, #42189, #30634, #34055 ),
 .UNSPECIFIED., .F., .F.,
 ( 4, 2, 2, 2, 4 ),
 ( 0.000000000000000000, 0.2500000000000000000, 0.5000000000000000000, 0.7500000000000000000, 1.000000000000000000 ),
 .UNSPECIFIED. ) ;
#14556 = CIRCLE ( 'NONE', #24040, 0.5560000000000009379 ) ;
#14557 = CARTESIAN_POINT ( 'NONE',  ( -24.61808062994217394, -12.87247312369571439, 66.42529869958860900 ) ) ;
#14558 = CARTESIAN_POINT ( 'NONE',  ( -15.53801481854660871, -7.601731716485351065, 70.74843289815109415 ) ) ;
#14559 = ORIENTED_EDGE ( 'NONE', *, *, #3435, .F. ) ;
#14560 = CARTESIAN_POINT ( 'NONE',  ( -23.08399920647563519, -9.964749700819742984, 66.73456405495493016 ) ) ;
#14561 = CARTESIAN_POINT ( 'NONE',  ( -12.50766613833180152, -19.86205114983803810, 64.86674886870797252 ) ) ;
#14562 =( BOUNDED_SURFACE ( )  B_SPLINE_SURFACE ( 3, 1, ( 
 ( #43107, #12582 ),
 ( #12820, #19977 ),
 ( #34979, #13286 ),
 ( #38925, #43606 ),
 ( #35222, #39416 ),
 ( #9864, #1247 ),
 ( #1497, #4967 ) ),
 .UNSPECIFIED., .T., .F., .F. ) 
 B_SPLINE_SURFACE_WITH_KNOTS ( ( 4, 3, 4 ),
 ( 2, 2 ),
 ( 0.000000000000000000, 0.5000000000000000000, 1.000000000000000000 ),
 ( 0.000000000000000000, 1.000000000000000000 ),
 .UNSPECIFIED. ) 
 GEOMETRIC_REPRESENTATION_ITEM ( )  RATIONAL_B_SPLINE_SURFACE ( (
 ( 1.000000000000000000, 1.000000000000000000),
 ( 0.3333333333333335369, 0.3333333333333330373),
 ( 0.3333333333333335369, 0.3333333333333330373),
 ( 1.000000000000000000, 1.000000000000000000),
 ( 0.3333333333333333703, 0.3333333333333333703),
 ( 0.3333333333333333703, 0.3333333333333333703),
 ( 1.000000000000000000, 1.000000000000000000) ) ) 
 REPRESENTATION_ITEM ( '' )  SURFACE ( )  );
#14563 = EDGE_LOOP ( 'NONE', ( #5362, #35544, #19797, #42840 ) ) ;
#14564 = CARTESIAN_POINT ( 'NONE',  ( -13.86248685510225087, -21.35271135026633971, 72.07607701462937655 ) ) ;
#14565 = CARTESIAN_POINT ( 'NONE',  ( -20.27409385541325904, -6.859212275519745106, 50.50378509014061734 ) ) ;
#14566 = ORIENTED_EDGE ( 'NONE', *, *, #26458, .F. ) ;
#14567 = CARTESIAN_POINT ( 'NONE',  ( -10.49754805884589004, -17.55449835891870691, 68.28377192865846723 ) ) ;
#14568 = FACE_OUTER_BOUND ( 'NONE', #23630, .T. ) ;
#14569 = CARTESIAN_POINT ( 'NONE',  ( -18.36159385541303735, -7.228003583438111335, 51.38655588711986866 ) ) ;
#14570 = ORIENTED_EDGE ( 'NONE', *, *, #23834, .T. ) ;
#14571 = CARTESIAN_POINT ( 'NONE',  ( -40.92409385541305511, -14.80920654474410725, 74.99999999999998579 ) ) ;
#14572 = ADVANCED_FACE ( 'NONE', ( #15413 ), #35880, .T. ) ;
#14573 = CARTESIAN_POINT ( 'NONE',  ( -15.65537882804863834, -7.980949930599003039, 67.34826994618644846 ) ) ;
#14574 =( BOUNDED_CURVE ( )  B_SPLINE_CURVE ( 3, ( #43601, #43098, #35216, #2464 ),
 .UNSPECIFIED., .F., .F. ) 
 B_SPLINE_CURVE_WITH_KNOTS ( ( 4, 4 ),
 ( 0.9074455897393672865, 1.000000000000000000 ),
 .UNSPECIFIED. ) 
 CURVE ( )  GEOMETRIC_REPRESENTATION_ITEM ( )  RATIONAL_B_SPLINE_CURVE ( ( 0.6983129098260870693, 0.7760317562606930952, 0.8765941196519974055, 1.000000000000000000 ) ) 
 REPRESENTATION_ITEM ( '' )  );
#14575 = CARTESIAN_POINT ( 'NONE',  ( -16.06050865347321732, -9.480920197610746669, 53.49899999999994549 ) ) ;
#14576 = PLANE ( 'NONE',  #2483 ) ;
#14577 = ORIENTED_EDGE ( 'NONE', *, *, #33178, .F. ) ;
#14578 = CARTESIAN_POINT ( 'NONE',  ( -10.78978130820344994, -12.42417047965500743, 57.62857332104950814 ) ) ;
#14579 = FACE_OUTER_BOUND ( 'NONE', #7780, .T. ) ;
#14580 = DIRECTION ( 'NONE',  ( 2.866981220435666553E-17, -1.000000000000000000, -1.190614954331866791E-16 ) ) ;
#14581 = DIRECTION ( 'NONE',  ( 3.395021121731789346E-32, 0.9999954153791273948, 0.003028072113822188795 ) ) ;
#14582 = CARTESIAN_POINT ( 'NONE',  ( -21.10164091802717223, -17.71419016815049119, 49.52966884056655772 ) ) ;
#14583 = ORIENTED_EDGE ( 'NONE', *, *, #6824, .T. ) ;
#14584 = EDGE_CURVE ( 'NONE', #30119, #5861, #39114, .T. ) ;
#14585 = CARTESIAN_POINT ( 'NONE',  ( -16.39155704513022016, -21.78318439201321866, 61.75568132354042206 ) ) ;
#14586 = FACE_OUTER_BOUND ( 'NONE', #35089, .T. ) ;
#14587 = ORIENTED_EDGE ( 'NONE', *, *, #12174, .F. ) ;
#14588 = DIRECTION ( 'NONE',  ( -3.071710424422018668E-17, 6.404604876783312462E-16, 1.000000000000000000 ) ) ;
#14589 = CARTESIAN_POINT ( 'NONE',  ( -21.76784385759799179, -9.357632978295825410, 49.97845033065682685 ) ) ;
#14590 = FACE_OUTER_BOUND ( 'NONE', #13077, .T. ) ;
#14591 = EDGE_LOOP ( 'NONE', ( #40204, #21928, #32220, #19763 ) ) ;
#14592 = CARTESIAN_POINT ( 'NONE',  ( -19.83743235192402210, -21.38007574497211039, 69.22777528876429187 ) ) ;
#14593 =( BOUNDED_CURVE ( )  B_SPLINE_CURVE ( 3, ( #38525, #7358, #26296, #22356 ),
 .UNSPECIFIED., .F., .F. ) 
 B_SPLINE_CURVE_WITH_KNOTS ( ( 4, 4 ),
 ( 0.4074455897393582937, 0.5000000000000000000 ),
 .UNSPECIFIED. ) 
 CURVE ( )  GEOMETRIC_REPRESENTATION_ITEM ( )  RATIONAL_B_SPLINE_CURVE ( ( 0.6983129098260915102, 0.7760317562606909858, 0.8765941196519919654, 0.9999999999999905631 ) ) 
 REPRESENTATION_ITEM ( '' )  );
#14594 = AXIS2_PLACEMENT_3D ( 'NONE', #7227, #33524, #41185 ) ;
#14595 = CARTESIAN_POINT ( 'NONE',  ( -10.20995793436087595, -16.92613924295324423, 54.02312124697527906 ) ) ;
#14596 = EDGE_LOOP ( 'NONE', ( #40615, #19259 ) ) ;
#14597 = VERTEX_POINT ( 'NONE', #4360 ) ;
#14598 = EDGE_LOOP ( 'NONE', ( #16598, #48083, #8516, #29399 ) ) ;
#14599 = CARTESIAN_POINT ( 'NONE',  ( -13.35534385650551492, -7.417179338643134834, 52.18511593390279302 ) ) ;
#14600 = CARTESIAN_POINT ( 'NONE',  ( -10.99586753834015695, -11.04334891231907534, 60.86381058728009208 ) ) ;
#14601 = CARTESIAN_POINT ( 'NONE',  ( -24.79676515827134153, -15.88070078827938048, 69.65590621464686194 ) ) ;
#14602 = LINE ( 'NONE', #23028, #47955 ) ;
#14603 = LINE ( 'NONE', #25975, #32294 ) ;
#14604 = ORIENTED_EDGE ( 'NONE', *, *, #2274, .T. ) ;
#14605 = ORIENTED_EDGE ( 'NONE', *, *, #47053, .F. ) ;
#14606 = CARTESIAN_POINT ( 'NONE',  ( -13.78034385650551563, -6.424090610841176385, 49.80797279389977916 ) ) ;
#14607 = EDGE_CURVE ( 'NONE', #34613, #37103, #5414, .T. ) ;
#14608 = CARTESIAN_POINT ( 'NONE',  ( -16.60134452727454146, -19.99433755013348346, 52.02966884056656482 ) ) ;
#14609 = CARTESIAN_POINT ( 'NONE',  ( -14.90534385650551918, -8.801233750844183135, 48.81488406609782515 ) ) ;
#14610 = EDGE_CURVE ( 'NONE', #40496, #6954, #32116, .T. ) ;
#14612 = ORIENTED_EDGE ( 'NONE', *, *, #46657, .T. ) ;
#14611 = EDGE_CURVE ( 'NONE', #1374, #29698, #8304, .T. ) ;
#14613 = B_SPLINE_CURVE_WITH_KNOTS ( 'NONE', 3,
 ( #31949, #39338, #9074, #31225 ),
 .UNSPECIFIED., .F., .F.,
 ( 4, 4 ),
 ( 0.001041996463600832314, 0.002493317452643608895 ),
 .UNSPECIFIED. ) ;
#14614 = CARTESIAN_POINT ( 'NONE',  ( -17.42409385541299471, -14.80920654474435594, 52.02966884056656482 ) ) ;
#14615 = ADVANCED_FACE ( 'NONE', ( #23570 ), #1630, .T. ) ;
#14616 = DIRECTION ( 'NONE',  ( -3.289814948237356682E-07, -7.277561423860909391E-07, 0.9999999999996810329 ) ) ;
#14617 = EDGE_CURVE ( 'NONE', #31313, #46311, #41477, .T. ) ;
#14618 = CARTESIAN_POINT ( 'NONE',  ( -24.40527833060663454, -14.29480840995819335, 69.95275285367253559 ) ) ;
#14619 = ORIENTED_EDGE ( 'NONE', *, *, #18953, .F. ) ;
#14620 = FACE_OUTER_BOUND ( 'NONE', #4494, .T. ) ;
#14621 = CIRCLE ( 'NONE', #23325, 4.686499999999999666 ) ;
#14622 = ORIENTED_EDGE ( 'NONE', *, *, #38306, .F. ) ;
#14623 = CARTESIAN_POINT ( 'NONE',  ( -22.14851325272248062, -9.572347091288939680, 60.13659902389549927 ) ) ;
#14624 = CARTESIAN_POINT ( 'NONE',  ( -18.15846822104387925, -21.77219406509840738, 69.00441818213361955 ) ) ;
#14625 = CARTESIAN_POINT ( 'NONE',  ( -24.41081920617251200, -17.39538559163089815, 69.51316173558434741 ) ) ;
#14626 = CARTESIAN_POINT ( 'NONE',  ( -10.42288197367123459, -12.26238041423571623, 57.43583165137763302 ) ) ;
#14627 = ADVANCED_FACE ( 'NONE', ( #19620 ), #32719, .T. ) ;
#14628 = ORIENTED_EDGE ( 'NONE', *, *, #37841, .F. ) ;
#14629 = CARTESIAN_POINT ( 'NONE',  ( -19.04074814492602030, -7.997133300950575396, 66.97242149538513445 ) ) ;
#14630 = CARTESIAN_POINT ( 'NONE',  ( -50.42409385541304800, -15.80920654474410725, 63.99999999999998579 ) ) ;
#14631 = CARTESIAN_POINT ( 'NONE',  ( -13.49145512112739631, -18.65424914341562612, 53.49899999999994549 ) ) ;
#14632 = DIRECTION ( 'NONE',  ( 0.5820088206811424580, -0.8131824719270213109, 7.019974882119936121E-08 ) ) ;
#14633 = ORIENTED_EDGE ( 'NONE', *, *, #46680, .F. ) ;
#14634 = DIRECTION ( 'NONE',  ( 0.9979768094191903138, 0.06357898915123821881, 0.000000000000000000 ) ) ;
#14635 = CARTESIAN_POINT ( 'NONE',  ( -17.13721359355439233, -7.364564939118506182, 70.62889357192571538 ) ) ;
#14636 = FACE_OUTER_BOUND ( 'NONE', #36534, .T. ) ;
#14637 = VERTEX_POINT ( 'NONE', #26172 ) ;
#14638 = FACE_BOUND ( 'NONE', #25582, .T. ) ;
#14639 = ORIENTED_EDGE ( 'NONE', *, *, #10008, .F. ) ;
#14640 = CARTESIAN_POINT ( 'NONE',  ( -18.31357888663955080, -21.80286911112441217, 69.11514702303101387 ) ) ;
#14641 = CARTESIAN_POINT ( 'NONE',  ( -23.44637151138313058, -19.19494152140299548, 62.50406877911783710 ) ) ;
#14642 = CARTESIAN_POINT ( 'NONE',  ( -13.89389072038462025, -21.36980434119256600, 72.11103101793651149 ) ) ;
#14643 = FACE_OUTER_BOUND ( 'NONE', #8204, .T. ) ;
#14644 = ORIENTED_EDGE ( 'NONE', *, *, #37407, .T. ) ;
#14645 = CARTESIAN_POINT ( 'NONE',  ( -17.42409385541306222, -14.80920654474411080, 75.49999999999998579 ) ) ;
#14646 = ORIENTED_EDGE ( 'NONE', *, *, #3727, .T. ) ;
#14647 = CARTESIAN_POINT ( 'NONE',  ( -10.16748990304072464, -13.12235252378331651, 71.39323974795351546 ) ) ;
#14648 = ORIENTED_EDGE ( 'NONE', *, *, #4316, .T. ) ;
#14649 = CARTESIAN_POINT ( 'NONE',  ( -16.09337498760136853, -22.13948385882417824, 58.40090183616962349 ) ) ;
#14650 = CARTESIAN_POINT ( 'NONE',  ( -13.52494119223468338, -20.62276537180227720, 58.27323320193088563 ) ) ;
#14651 = ORIENTED_EDGE ( 'NONE', *, *, #38747, .T. ) ;
#14652 = ORIENTED_EDGE ( 'NONE', *, *, #45455, .F. ) ;
#14653 = CARTESIAN_POINT ( 'NONE',  ( -15.56683366104601696, -8.060027224340267082, 70.68277797453286837 ) ) ;
#14654 = CARTESIAN_POINT ( 'NONE',  ( -22.24952110180534604, -19.88199308653408792, 69.24588173298749894 ) ) ;
#14655 = MANIFOLD_SOLID_BREP ( 'Stock-MAS-175-1', #9501 ) ;
#14656 = CARTESIAN_POINT ( 'NONE',  ( -26.42409385541305511, -8.109206544744111511, 51.75000000000000711 ) ) ;
#14657 = CARTESIAN_POINT ( 'NONE',  ( -10.58706256399181100, -13.30549982004886012, 74.96201107970274791 ) ) ;
#14658 = ADVANCED_FACE ( 'NONE', ( #45862 ), #30361, .T. ) ;
#14659 = CARTESIAN_POINT ( 'NONE',  ( -24.15187520166839974, -12.87586873588168324, 66.31749134914322497 ) ) ;
#14660 = CARTESIAN_POINT ( 'NONE',  ( -17.60291880755090332, -7.361353052781006490, 63.70057029387179881 ) ) ;
#14661 = CARTESIAN_POINT ( 'NONE',  ( -14.79254118299126119, -21.77901061722586817, 61.74262151019149059 ) ) ;
#14662 = CIRCLE ( 'NONE', #42232, 1.999999999999999112 ) ;
#14663 = VECTOR ( 'NONE', #1097, 1000.000000000000000 ) ;
#14664 = ORIENTED_EDGE ( 'NONE', *, *, #43440, .F. ) ;
#14665 = ORIENTED_EDGE ( 'NONE', *, *, #29316, .T. ) ;
#14666 = CARTESIAN_POINT ( 'NONE',  ( -17.25805186741143871, -7.753187986760909034, 63.70624286928425306 ) ) ;
#14667 = ADVANCED_FACE ( 'NONE', ( #16031 ), #27128, .T. ) ;
#14668 = DIRECTION ( 'NONE',  ( -3.071710424422018668E-17, 6.404604876783312462E-16, 1.000000000000000000 ) ) ;
#14669 = CARTESIAN_POINT ( 'NONE',  ( -21.92639021642452946, -9.447133411642054668, 63.30226860340928852 ) ) ;
#14670 = DIRECTION ( 'NONE',  ( 0.000000000000000000, 0.000000000000000000, 1.000000000000000000 ) ) ;
#14671 =( BOUNDED_CURVE ( )  B_SPLINE_CURVE ( 3, ( #4046, #8709, #19787, #34792 ),
 .UNSPECIFIED., .F., .F. ) 
 B_SPLINE_CURVE_WITH_KNOTS ( ( 4, 4 ),
 ( 0.5000000000000000000, 0.9074455897393621795 ),
 .UNSPECIFIED. ) 
 CURVE ( )  GEOMETRIC_REPRESENTATION_ITEM ( )  RATIONAL_B_SPLINE_CURVE ( ( 1.000000000000031530, 0.4567392136813390180, 0.3561768502900107825, 0.6983129098260809631 ) ) 
 REPRESENTATION_ITEM ( '' )  );
#14672 = CIRCLE ( 'NONE', #17078, 2.000000000000000000 ) ;
#14673 = DIRECTION ( 'NONE',  ( 0.3224496555704362000, 0.8691421305882578441, 0.3749909018349790180 ) ) ;
#14674 = ORIENTED_EDGE ( 'NONE', *, *, #3655, .T. ) ;
#14675 = CARTESIAN_POINT ( 'NONE',  ( -21.11784385650551954, -9.790100578890868377, 49.79778022625163203 ) ) ;
#14676 = ORIENTED_EDGE ( 'NONE', *, *, #23873, .T. ) ;
#14677 = LINE ( 'NONE', #29746, #8806 ) ;
#14678 = ADVANCED_FACE ( 'NONE', ( #19755 ), #1950, .T. ) ;
#14679 = CARTESIAN_POINT ( 'NONE',  ( -21.76886496386750736, -13.05243499865792067, 49.52966884056655772 ) ) ;
#14680 = ADVANCED_FACE ( 'NONE', ( #2996 ), #40198, .F. ) ;
#14681 = ORIENTED_EDGE ( 'NONE', *, *, #16181, .T. ) ;
#14682 = CARTESIAN_POINT ( 'NONE',  ( -22.92319755143357085, -10.39759026177046763, 63.37185995336191979 ) ) ;
#14683 = LINE ( 'NONE', #29754, #7590 ) ;
#14684 = ORIENTED_EDGE ( 'NONE', *, *, #12140, .T. ) ;
#14685 = CARTESIAN_POINT ( 'NONE',  ( -17.42409385541299471, -14.80920654474434883, 62.02966884056656482 ) ) ;
#14686 = EDGE_CURVE ( 'NONE', #28351, #38822, #20259, .T. ) ;
#14687 = FACE_OUTER_BOUND ( 'NONE', #45372, .T. ) ;
#14688 = EDGE_LOOP ( 'NONE', ( #35995, #36485 ) ) ;
#14689 = LINE ( 'NONE', #40829, #27524 ) ;
#14690 = AXIS2_PLACEMENT_3D ( 'NONE', #39898, #3434, #44336 ) ;
#14691 = AXIS2_PLACEMENT_3D ( 'NONE', #25934, #3769, #38208 ) ;
#14692 = ORIENTED_EDGE ( 'NONE', *, *, #38942, .T. ) ;
#14693 = DIRECTION ( 'NONE',  ( 1.404489475409085785E-08, -6.428047479010519175E-07, -0.9999999999997932765 ) ) ;
#14694 = CARTESIAN_POINT ( 'NONE',  ( -11.50075484580269070, -18.54176165173950253, 64.97537046917975090 ) ) ;
#14695 = ORIENTED_EDGE ( 'NONE', *, *, #36386, .F. ) ;
#14696 = CARTESIAN_POINT ( 'NONE',  ( -50.42409385541304800, -15.80920654474410725, 56.99999999999999289 ) ) ;
#14697 = CARTESIAN_POINT ( 'NONE',  ( -18.53556552080321751, -22.17591605216722428, 72.40015545304112266 ) ) ;
#14698 = ORIENTED_EDGE ( 'NONE', *, *, #25362, .F. ) ;
#14699 = CARTESIAN_POINT ( 'NONE',  ( -17.42409385541300892, -14.80920654474439679, 47.99999999999994316 ) ) ;
#14700 = AXIS2_PLACEMENT_3D ( 'NONE', #3782, #18793, #41439 ) ;
#14701 = CARTESIAN_POINT ( 'NONE',  ( -11.10837990474057158, -18.76092553618217451, 61.39898045628379464 ) ) ;
#14702 = CARTESIAN_POINT ( 'NONE',  ( -23.72641715273374530, -11.63183476396761407, 70.03643756225406491 ) ) ;
#14703 = EDGE_LOOP ( 'NONE', ( #27756, #6562, #29997, #7440, #39704 ) ) ;
#14704 = CARTESIAN_POINT ( 'NONE',  ( -19.89775169278732392, -21.83667719550688346, 69.11295222586642240 ) ) ;
#14705 = CARTESIAN_POINT ( 'NONE',  ( -40.92409385541306222, -14.90920654474428630, 74.99999999999998579 ) ) ;
#14706 = CARTESIAN_POINT ( 'NONE',  ( -23.29918339618657086, -19.39037464299967439, 58.99915238703562181 ) ) ;
#14707 = ORIENTED_EDGE ( 'NONE', *, *, #13951, .F. ) ;
#14708 = ORIENTED_EDGE ( 'NONE', *, *, #8917, .F. ) ;
#14709 = FACE_OUTER_BOUND ( 'NONE', #37777, .T. ) ;
#14710 = CARTESIAN_POINT ( 'NONE',  ( -16.87202378910036771, -7.830949141774897981, 74.18691624321796496 ) ) ;
#14711 = CARTESIAN_POINT ( 'NONE',  ( -23.46741908093438767, -19.16603997859080266, 62.53902161361033052 ) ) ;
#14712 = CARTESIAN_POINT ( 'NONE',  ( -14.17409385759798823, -6.859212275519751323, 50.50378509014259265 ) ) ;
#14713 = CARTESIAN_POINT ( 'NONE',  ( -22.79444606840252874, -10.23710104419528122, 62.95697184964878090 ) ) ;
#14714 =( BOUNDED_CURVE ( )  B_SPLINE_CURVE ( 3, ( #43380, #12356, #16035, #27376 ),
 .UNSPECIFIED., .F., .F. ) 
 B_SPLINE_CURVE_WITH_KNOTS ( ( 4, 4 ),
 ( 0.9074455897393653991, 1.000000000000000000 ),
 .UNSPECIFIED. ) 
 CURVE ( )  GEOMETRIC_REPRESENTATION_ITEM ( )  RATIONAL_B_SPLINE_CURVE ( ( 0.6983129098260982826, 0.7760317562607027542, 0.8765941196520032896, 1.000000000000000000 ) ) 
 REPRESENTATION_ITEM ( '' )  );
#14715 = EDGE_CURVE ( 'NONE', #44272, #43656, #17109, .T. ) ;
#14716 = FACE_OUTER_BOUND ( 'NONE', #45713, .T. ) ;
#14717 = CARTESIAN_POINT ( 'NONE',  ( -24.03783269458455862, -17.25936868619852760, 65.82868649746481537 ) ) ;
#14718 = DIRECTION ( 'NONE',  ( -3.071710424422018668E-17, 6.404604876783312462E-16, 1.000000000000000000 ) ) ;
#14719 = ORIENTED_EDGE ( 'NONE', *, *, #31494, .T. ) ;
#14720 = B_SPLINE_CURVE_WITH_KNOTS ( 'NONE', 3,
 ( #44683, #11188, #29903, #26203, #26693, #18549, #7751, #10938, #41214, #7503 ),
 .UNSPECIFIED., .F., .F.,
 ( 4, 2, 2, 2, 4 ),
 ( 0.1272669073658150574, 0.2522669073463055245, 0.3772669073267960194, 0.5022669073072865142, 0.6272669072877770091 ),
 .UNSPECIFIED. ) ;
#14721 = CARTESIAN_POINT ( 'NONE',  ( -24.72409385541305582, -15.80920654474410725, 65.99999999999998579 ) ) ;
#14722 = CARTESIAN_POINT ( 'NONE',  ( -18.26818317795011737, -21.80864274563727889, 68.82074505211160442 ) ) ;
#14723 = CYLINDRICAL_SURFACE ( 'NONE', #5600, 4.686499999999997002 ) ;
#14724 =( BOUNDED_CURVE ( )  B_SPLINE_CURVE ( 3, ( #36006, #33026, #47363, #29596 ),
 .UNSPECIFIED., .F., .F. ) 
 B_SPLINE_CURVE_WITH_KNOTS ( ( 4, 4 ),
 ( 4.712388980384690562, 4.921828490624009511 ),
 .UNSPECIFIED. ) 
 CURVE ( )  GEOMETRIC_REPRESENTATION_ITEM ( )  RATIONAL_B_SPLINE_CURVE ( ( 1.000000000000000000, 0.9963479302455156006, 0.9963479302455156006, 1.000000000000000000 ) ) 
 REPRESENTATION_ITEM ( '' )  );
#14725 = VECTOR ( 'NONE', #10560, 1000.000000000000000 ) ;
#14726 = ORIENTED_EDGE ( 'NONE', *, *, #1209, .T. ) ;
#14727 = VECTOR ( 'NONE', #1727, 1000.000000000000000 ) ;
#14728 = VERTEX_POINT ( 'NONE', #48295 ) ;
#14729 = CARTESIAN_POINT ( 'NONE',  ( -17.03007621496013968, -7.369466030635982712, 74.12164781354181287 ) ) ;
#14730 = DIRECTION ( 'NONE',  ( 3.071710424422018668E-17, -6.404604876783312462E-16, -1.000000000000000000 ) ) ;
#14731 = EDGE_CURVE ( 'NONE', #33555, #28685, #12302, .T. ) ;
#14732 = CARTESIAN_POINT ( 'NONE',  ( -13.35181980949104741, -21.04778605225073207, 61.70920450351935216 ) ) ;
#14733 = CARTESIAN_POINT ( 'NONE',  ( -10.18401502636761968, -13.05277926903019470, 71.32333192088977114 ) ) ;
#14734 = CIRCLE ( 'NONE', #17916, 1.350000000000004086 ) ;
#14735 = EDGE_CURVE ( 'NONE', #17705, #46048, #25536, .T. ) ;
#14736 = EDGE_LOOP ( 'NONE', ( #18470, #20370, #5418, #41506, #30709 ) ) ;
#14737 = B_SPLINE_CURVE_WITH_KNOTS ( 'NONE', 3,
 ( #6376, #2190, #32244, #28545, #24850, #2437, #32478, #21870, #14444, #11776 ),
 .UNSPECIFIED., .F., .F.,
 ( 4, 2, 2, 2, 4 ),
 ( 0.1272669073659020711, 0.2522669073463749134, 0.3772669073268477558, 0.5022669073073343649, 0.6272669072878209739 ),
 .UNSPECIFIED. ) ;
#14738 = DIRECTION ( 'NONE',  ( 2.866981220435666553E-17, -1.000000000000000000, -1.190614954331866791E-16 ) ) ;
#14739 = ADVANCED_FACE ( 'NONE', ( #43664 ), #12379, .F. ) ;
#14740 = DIRECTION ( 'NONE',  ( -0.9687793358424819923, 0.2479245821708680464, 0.000000000000000000 ) ) ;
#14741 = ORIENTED_EDGE ( 'NONE', *, *, #42366, .T. ) ;
#14742 = CARTESIAN_POINT ( 'NONE',  ( -22.14090652532222236, -20.04928072148792495, 62.51967078134249078 ) ) ;
#14743 = EDGE_CURVE ( 'NONE', #40402, #596, #35009, .T. ) ;
#14744 = CARTESIAN_POINT ( 'NONE',  ( -24.17271849214968071, -12.95015691860989371, 66.60246741689840633 ) ) ;
#14745 = DIRECTION ( 'NONE',  ( 0.6408936281290996684, 0.7676297007174210929, 4.260501105223829223E-08 ) ) ;
#14746 = ORIENTED_EDGE ( 'NONE', *, *, #5457, .F. ) ;
#14747 = CARTESIAN_POINT ( 'NONE',  ( -17.54761319933287211, -7.808689222983000278, 67.13112577798570157 ) ) ;
#14748 = ORIENTED_EDGE ( 'NONE', *, *, #11769, .T. ) ;
#14749 = CARTESIAN_POINT ( 'NONE',  ( -19.50997552649656086, -21.96132259753523996, 62.25149580216906742 ) ) ;
#14750 = DIRECTION ( 'NONE',  ( -0.8356905716187448263, 0.5492005722024784209, 7.728900804118606451E-08 ) ) ;
#14751 = ORIENTED_EDGE ( 'NONE', *, *, #8028, .T. ) ;
#14752 = CARTESIAN_POINT ( 'NONE',  ( -13.29676203468008033, -8.606078807347360637, 57.08312357396523140 ) ) ;
#14753 = LINE ( 'NONE', #41141, #5361 ) ;
#14754 = CARTESIAN_POINT ( 'NONE',  ( -20.13659385650551670, -6.915538690918075382, 49.31353937987644542 ) ) ;
#14755 = AXIS2_PLACEMENT_3D ( 'NONE', #25464, #11410, #44928 ) ;
#14756 = CARTESIAN_POINT ( 'NONE',  ( -14.32608993321936453, -8.532007372683787949, 67.48648493512258995 ) ) ;
#14757 = AXIS2_PLACEMENT_3D ( 'NONE', #18306, #33317, #33562 ) ;
#14758 = EDGE_CURVE ( 'NONE', #46590, #43248, #10719, .T. ) ;
#14759 = CARTESIAN_POINT ( 'NONE',  ( -24.26499744607890818, -17.75976858747020160, 62.65856309191605789 ) ) ;
#14760 = PLANE ( 'NONE',  #48106 ) ;
#14761 = CARTESIAN_POINT ( 'NONE',  ( -16.63294949632448905, -21.81482455919772789, 65.52004579927108807 ) ) ;
#14762 = ORIENTED_EDGE ( 'NONE', *, *, #15861, .F. ) ;
#14763 = CIRCLE ( 'NONE', #25039, 2.000000000000000888 ) ;
#14764 = EDGE_CURVE ( 'NONE', #35214, #22721, #3904, .T. ) ;
#14765 = CYLINDRICAL_SURFACE ( 'NONE', #25844, 1.999999999999999556 ) ;
#14766 = CARTESIAN_POINT ( 'NONE',  ( -14.41428173599358331, -7.994163662063686893, 63.97474278339937115 ) ) ;
#14767 = DIRECTION ( 'NONE',  ( 1.224646799147353207E-16, 1.000000000000000000, -1.912410701131276611E-32 ) ) ;
#14768 = DIRECTION ( 'NONE',  ( 0.9294853595766541243, 0.3688590060343629462, 0.000000000000000000 ) ) ;
#14769 = DIRECTION ( 'NONE',  ( -0.4780674886490096087, 0.8783231047267435754, 5.292596395488305015E-08 ) ) ;
#14770 = VERTEX_POINT ( 'NONE', #17760 ) ;
#14771 = ORIENTED_EDGE ( 'NONE', *, *, #19715, .T. ) ;
#14772 = LINE ( 'NONE', #44871, #31407 ) ;
#14773 = CARTESIAN_POINT ( 'NONE',  ( -14.98927377128279126, -8.246306944878790901, 56.84999999999994458 ) ) ;
#14774 = EDGE_LOOP ( 'NONE', ( #24661, #280 ) ) ;
#14776 = CARTESIAN_POINT ( 'NONE',  ( -24.05059673655033947, -17.06518960458298650, 73.18336032079744768 ) ) ;
#14775 = DIRECTION ( 'NONE',  ( -0.6323592902076723421, -0.7746752403995151859, 4.984538757074985308E-08 ) ) ;
#14777 = CARTESIAN_POINT ( 'NONE',  ( -11.32868395029271724, -18.25189577030657517, 57.82331260959011843 ) ) ;
#14778 = VECTOR ( 'NONE', #33604, 1000.000000000000000 ) ;
#14779 = CARTESIAN_POINT ( 'NONE',  ( -14.45498764112879186, -8.410827627250604621, 71.02957685130120069 ) ) ;
#14780 = CARTESIAN_POINT ( 'NONE',  ( -20.19053640067075506, -7.838066347919499854, 47.99999999999994316 ) ) ;
#14781 = EDGE_CURVE ( 'NONE', #6686, #9124, #47819, .T. ) ;
#14782 = CARTESIAN_POINT ( 'NONE',  ( -18.11889201384288128, -21.82488578508536747, 65.34532159284481168 ) ) ;
#14783 = PLANE ( 'NONE',  #7451 ) ;
#14784 = CARTESIAN_POINT ( 'NONE',  ( -11.46606301615817713, -19.28211147136272174, 71.84719208600056106 ) ) ;
#14785 = DIRECTION ( 'NONE',  ( -5.731567514496413899E-31, -1.020425574103664789E-16, -1.000000000000000000 ) ) ;
#14786 = ORIENTED_EDGE ( 'NONE', *, *, #40824, .T. ) ;
#14787 = CARTESIAN_POINT ( 'NONE',  ( -13.21312298333807611, -8.663458122980285836, 60.58950274328479679 ) ) ;
#14788 = CARTESIAN_POINT ( 'NONE',  ( -21.50272164136802999, -9.054240346128722194, 66.66149779378484652 ) ) ;
#14789 = CARTESIAN_POINT ( 'NONE',  ( -12.07145959968993409, -19.99109779731879399, 61.49704379391130260 ) ) ;
#14790 = CYLINDRICAL_SURFACE ( 'NONE', #44488, 0.1500000000000054068 ) ;
#14791 = FACE_OUTER_BOUND ( 'NONE', #10240, .T. ) ;
#14792 = CARTESIAN_POINT ( 'NONE',  ( -14.53767063111817137, -21.24453063237525541, 58.58106478802027084 ) ) ;
#14793 = CARTESIAN_POINT ( 'NONE',  ( -23.35641471936834535, -10.99444570894131168, 73.24704464419542660 ) ) ;
#14794 = ORIENTED_EDGE ( 'NONE', *, *, #47350, .T. ) ;
#14795 = VERTEX_POINT ( 'NONE', #29105 ) ;
#14796 = CARTESIAN_POINT ( 'NONE',  ( -14.59284385541304729, -8.630756214087126565, 51.74842643355248129 ) ) ;
#14797 = ORIENTED_EDGE ( 'NONE', *, *, #14895, .T. ) ;
#14798 = CARTESIAN_POINT ( 'NONE',  ( -22.92319839529956838, -10.39759132684999265, 63.22185995336808162 ) ) ;
#14799 = VECTOR ( 'NONE', #23236, 1000.000000000000000 ) ;
#14800 = DIRECTION ( 'NONE',  ( -3.071710424422018668E-17, 6.404604876783312462E-16, 1.000000000000000000 ) ) ;
#14801 = TOROIDAL_SURFACE ( 'NONE', #42370, 1.899999999999999911, 0.1000000000000000056 ) ;
#14802 = AXIS2_PLACEMENT_3D ( 'NONE', #20084, #12448, #31167 ) ;
#14803 = AXIS2_PLACEMENT_3D ( 'NONE', #17339, #32383, #39280 ) ;
#14804 = EDGE_CURVE ( 'NONE', #14479, #28111, #16299, .T. ) ;
#14805 = CARTESIAN_POINT ( 'NONE',  ( -24.61605457543312525, -12.86511826566283290, 66.41751344402152313 ) ) ;
#14806 = CARTESIAN_POINT ( 'NONE',  ( -15.61361955732275497, -7.582487114453736687, 70.71715703711943490 ) ) ;
#14807 = VERTEX_POINT ( 'NONE', #39866 ) ;
#14808 = EDGE_CURVE ( 'NONE', #43944, #28462, #19211, .T. ) ;
#14809 = CARTESIAN_POINT ( 'NONE',  ( -15.95707209241614422, -7.504986913482371236, 63.85506412386598640 ) ) ;
#14810 = AXIS2_PLACEMENT_3D ( 'NONE', #12375, #5239, #4758 ) ;
#14811 = CARTESIAN_POINT ( 'NONE',  ( -22.05923648098858791, -20.05472392750071720, 62.23439162613904330 ) ) ;
#14812 = VERTEX_POINT ( 'NONE', #35917 ) ;
#14813 = CARTESIAN_POINT ( 'NONE',  ( -13.11946129443726861, -9.225960368241006293, 67.37942785707224402 ) ) ;
#14814 = CARTESIAN_POINT ( 'NONE',  ( -41.41379973776600565, -14.80920654474410725, 71.08235294117645253 ) ) ;
#14815 = ORIENTED_EDGE ( 'NONE', *, *, #19160, .F. ) ;
#14816 = CARTESIAN_POINT ( 'NONE',  ( -18.34560609025200861, -9.386954687716539070, 53.49899999999994549 ) ) ;
#14817 = DIRECTION ( 'NONE',  ( -3.071710424422018668E-17, 6.404604876783312462E-16, 1.000000000000000000 ) ) ;
#14818 = CARTESIAN_POINT ( 'NONE',  ( -23.29871437377730814, -10.22635856038569990, 59.71548043103533843 ) ) ;
#14819 = ORIENTED_EDGE ( 'NONE', *, *, #18402, .F. ) ;
#14820 = CARTESIAN_POINT ( 'NONE',  ( -20.03282965983824226, -21.84088468745754597, 47.99999999999994316 ) ) ;
#14821 = CARTESIAN_POINT ( 'NONE',  ( -23.52949419687348964, -11.28347464189849525, 70.17738639980606763 ) ) ;
#14822 = EDGE_CURVE ( 'NONE', #19035, #9708, #37762, .T. ) ;
#14823 = CARTESIAN_POINT ( 'NONE',  ( -46.48018488037470064, -16.43194983366065642, 70.50000000000000000 ) ) ;
#14824 = CARTESIAN_POINT ( 'NONE',  ( -21.39310587431502242, -21.11392247816499435, 69.20450181858771543 ) ) ;
#14825 = VERTEX_POINT ( 'NONE', #2197 ) ;
#14826 = CARTESIAN_POINT ( 'NONE',  ( -11.88016137193916677, -19.16921147633432199, 71.57197012879584008 ) ) ;
#14827 = DIRECTION ( 'NONE',  ( -0.5022914217388751990, 0.8646984027090225400, 6.766381827299041184E-08 ) ) ;
#14828 = DIRECTION ( 'NONE',  ( -3.071710424422018668E-17, 6.404604876783312462E-16, 1.000000000000000000 ) ) ;
#14829 = ADVANCED_FACE ( 'NONE', ( #29275 ), #28552, .T. ) ;
#14830 = CARTESIAN_POINT ( 'NONE',  ( 10.57590614458695377, -0.1092432217106413528, 50.52422457691089619 ) ) ;
#14831 = EDGE_CURVE ( 'NONE', #9420, #11732, #44075, .T. ) ;
#14832 = EDGE_CURVE ( 'NONE', #24815, #5348, #17331, .T. ) ;
#14833 = CARTESIAN_POINT ( 'NONE',  ( -20.44284385650551883, -8.811426318492348031, 52.18089403414751359 ) ) ;
#14834 = EDGE_CURVE ( 'NONE', #32811, #17454, #42301, .T. ) ;
#14835 = ORIENTED_EDGE ( 'NONE', *, *, #45969, .F. ) ;
#14836 = AXIS2_PLACEMENT_3D ( 'NONE', #34673, #30026, #41332 ) ;
#14837 = CARTESIAN_POINT ( 'NONE',  ( -16.22958052549516950, -7.455513305798441515, 60.45674424308347739 ) ) ;
#14838 = CARTESIAN_POINT ( 'NONE',  ( -45.37196614242555626, -14.20920654474410760, 70.43449436244726769 ) ) ;
#14839 = ORIENTED_EDGE ( 'NONE', *, *, #32782, .F. ) ;
#14840 = CARTESIAN_POINT ( 'NONE',  ( -22.53429319464571279, -9.952421322533329118, 73.48161091678163359 ) ) ;
#14841 = CARTESIAN_POINT ( 'NONE',  ( -17.42409385541299471, -14.80920654474435771, 49.52966884056655772 ) ) ;
#14842 = ORIENTED_EDGE ( 'NONE', *, *, #34978, .T. ) ;
#14843 = B_SPLINE_CURVE_WITH_KNOTS ( 'NONE', 3,
 ( #1773, #46353, #27866, #42665, #1274, #46103, #35493, #20238, #12363, #27384 ),
 .UNSPECIFIED., .F., .F.,
 ( 4, 2, 2, 2, 4 ),
 ( 0.000000000000000000, 0.2500000000000000000, 0.5000000000000000000, 0.7500000000000000000, 1.000000000000000000 ),
 .UNSPECIFIED. ) ;
#14844 = CARTESIAN_POINT ( 'NONE',  ( -23.56138519289638822, -11.33989039198723070, 69.89210750373884196 ) ) ;
#14845 = VECTOR ( 'NONE', #33748, 1000.000000000000000 ) ;
#14846 = AXIS2_PLACEMENT_3D ( 'NONE', #19232, #34233, #15508 ) ;
#14847 = CARTESIAN_POINT ( 'NONE',  ( -14.58623519113625200, -21.69754534531507772, 58.26594266842833036 ) ) ;
#14848 = ORIENTED_EDGE ( 'NONE', *, *, #13890, .T. ) ;
#14849 = VERTEX_POINT ( 'NONE', #21163 ) ;
#14850 = CARTESIAN_POINT ( 'NONE',  ( -14.03034385650551563, -9.794322478646142471, 51.19202720610083901 ) ) ;
#14851 = VECTOR ( 'NONE', #44744, 1000.000000000000000 ) ;
#14852 = CARTESIAN_POINT ( 'NONE',  ( -11.47236213698566054, -10.32806074475630886, 74.55389686390628867 ) ) ;
#14853 = LINE ( 'NONE', #48617, #22978 ) ;
#14854 = DIRECTION ( 'NONE',  ( -3.071710424422018668E-17, 6.404604876783312462E-16, 1.000000000000000000 ) ) ;
#14855 = CARTESIAN_POINT ( 'NONE',  ( -21.15825550006504940, -20.79330918033647535, 72.61626714470398269 ) ) ;
#14856 = EDGE_LOOP ( 'NONE', ( #29972, #27815 ) ) ;
#14857 = ORIENTED_EDGE ( 'NONE', *, *, #4048, .F. ) ;
#14858 = CARTESIAN_POINT ( 'NONE',  ( -13.55534385650551243, -7.417179338643134834, 52.18511593390279302 ) ) ;
#14859 = EDGE_CURVE ( 'NONE', #34680, #16467, #40931, .T. ) ;
#14860 = FACE_OUTER_BOUND ( 'NONE', #21452, .T. ) ;
#14861 = CARTESIAN_POINT ( 'NONE',  ( -10.84048750645423098, -17.18764830010450595, 61.44277775138327513 ) ) ;
#14862 =( BOUNDED_CURVE ( )  B_SPLINE_CURVE ( 3, ( #44632, #15050, #11376, #18506 ),
 .UNSPECIFIED., .F., .F. ) 
 B_SPLINE_CURVE_WITH_KNOTS ( ( 4, 4 ),
 ( 0.9074455897393705062, 1.000000000000000000 ),
 .UNSPECIFIED. ) 
 CURVE ( )  GEOMETRIC_REPRESENTATION_ITEM ( )  RATIONAL_B_SPLINE_CURVE ( ( 0.6983129098261057210, 0.7760317562607091935, 0.8765941196520072864, 1.000000000000000000 ) ) 
 REPRESENTATION_ITEM ( '' )  );
#14863 = B_SPLINE_CURVE_WITH_KNOTS ( 'NONE', 1,
 ( #26696, #25960 ),
 .UNSPECIFIED., .F., .F.,
 ( 2, 2 ),
 ( 0.000000000000000000, 1.000000000000000000 ),
 .UNSPECIFIED. ) ;
#14864 = CARTESIAN_POINT ( 'NONE',  ( -14.62409385650551386, -6.426201560718813433, 50.50509628382439331 ) ) ;
#14865 = VERTEX_POINT ( 'NONE', #36397 ) ;
#14866 = CARTESIAN_POINT ( 'NONE',  ( -15.53265176333180619, -21.60105060138385369, 72.33103357390284316 ) ) ;
#14867 = AXIS2_PLACEMENT_3D ( 'NONE', #8496, #23524, #4806 ) ;
#14868 = PLANE ( 'NONE',  #1658 ) ;
#14869 = FACE_OUTER_BOUND ( 'NONE', #22913, .T. ) ;
#14870 = ORIENTED_EDGE ( 'NONE', *, *, #28419, .F. ) ;
#14871 =( BOUNDED_CURVE ( )  B_SPLINE_CURVE ( 3, ( #26232, #15616, #15131, #30188 ),
 .UNSPECIFIED., .F., .F. ) 
 B_SPLINE_CURVE_WITH_KNOTS ( ( 4, 4 ),
 ( 0.5000000000000000000, 0.9074455897393693959 ),
 .UNSPECIFIED. ) 
 CURVE ( )  GEOMETRIC_REPRESENTATION_ITEM ( )  RATIONAL_B_SPLINE_CURVE ( ( 1.000000000000009992, 0.4567392136813236414, 0.3561768502900199418, 0.6983129098261101619 ) ) 
 REPRESENTATION_ITEM ( '' )  );
#14872 = CARTESIAN_POINT ( 'NONE',  ( -23.00382247466728103, -19.03821840904449303, 62.42577227956508068 ) ) ;
#14873 =( BOUNDED_CURVE ( )  B_SPLINE_CURVE ( 3, ( #32342, #20282, #35285, #31610 ),
 .UNSPECIFIED., .F., .F. ) 
 B_SPLINE_CURVE_WITH_KNOTS ( ( 4, 4 ),
 ( 0.9074455897393675086, 1.000000000000000000 ),
 .UNSPECIFIED. ) 
 CURVE ( )  GEOMETRIC_REPRESENTATION_ITEM ( )  RATIONAL_B_SPLINE_CURVE ( ( 0.6983129098261082746, 0.7760317562607114139, 0.8765941196520086187, 1.000000000000000000 ) ) 
 REPRESENTATION_ITEM ( '' )  );
#14874 = CIRCLE ( 'NONE', #38496, 1.049999999999998934 ) ;
#14875 = ORIENTED_EDGE ( 'NONE', *, *, #19882, .F. ) ;
#14876 = FACE_OUTER_BOUND ( 'NONE', #23659, .T. ) ;
#14877 = CYLINDRICAL_SURFACE ( 'NONE', #13164, 0.1500000000000028255 ) ;
#14878 = CARTESIAN_POINT ( 'NONE',  ( -18.52415950777489684, -7.896185818571675341, 74.14064402152244782 ) ) ;
#14879 = CARTESIAN_POINT ( 'NONE',  ( -21.53861794036900079, -21.02004141303368101, 72.63951040967180006 ) ) ;
#14880 = B_SPLINE_CURVE_WITH_KNOTS ( 'NONE', 3,
 ( #19829, #4551, #8987, #19575, #15866, #38524, #16346, #31138, #16831, #46415 ),
 .UNSPECIFIED., .F., .F.,
 ( 4, 2, 2, 2, 4 ),
 ( 0.000000000000000000, 0.2500000000000000000, 0.5000000000000000000, 0.7500000000000000000, 1.000000000000000000 ),
 .UNSPECIFIED. ) ;
#14881 = ORIENTED_EDGE ( 'NONE', *, *, #24428, .F. ) ;
#14882 = CARTESIAN_POINT ( 'NONE',  ( -10.42477179210370686, -17.36325313327283482, 61.27087820301521504 ) ) ;
#14883 = AXIS2_PLACEMENT_3D ( 'NONE', #25118, #47033, #6158 ) ;
#14884 = CARTESIAN_POINT ( 'NONE',  ( -24.21474372977315070, -11.74455924407879337, 59.64382217289720955 ) ) ;
#14885 = CARTESIAN_POINT ( 'NONE',  ( -13.18904211892902367, -11.30002761096173280, 54.07175714974879099 ) ) ;
#14886 = DIRECTION ( 'NONE',  ( 9.352133743349324758E-06, 6.779811746737758835E-06, 0.9999999999332858103 ) ) ;
#14887 = ORIENTED_EDGE ( 'NONE', *, *, #25495, .T. ) ;
#14888 = CARTESIAN_POINT ( 'NONE',  ( -10.54823608622644038, -17.67727527167151536, 68.20383655110275356 ) ) ;
#14889 = CARTESIAN_POINT ( 'NONE',  ( -18.46649413407774887, -22.18667672369172550, 72.47166315949273496 ) ) ;
#14891 =( BOUNDED_SURFACE ( )  B_SPLINE_SURFACE ( 3, 1, ( 
 ( #9197, #39224 ),
 ( #13102, #36700 ),
 ( #25898, #44159 ),
 ( #29845, #40911 ),
 ( #14299, #10408 ),
 ( #33018, #48538 ),
 ( #25417, #29589 ) ),
 .UNSPECIFIED., .T., .F., .F. ) 
 B_SPLINE_SURFACE_WITH_KNOTS ( ( 4, 3, 4 ),
 ( 2, 2 ),
 ( 0.000000000000000000, 0.5000000000000000000, 1.000000000000000000 ),
 ( 0.000000000000000000, 1.000000000000000000 ),
 .UNSPECIFIED. ) 
 GEOMETRIC_REPRESENTATION_ITEM ( )  RATIONAL_B_SPLINE_SURFACE ( (
 ( 1.000000000000000000, 1.000000000000000000),
 ( 0.3333333333333335369, 0.3333333333333330373),
 ( 0.3333333333333335369, 0.3333333333333330373),
 ( 1.000000000000000000, 1.000000000000000000),
 ( 0.3333333333333333703, 0.3333333333333333703),
 ( 0.3333333333333333703, 0.3333333333333333703),
 ( 1.000000000000000000, 1.000000000000000000) ) ) 
 REPRESENTATION_ITEM ( '' )  SURFACE ( )  );
#14890 = CARTESIAN_POINT ( 'NONE',  ( -18.66311988809301425, -7.868636481342422329, 70.65595886192740238 ) ) ;
#14892 = FACE_BOUND ( 'NONE', #13153, .T. ) ;
#14893 = ORIENTED_EDGE ( 'NONE', *, *, #15928, .T. ) ;
#14894 = EDGE_CURVE ( 'NONE', #30011, #42667, #2677, .T. ) ;
#14895 = EDGE_CURVE ( 'NONE', #26989, #19312, #6124, .T. ) ;
#14896 = DIRECTION ( 'NONE',  ( -0.9729319276368276759, -0.2310918955413239773, 6.827553174175007530E-08 ) ) ;
#14897 = CARTESIAN_POINT ( 'NONE',  ( -10.53619943228106948, -16.06595316453636713, 71.55823587554787935 ) ) ;
#14898 = CARTESIAN_POINT ( 'NONE',  ( -24.41706613368967282, -14.49561630978402071, 62.90399773248653048 ) ) ;
#14899 = CARTESIAN_POINT ( 'NONE',  ( -14.76159385541304658, -7.228003583438121993, 51.38655588711985445 ) ) ;
#14900 = ORIENTED_EDGE ( 'NONE', *, *, #28654, .T. ) ;
#14901 = CARTESIAN_POINT ( 'NONE',  ( -10.44202778021669609, -14.30845378979165794, 64.68803863533310050 ) ) ;
#14902 = EDGE_LOOP ( 'NONE', ( #43587, #20091, #20202, #19544, #11265 ) ) ;
#14903 = FACE_OUTER_BOUND ( 'NONE', #47600, .T. ) ;
#14904 = CYLINDRICAL_SURFACE ( 'NONE', #4660, 1.249999999999998668 ) ;
#14905 = DIRECTION ( 'NONE',  ( -3.071710424422018668E-17, 6.404604876783312462E-16, 1.000000000000000000 ) ) ;
#14906 = B_SPLINE_CURVE_WITH_KNOTS ( 'NONE', 1,
 ( #11105, #30563 ),
 .UNSPECIFIED., .F., .F.,
 ( 2, 2 ),
 ( 0.000000000000000000, 1.000000000000000000 ),
 .UNSPECIFIED. ) ;
#14907 = ORIENTED_EDGE ( 'NONE', *, *, #23883, .F. ) ;
#14908 = CARTESIAN_POINT ( 'NONE',  ( -12.70616753690738143, -9.559812705026583757, 71.00492334522255078 ) ) ;
#14909 = EDGE_CURVE ( 'NONE', #26571, #24126, #3164, .T. ) ;
#14910 = EDGE_CURVE ( 'NONE', #31125, #1137, #24261, .T. ) ;
#14911 = DIRECTION ( 'NONE',  ( -3.071710424422018668E-17, 6.404604876783312462E-16, 1.000000000000000000 ) ) ;
#14912 = ORIENTED_EDGE ( 'NONE', *, *, #15456, .F. ) ;
#14913 = ORIENTED_EDGE ( 'NONE', *, *, #18392, .F. ) ;
#14914 = EDGE_LOOP ( 'NONE', ( #41194, #25932, #43235, #14126 ) ) ;
#14915 = CARTESIAN_POINT ( 'NONE',  ( -15.53265176333180619, -21.60105060138385369, 72.33103357390284316 ) ) ;
#14917 = CARTESIAN_POINT ( 'NONE',  ( -22.31677908589231762, -19.81551989533932101, 69.47417984703402283 ) ) ;
#14916 = AXIS2_PLACEMENT_3D ( 'NONE', #44358, #47328, #47560 ) ;
#14918 = VECTOR ( 'NONE', #18044, 1000.000000000000000 ) ;
#14919 = CARTESIAN_POINT ( 'NONE',  ( -12.56171917241870695, -20.45376946399996854, 71.99148991968543498 ) ) ;
#14920 = DIRECTION ( 'NONE',  ( -5.731567514496413899E-31, -1.020425574103664789E-16, -1.000000000000000000 ) ) ;
#14921 = CARTESIAN_POINT ( 'NONE',  ( -24.22725865585316285, -12.95987763975231388, 66.30246766143382331 ) ) ;
#14922 = DIRECTION ( 'NONE',  ( 3.413470714839332458E-33, -1.190614954331866791E-16, 1.000000000000000000 ) ) ;
#14923 = CARTESIAN_POINT ( 'NONE',  ( -20.27409385541325904, -6.859212275519745106, 50.50378509014061734 ) ) ;
#14924 = EDGE_LOOP ( 'NONE', ( #28318, #31214, #41611, #23702, #38977 ) ) ;
#14925 = VERTEX_POINT ( 'NONE', #6863 ) ;
#14926 = CARTESIAN_POINT ( 'NONE',  ( -16.30010877417799264, -7.443724743308521852, 60.38683862147721726 ) ) ;
#14927 = EDGE_CURVE ( 'NONE', #2344, #40137, #19201, .T. ) ;
#14928 = CARTESIAN_POINT ( 'NONE',  ( -13.92949766901237041, -8.229479445867253773, 74.33921261090144128 ) ) ;
#14929 = CARTESIAN_POINT ( 'NONE',  ( -14.93209738089114857, -21.40413054883831734, 61.93600443765902241 ) ) ;
#14930 = AXIS2_PLACEMENT_3D ( 'NONE', #16569, #42932, #46140 ) ;
#14931 = CARTESIAN_POINT ( 'NONE',  ( -15.59410181515468530, -19.12364873146922051, 49.52966884056656482 ) ) ;
#14932 = ORIENTED_EDGE ( 'NONE', *, *, #5805, .T. ) ;
#14933 = CARTESIAN_POINT ( 'NONE',  ( -14.93034385650551599, -9.794322478646142471, 51.19202720610083901 ) ) ;
#14934 = ORIENTED_EDGE ( 'NONE', *, *, #36083, .T. ) ;
#14935 = CARTESIAN_POINT ( 'NONE',  ( -10.61946413101933295, -12.96527513164080148, 67.73832368323806463 ) ) ;
#14936 = FACE_OUTER_BOUND ( 'NONE', #28589, .T. ) ;
#14937 = CLOSED_SHELL ( 'NONE', ( #4277, #28164, #24746, #10189, #21404, #37042, #42174 ) ) ;
#14938 = CARTESIAN_POINT ( 'NONE',  ( -10.39215600595210454, -14.30487551902977650, 64.38803863383273551 ) ) ;
#14939 = ORIENTED_EDGE ( 'NONE', *, *, #45087, .F. ) ;
#14940 = CARTESIAN_POINT ( 'NONE',  ( -22.51786048828498465, -9.935131201570847281, 73.78161090940139388 ) ) ;
#14941 = B_SPLINE_CURVE_WITH_KNOTS ( 'NONE', 3,
 ( #32463, #11271, #26284, #48435, #14669, #6601, #40558, #18145, #11022, #40328 ),
 .UNSPECIFIED., .F., .F.,
 ( 4, 2, 2, 2, 4 ),
 ( 0.000000000000000000, 0.2500000000000000000, 0.5000000000000000000, 0.7500000000000000000, 1.000000000000000000 ),
 .UNSPECIFIED. ) ;
#14942 = CARTESIAN_POINT ( 'NONE',  ( -10.47274630608271373, -15.98537029978553825, 67.98327651004974825 ) ) ;
#14943 = FACE_OUTER_BOUND ( 'NONE', #21851, .T. ) ;
#14944 = AXIS2_PLACEMENT_3D ( 'NONE', #14157, #40524, #47680 ) ;
#14945 = VERTEX_POINT ( 'NONE', #47508 ) ;
#14946 = CARTESIAN_POINT ( 'NONE',  ( -10.40245588357037043, -14.17414831712846990, 61.20349182037644198 ) ) ;
#14947 = CARTESIAN_POINT ( 'NONE',  ( -10.45859239952313224, -15.89938452881993847, 64.79299464097340433 ) ) ;
#14948 = DIRECTION ( 'NONE',  ( 1.000000000000000000, 1.669677910507523057E-21, 6.493791346278465266E-22 ) ) ;
#14949 = VERTEX_POINT ( 'NONE', #47269 ) ;
#14950 = CARTESIAN_POINT ( 'NONE',  ( -20.72713954719890239, -8.131453259470875494, 63.46121511881940336 ) ) ;
#14951 = VECTOR ( 'NONE', #31915, 1000.000000000000000 ) ;
#14952 = ORIENTED_EDGE ( 'NONE', *, *, #25894, .T. ) ;
#14953 = CARTESIAN_POINT ( 'NONE',  ( -24.47401588439614528, -14.84236418521736312, 59.54300237059217693 ) ) ;
#14954 = CARTESIAN_POINT ( 'NONE',  ( -11.53125380103513109, -18.58817033051094825, 64.76323772856727601 ) ) ;
#14955 = ORIENTED_EDGE ( 'NONE', *, *, #4931, .T. ) ;
#14956 = ADVANCED_FACE ( 'NONE', ( #13740 ), #28785, .T. ) ;
#14957 = LINE ( 'NONE', #41326, #48619 ) ;
#14958 = CARTESIAN_POINT ( 'NONE',  ( -23.34288396506439867, -19.33377296368179543, 59.06906041190286771 ) ) ;
#14959 = ORIENTED_EDGE ( 'NONE', *, *, #17663, .T. ) ;
#14960 = DIRECTION ( 'NONE',  ( -3.811252426750347363E-06, -6.838859004669815670E-06, -0.9999999999693520714 ) ) ;
#14961 = AXIS2_PLACEMENT_3D ( 'NONE', #27247, #15908, #41542 ) ;
#14962 = CARTESIAN_POINT ( 'NONE',  ( -10.90274299180159012, -17.35673364766031668, 68.32551725290736044 ) ) ;
#14963 = VERTEX_POINT ( 'NONE', #14452 ) ;
#14964 = CARTESIAN_POINT ( 'NONE',  ( -12.10369346210734243, -9.594120923840563364, 57.27430859790474926 ) ) ;
#14965 = ADVANCED_FACE ( 'NONE', ( #24623 ), #45047, .T. ) ;
#14966 = CARTESIAN_POINT ( 'NONE',  ( -21.80081500731019872, -8.780166552249799139, 70.27099206861544189 ) ) ;
#14967 = CARTESIAN_POINT ( 'NONE',  ( -30.42409385541305156, -6.859206544744110623, 50.50000000000000000 ) ) ;
#14969 = EDGE_LOOP ( 'NONE', ( #457, #40292 ) ) ;
#14968 = TOROIDAL_SURFACE ( 'NONE', #1643, 1.700000000000000178, 0.2500000000000000000 ) ;
#14970 = ORIENTED_EDGE ( 'NONE', *, *, #38701, .T. ) ;
#14971 = ADVANCED_FACE ( 'NONE', ( #45527 ), #41084, .T. ) ;
#14972 = CARTESIAN_POINT ( 'NONE',  ( -23.35559249269254423, -10.30144050037046810, 59.80192198407322479 ) ) ;
#14973 = DIRECTION ( 'NONE',  ( -0.9687793358424819923, 0.2479245821708680464, 0.000000000000000000 ) ) ;
#14974 = LINE ( 'NONE', #37381, #2882 ) ;
#14975 = CARTESIAN_POINT ( 'NONE',  ( -45.55409385541305767, -14.20920654474410760, 69.94787228701220272 ) ) ;
#14976 =( BOUNDED_CURVE ( )  B_SPLINE_CURVE ( 3, ( #8464, #37761, #41716, #16313 ),
 .UNSPECIFIED., .F., .F. ) 
 B_SPLINE_CURVE_WITH_KNOTS ( ( 4, 4 ),
 ( 4.712388980384690562, 4.921828490624009511 ),
 .UNSPECIFIED. ) 
 CURVE ( )  GEOMETRIC_REPRESENTATION_ITEM ( )  RATIONAL_B_SPLINE_CURVE ( ( 1.000000000000000000, 0.9963479302455156006, 0.9963479302455156006, 1.000000000000000000 ) ) 
 REPRESENTATION_ITEM ( '' )  );
#14977 = CARTESIAN_POINT ( 'NONE',  ( -14.06159385759798930, -7.228003583438117552, 51.38655588711986155 ) ) ;
#14978 = ADVANCED_FACE ( 'NONE', ( #26551 ), #3913, .T. ) ;
#14979 = CARTESIAN_POINT ( 'NONE',  ( -10.40218298486903592, -14.14017159955334435, 57.44824790076416576 ) ) ;
#14980 = CARTESIAN_POINT ( 'NONE',  ( -12.40319033546273531, -19.76959921888892424, 68.48090162751329046 ) ) ;
#14981 = CARTESIAN_POINT ( 'NONE',  ( -17.36767326789754406, -7.755820026086070129, 63.75877036558070898 ) ) ;
#14982 = CARTESIAN_POINT ( 'NONE',  ( -13.54822921233619226, -20.69819393533649077, 61.51646323540209949 ) ) ;
#14983 = ORIENTED_EDGE ( 'NONE', *, *, #26597, .T. ) ;
#14984 = VECTOR ( 'NONE', #33398, 1000.000000000000000 ) ;
#14985 = B_SPLINE_CURVE_WITH_KNOTS ( 'NONE', 3,
 ( #12054, #38135, #22910, #45801, #30781, #731, #15724, #3, #11560, #4667 ),
 .UNSPECIFIED., .F., .F.,
 ( 4, 2, 2, 2, 4 ),
 ( 0.6272669072877804508, 0.7522669073072891788, 0.8772669073267977957, 1.002266907346306635, 1.127266907365815252 ),
 .UNSPECIFIED. ) ;
#14986 = CIRCLE ( 'NONE', #38630, 2.000000000000001332 ) ;
#14987 = DIRECTION ( 'NONE',  ( 3.549360974554993999E-17, -6.371834667797928663E-18, -1.000000000000000000 ) ) ;
#14988 = DIRECTION ( 'NONE',  ( -0.6538427738826437796, -0.7566304428460742804, 5.916677973164435741E-08 ) ) ;
#14989 = AXIS2_PLACEMENT_3D ( 'NONE', #8553, #46220, #39312 ) ;
#14990 = ORIENTED_EDGE ( 'NONE', *, *, #35650, .T. ) ;
#14991 = ORIENTED_EDGE ( 'NONE', *, *, #32466, .T. ) ;
#14992 = DIRECTION ( 'NONE',  ( 1.000000000000000000, -4.164305804376849172E-17, 1.614929280266638808E-16 ) ) ;
#14993 = CARTESIAN_POINT ( 'NONE',  ( -10.64823551202976937, -13.04561788836951308, 71.39755745898455075 ) ) ;
#14994 = CARTESIAN_POINT ( 'NONE',  ( -21.79028809537168243, -9.273590339475653366, 63.47681654923867711 ) ) ;
#14995 = CARTESIAN_POINT ( 'NONE',  ( -10.45859239952313224, -15.89938452881993847, 64.79299464097340433 ) ) ;
#14996 = AXIS2_PLACEMENT_3D ( 'NONE', #31190, #19377, #669 ) ;
#14997 = ORIENTED_EDGE ( 'NONE', *, *, #22427, .T. ) ;
#14998 = B_SPLINE_CURVE_WITH_KNOTS ( 'NONE', 3,
 ( #46872, #47604, #9455, #17050, #32096, #31616, #36012, #39237, #2292, #9703 ),
 .UNSPECIFIED., .F., .F.,
 ( 4, 2, 2, 2, 4 ),
 ( 0.000000000000000000, 0.2500000000000000000, 0.5000000000000000000, 0.7500000000000000000, 1.000000000000000000 ),
 .UNSPECIFIED. ) ;
#14999 = CARTESIAN_POINT ( 'NONE',  ( -24.47111443619382243, -12.39179416916012855, 73.41942463439355038 ) ) ;
#15000 = CARTESIAN_POINT ( 'NONE',  ( -12.79725882921341373, -20.12850138265567068, 72.10653676770067477 ) ) ;
#15001 = AXIS2_PLACEMENT_3D ( 'NONE', #22873, #3909, #18915 ) ;
#15002 = ORIENTED_EDGE ( 'NONE', *, *, #33942, .F. ) ;
#15003 = DIRECTION ( 'NONE',  ( -1.000000000000000000, -1.665334536937734564E-16, -1.927470528863183637E-16 ) ) ;
#15004 = CARTESIAN_POINT ( 'NONE',  ( -23.29909385595927773, -9.575706171368036479, 50.49555931301712519 ) ) ;
#15005 = CARTESIAN_POINT ( 'NONE',  ( -23.04367560227575140, -10.55211830211007218, 59.60203429193362012 ) ) ;
#15006 = EDGE_CURVE ( 'NONE', #9620, #11090, #28130, .T. ) ;
#15007 = VERTEX_POINT ( 'NONE', #15203 ) ;
#15008 = CARTESIAN_POINT ( 'NONE',  ( -12.74909871793134997, -15.13738746211001462, 49.52966884056655772 ) ) ;
#15009 = ORIENTED_EDGE ( 'NONE', *, *, #6688, .T. ) ;
#15010 = CARTESIAN_POINT ( 'NONE',  ( -19.62622408449249178, -21.50961356628077326, 61.88014844347227950 ) ) ;
#15011 = CARTESIAN_POINT ( 'NONE',  ( -11.14114413899577904, -10.80566798617789459, 57.32407932063995304 ) ) ;
#15012 = ORIENTED_EDGE ( 'NONE', *, *, #19348, .T. ) ;
#15013 = DIRECTION ( 'NONE',  ( -0.9524241471993249997, -0.0009228828802096092788, 0.3047743298226210373 ) ) ;
#15014 = CARTESIAN_POINT ( 'NONE',  ( -17.42409385541299471, -14.80920654474435771, 49.52966884056655772 ) ) ;
#15015 = CARTESIAN_POINT ( 'NONE',  ( -22.21784385650551741, -9.790100578890868377, 49.79778022625163203 ) ) ;
#15016 = VECTOR ( 'NONE', #19539, 1000.000000000000000 ) ;
#15017 = CARTESIAN_POINT ( 'NONE',  ( -10.35611353805053980, -12.45393147150008772, 61.05499485166044593 ) ) ;
#15018 =( BOUNDED_CURVE ( )  B_SPLINE_CURVE ( 3, ( #35458, #21432, #9135, #43358 ),
 .UNSPECIFIED., .F., .F. ) 
 B_SPLINE_CURVE_WITH_KNOTS ( ( 4, 4 ),
 ( 0.000000000000000000, 0.4074455897393596260 ),
 .UNSPECIFIED. ) 
 CURVE ( )  GEOMETRIC_REPRESENTATION_ITEM ( )  RATIONAL_B_SPLINE_CURVE ( ( 1.000000000000000000, 0.4567392136813386294, 0.3561768502900327649, 0.6983129098260822953 ) ) 
 REPRESENTATION_ITEM ( '' )  );
#15019 = CARTESIAN_POINT ( 'NONE',  ( -24.26499744607890818, -17.75976858747020160, 62.65856309191605789 ) ) ;
#15020 = CARTESIAN_POINT ( 'NONE',  ( -14.06159385759798930, -7.228003583438117552, 51.38655588711986155 ) ) ;
#15021 = PLANE ( 'NONE',  #28230 ) ;
#15022 = VERTEX_POINT ( 'NONE', #7611 ) ;
#15023 = CIRCLE ( 'NONE', #15809, 5.249999999999998224 ) ;
#15024 = CARTESIAN_POINT ( 'NONE',  ( -19.09647057632575340, -21.60781438815542188, 58.75337332744499719 ) ) ;
#15025 = CARTESIAN_POINT ( 'NONE',  ( -10.40687472791218049, -14.09964931664121579, 64.80292589203708076 ) ) ;
#15026 = CARTESIAN_POINT ( 'NONE',  ( -23.34481426128875370, -18.63642081788812987, 69.29371984264746231 ) ) ;
#15027 = CARTESIAN_POINT ( 'NONE',  ( -45.50908060261262023, -14.20920654474410760, 70.13000000000000966 ) ) ;
#15028 = CARTESIAN_POINT ( 'NONE',  ( -16.04563226305852908, -7.895241551553309201, 63.97010999323463665 ) ) ;
#15029 = ORIENTED_EDGE ( 'NONE', *, *, #30425, .F. ) ;
#15030 = ORIENTED_EDGE ( 'NONE', *, *, #26750, .F. ) ;
#15031 = EDGE_CURVE ( 'NONE', #5311, #31006, #33931, .T. ) ;
#15032 = CARTESIAN_POINT ( 'NONE',  ( -24.05923365589681140, -11.41972516488058176, 66.60869825954527812 ) ) ;
#15033 = CARTESIAN_POINT ( 'NONE',  ( -10.50893933415051507, -13.43540278197273885, 74.96345540680638919 ) ) ;
#15034 = ORIENTED_EDGE ( 'NONE', *, *, #29131, .F. ) ;
#15035 = CARTESIAN_POINT ( 'NONE',  ( -17.79084007069931417, -7.768752218527305686, 60.38060768310333515 ) ) ;
#15036 = AXIS2_PLACEMENT_3D ( 'NONE', #45198, #11439, #20295 ) ;
#15037 = CARTESIAN_POINT ( 'NONE',  ( -18.19389434033494268, -22.21941471489327569, 65.53027570717884487 ) ) ;
#15038 = CARTESIAN_POINT ( 'NONE',  ( -12.47631366984485268, -9.857336861045936871, 57.38935527210361442 ) ) ;
#15039 = EDGE_CURVE ( 'NONE', #8569, #35964, #30336, .T. ) ;
#15040 = CARTESIAN_POINT ( 'NONE',  ( -10.45988366621089405, -15.51674690159928005, 57.58295249508964275 ) ) ;
#15041 = DIRECTION ( 'NONE',  ( -0.1240347345892086062, 1.145860353393066553E-16, -0.9922778767136676281 ) ) ;
#15042 = CARTESIAN_POINT ( 'NONE',  ( -24.30048588269890431, -16.36411231998812710, 59.12332431758469653 ) ) ;
#15043 =( BOUNDED_SURFACE ( )  B_SPLINE_SURFACE ( 3, 1, ( 
 ( #29308, #25605 ),
 ( #36917, #40870 ),
 ( #3442, #27074 ),
 ( #23880, #38142 ),
 ( #31497, #15975 ),
 ( #4926, #39117 ),
 ( #46282, #34938 ) ),
 .UNSPECIFIED., .T., .F., .F. ) 
 B_SPLINE_SURFACE_WITH_KNOTS ( ( 4, 3, 4 ),
 ( 2, 2 ),
 ( 0.000000000000000000, 0.5000000000000000000, 1.000000000000000000 ),
 ( 0.000000000000000000, 1.000000000000000000 ),
 .UNSPECIFIED. ) 
 GEOMETRIC_REPRESENTATION_ITEM ( )  RATIONAL_B_SPLINE_SURFACE ( (
 ( 1.000000000000000000, 1.000000000000000000),
 ( 0.3333333333333335369, 0.3333333333333330373),
 ( 0.3333333333333335369, 0.3333333333333330373),
 ( 1.000000000000000000, 1.000000000000000000),
 ( 0.3333333333333333703, 0.3333333333333333703),
 ( 0.3333333333333333703, 0.3333333333333333703),
 ( 1.000000000000000000, 1.000000000000000000) ) ) 
 REPRESENTATION_ITEM ( '' )  SURFACE ( )  );
#15044 = CARTESIAN_POINT ( 'NONE',  ( -13.98060997152859741, -8.714678138767887106, 74.42628082040340587 ) ) ;
#15045 = ADVANCED_FACE ( 'NONE', ( #26804 ), #7119, .T. ) ;
#15046 = DIRECTION ( 'NONE',  ( 2.866981220435666553E-17, -1.000000000000000000, -1.190614954331866791E-16 ) ) ;
#15047 = DIRECTION ( 'NONE',  ( 1.927470528863184130E-16, 1.434740771370715221E-29, -1.000000000000000000 ) ) ;
#15048 = VERTEX_POINT ( 'NONE', #460 ) ;
#15049 = CIRCLE ( 'NONE', #40246, 2.000000000000001776 ) ;
#15050 = CARTESIAN_POINT ( 'NONE',  ( -20.35133084405233816, -8.395599718752041696, 67.08104079005559583 ) ) ;
#15051 = CARTESIAN_POINT ( 'NONE',  ( -45.92409385541306222, -14.20920654474410760, 70.50000000000000000 ) ) ;
#15052 = CARTESIAN_POINT ( 'NONE',  ( -15.65211700886707469, -8.035536993839519582, 74.19058801755400623 ) ) ;
#15053 = CARTESIAN_POINT ( 'NONE',  ( -20.64284385759799534, -7.587656875400192291, 49.25157356644813689 ) ) ;
#15054 = CARTESIAN_POINT ( 'NONE',  ( -21.23034385541294711, -6.857644439847737416, 49.98602051094152898 ) ) ;
#15055 = EDGE_CURVE ( 'NONE', #43598, #9477, #34451, .T. ) ;
#15056 = CARTESIAN_POINT ( 'NONE',  ( -11.83525646650322827, -10.59418119787233259, 74.43885130403194239 ) ) ;
#15057 = CARTESIAN_POINT ( 'NONE',  ( -18.19389323530821301, -22.21941482433020809, 65.53027461949925225 ) ) ;
#15058 = ORIENTED_EDGE ( 'NONE', *, *, #6005, .T. ) ;
#15059 = VERTEX_POINT ( 'NONE', #15439 ) ;
#15060 = CARTESIAN_POINT ( 'NONE',  ( -13.86159385541304090, -7.228003583438117552, 51.38655588711986155 ) ) ;
#15061 = CIRCLE ( 'NONE', #30032, 5.249999999999998224 ) ;
#15062 = ORIENTED_EDGE ( 'NONE', *, *, #89, .T. ) ;
#15063 = CARTESIAN_POINT ( 'NONE',  ( -15.91784385759799392, -6.860780111191481900, 51.02154966934377001 ) ) ;
#15064 = VECTOR ( 'NONE', #5272, 1000.000000000000000 ) ;
#15065 = DIRECTION ( 'NONE',  ( -0.9789991564299000970, -0.2038642972899922245, 4.410747590293501912E-08 ) ) ;
#15066 = CARTESIAN_POINT ( 'NONE',  ( -13.72409385759798894, -9.359200813967568422, 50.49621490985803263 ) ) ;
#15067 = CARTESIAN_POINT ( 'NONE',  ( -17.84575570470781258, -7.371070506658266908, 60.33706685437874739 ) ) ;
#15068 = VERTEX_POINT ( 'NONE', #7857 ) ;
#15069 = CARTESIAN_POINT ( 'NONE',  ( -13.59269417415731063, -21.19935819725622039, 65.09973481642835225 ) ) ;
#15070 = CIRCLE ( 'NONE', #22165, 2.000000000000000888 ) ;
#15071 = CARTESIAN_POINT ( 'NONE',  ( -21.84079957929829874, -9.314189696129256291, 63.19153755727188582 ) ) ;
#15072 = ORIENTED_EDGE ( 'NONE', *, *, #39126, .T. ) ;
#15073 = CARTESIAN_POINT ( 'NONE',  ( -24.72409385541305582, -14.80920654474417830, 64.94117647058821774 ) ) ;
#15074 = ADVANCED_FACE ( 'NONE', ( #30012 ), #12599, .T. ) ;
#15075 = CARTESIAN_POINT ( 'NONE',  ( -12.26463566984678621, -20.18368350662160182, 65.02708282775662951 ) ) ;
#15076 = VERTEX_POINT ( 'NONE', #701 ) ;
#15077 = CARTESIAN_POINT ( 'NONE',  ( -17.42409385541299471, -14.80920654474435771, 49.52966884056655772 ) ) ;
#15078 = DIRECTION ( 'NONE',  ( -0.7489133456531320565, -0.6626679415081376812, 6.686399169904807862E-09 ) ) ;
#15079 = CARTESIAN_POINT ( 'NONE',  ( -24.03361690119365335, -12.50376453790854647, 73.52760217071977422 ) ) ;
#15080 = ORIENTED_EDGE ( 'NONE', *, *, #4427, .T. ) ;
#15081 = CARTESIAN_POINT ( 'NONE',  ( -19.78614017500849087, -21.39864787494504839, 68.93482476778672208 ) ) ;
#15082 = B_SPLINE_CURVE_WITH_KNOTS ( 'NONE', 3,
 ( #42110, #38651, #8629, #42611, #23892, #26857, #4938, #45582, #34948, #991 ),
 .UNSPECIFIED., .F., .F.,
 ( 4, 2, 2, 2, 4 ),
 ( 0.000000000000000000, 0.2500000000000000000, 0.5000000000000000000, 0.7500000000000000000, 1.000000000000000000 ),
 .UNSPECIFIED. ) ;
#15083 = DIRECTION ( 'NONE',  ( 0.9710973231077277834, -0.2386838684389877285, 7.431671637556432894E-08 ) ) ;
#15084 = B_SPLINE_CURVE_WITH_KNOTS ( 'NONE', 3,
 ( #12968, #38599, #23345, #1407, #1660, #30981, #27760, #23840, #20380, #35138 ),
 .UNSPECIFIED., .F., .F.,
 ( 4, 2, 2, 2, 4 ),
 ( 0.6272669072877694596, 0.7522669073072851820, 0.8772669073268009043, 1.002266907346316627, 1.127266907365832349 ),
 .UNSPECIFIED. ) ;
#15085 = CARTESIAN_POINT ( 'NONE',  ( -24.71334354870178274, -13.26952572216105075, 59.47772645308575790 ) ) ;
#15086 = DIRECTION ( 'NONE',  ( -3.071710424422018668E-17, 6.404604876783312462E-16, 1.000000000000000000 ) ) ;
#15087 = ORIENTED_EDGE ( 'NONE', *, *, #21366, .F. ) ;
#15088 = CARTESIAN_POINT ( 'NONE',  ( -24.37445139888341927, -16.03700657411734198, 59.27899288712937675 ) ) ;
#15089 = FACE_OUTER_BOUND ( 'NONE', #33454, .T. ) ;
#15090 = EDGE_CURVE ( 'NONE', #33946, #7654, #39052, .T. ) ;
#15091 = DIRECTION ( 'NONE',  ( -3.071710424422018668E-17, 6.404604876783312462E-16, 1.000000000000000000 ) ) ;
#15092 = CARTESIAN_POINT ( 'NONE',  ( -18.44528782684011858, -21.78515541812411982, 72.29983070759432451 ) ) ;
#15093 = CARTESIAN_POINT ( 'NONE',  ( -16.14646913593085742, -7.469405111292049426, 60.36061804874157843 ) ) ;
#15094 = CARTESIAN_POINT ( 'NONE',  ( 25.57590614458706568, 1.890747609047893185, 50.53028072113869484 ) ) ;
#15095 = CARTESIAN_POINT ( 'NONE',  ( -20.21784385650551386, -9.790100578890868377, 49.79778022625163203 ) ) ;
#15096 = VERTEX_POINT ( 'NONE', #37119 ) ;
#15097 = AXIS2_PLACEMENT_3D ( 'NONE', #39305, #2357, #42767 ) ;
#15098 = CARTESIAN_POINT ( 'NONE',  ( -16.30010877417799264, -7.443724743308521852, 60.38683862147721726 ) ) ;
#15099 = LINE ( 'NONE', #18550, #2195 ) ;
#15100 = ORIENTED_EDGE ( 'NONE', *, *, #13877, .T. ) ;
#15101 = CARTESIAN_POINT ( 'NONE',  ( -22.37985709289073455, -19.82347726015160205, 69.17417989525732480 ) ) ;
#15102 = CARTESIAN_POINT ( 'NONE',  ( -22.49805064719525305, -9.986866608920609067, 73.48161091687566682 ) ) ;
#15103 = DIRECTION ( 'NONE',  ( -0.9375570856950864451, 0.3478314405900309603, -3.549360974553817487E-17 ) ) ;
#15104 = VERTEX_POINT ( 'NONE', #31700 ) ;
#15105 = DIRECTION ( 'NONE',  ( 3.964551030465574775E-06, 2.747358549199493871E-07, -0.9999999999921034277 ) ) ;
#15106 = EDGE_CURVE ( 'NONE', #4399, #956, #43288, .T. ) ;
#15107 = LINE ( 'NONE', #11675, #33782 ) ;
#15108 = B_SPLINE_CURVE_WITH_KNOTS ( 'NONE', 1,
 ( #46894, #31386 ),
 .UNSPECIFIED., .F., .F.,
 ( 2, 2 ),
 ( 0.000000000000000000, 1.000000000000000000 ),
 .UNSPECIFIED. ) ;
#15109 = ORIENTED_EDGE ( 'NONE', *, *, #11058, .T. ) ;
#15110 = CARTESIAN_POINT ( 'NONE',  ( -14.48034385650551847, -6.424090610841176385, 49.80797279389977916 ) ) ;
#15111 = EDGE_CURVE ( 'NONE', #6268, #36141, #44398, .T. ) ;
#15112 = EDGE_CURVE ( 'NONE', #38065, #29761, #39079, .T. ) ;
#15113 = CARTESIAN_POINT ( 'NONE',  ( -18.77307807160576303, -7.482301894102196371, 70.56342156955103917 ) ) ;
#15114 = DIRECTION ( 'NONE',  ( -3.071710424422018668E-17, 6.404604876783312462E-16, 1.000000000000000000 ) ) ;
#15115 = CARTESIAN_POINT ( 'NONE',  ( -13.62948724496060215, -8.926948417807865965, 57.26967755883410405 ) ) ;
#15116 = ORIENTED_EDGE ( 'NONE', *, *, #31984, .F. ) ;
#15117 = ORIENTED_EDGE ( 'NONE', *, *, #19993, .T. ) ;
#15118 = CARTESIAN_POINT ( 'NONE',  ( -16.25534385650551528, -7.417179338643134834, 52.18511593390279302 ) ) ;
#15119 = B_SPLINE_CURVE_WITH_KNOTS ( 'NONE', 3,
 ( #40928, #24773, #43245, #14541, #9262, #40677, #5581, #7214, #29606, #44395 ),
 .UNSPECIFIED., .F., .F.,
 ( 4, 2, 2, 2, 4 ),
 ( 0.1272669073658040384, 0.2522669073462902034, 0.3772669073267763129, 0.5022669073072624224, 0.6272669072877485874 ),
 .UNSPECIFIED. ) ;
#15120 = FACE_OUTER_BOUND ( 'NONE', #20843, .T. ) ;
#15121 = CARTESIAN_POINT ( 'NONE',  ( -16.19814190158817269, -21.75179548504963023, 58.43585572027992470 ) ) ;
#15123 = EDGE_CURVE ( 'NONE', #10945, #10797, #13965, .T. ) ;
#15122 = CARTESIAN_POINT ( 'NONE',  ( -14.28659385650551528, -9.302874398569244363, 51.68646062012417985 ) ) ;
#15124 = EDGE_CURVE ( 'NONE', #46532, #12430, #6301, .T. ) ;
#15125 = EDGE_CURVE ( 'NONE', #21906, #19358, #12023, .T. ) ;
#15126 = ADVANCED_FACE ( 'NONE', ( #12743 ), #20131, .T. ) ;
#15127 = CARTESIAN_POINT ( 'NONE',  ( -17.85728874018076340, -21.84618329174708151, 61.89007996730683203 ) ) ;
#15128 = CARTESIAN_POINT ( 'NONE',  ( -18.83482760403246203, -7.952772484924772733, 67.18606370727887622 ) ) ;
#15129 = CARTESIAN_POINT ( 'NONE',  ( -23.79305894267454491, -17.83234277001198365, 59.00378422961142633 ) ) ;
#15130 = EDGE_LOOP ( 'NONE', ( #24092, #26357, #1617, #10322, #48047 ) ) ;
#15131 = CARTESIAN_POINT ( 'NONE',  ( -12.20851000913748585, -19.55815686523975927, 61.69678616734186960 ) ) ;
#15132 = VERTEX_POINT ( 'NONE', #43021 ) ;
#15133 = CARTESIAN_POINT ( 'NONE',  ( -13.01482893870565682, -8.804038099563683772, 63.95300575187839343 ) ) ;
#15134 = CARTESIAN_POINT ( 'NONE',  ( -24.83243314287557268, -14.02236757053316651, 73.32282709813433996 ) ) ;
#15135 = CARTESIAN_POINT ( 'NONE',  ( -17.42409385541299471, -14.80920654474435771, 49.52966884056655772 ) ) ;
#15136 = FACE_OUTER_BOUND ( 'NONE', #25575, .T. ) ;
#15137 = EDGE_LOOP ( 'NONE', ( #11099, #20509, #11537, #15807, #43294 ) ) ;
#15138 = CARTESIAN_POINT ( 'NONE',  ( -18.05557233295238362, -22.23314744338585669, 61.98880637900742130 ) ) ;
#15139 = DIRECTION ( 'NONE',  ( -0.000000000000000000, -1.000000000000000000, -0.000000000000000000 ) ) ;
#15140 = CARTESIAN_POINT ( 'NONE',  ( -20.17268378225416825, -8.371407738384645469, 70.25100341248858626 ) ) ;
#15141 = CARTESIAN_POINT ( 'NONE',  ( -24.31482341358216104, -13.31912415075585088, 59.51267924675325816 ) ) ;
#15142 = EDGE_LOOP ( 'NONE', ( #26842, #25135, #4833, #21879, #33828 ) ) ;
#15143 = CARTESIAN_POINT ( 'NONE',  ( -23.00441930688031889, -19.11762475274336737, 59.03410642058399560 ) ) ;
#15144 = CYLINDRICAL_SURFACE ( 'NONE', #39187, 0.1499999999999954148 ) ;
#15145 = CARTESIAN_POINT ( 'NONE',  ( -24.20371252810814866, -12.87440185077122834, 66.58774614429587757 ) ) ;
#15146 = FACE_BOUND ( 'NONE', #46050, .T. ) ;
#15147 = ORIENTED_EDGE ( 'NONE', *, *, #32228, .F. ) ;
#15148 = DIRECTION ( 'NONE',  ( 0.000000000000000000, 0.007114381193220344589, -0.9999746924698832418 ) ) ;
#15150 = EDGE_CURVE ( 'NONE', #2446, #13964, #15084, .T. ) ;
#15149 = CARTESIAN_POINT ( 'NONE',  ( -17.42409385541299471, -14.80920654474435594, 52.02966884056656482 ) ) ;
#15151 = VECTOR ( 'NONE', #31380, 1000.000000000000000 ) ;
#15152 = CARTESIAN_POINT ( 'NONE',  ( -13.08322001584757643, -9.253902105542977097, 67.67382971635112199 ) ) ;
#15153 = CARTESIAN_POINT ( 'NONE',  ( -21.19428927390184114, -8.848463597801222491, 73.48639860482715847 ) ) ;
#15154 = ORIENTED_EDGE ( 'NONE', *, *, #35430, .F. ) ;
#15155 = CARTESIAN_POINT ( 'NONE',  ( -17.42409385541299471, -14.80920654474435594, 52.02966884056656482 ) ) ;
#15156 = ORIENTED_EDGE ( 'NONE', *, *, #48131, .F. ) ;
#15157 = CARTESIAN_POINT ( 'NONE',  ( -12.74071866071660075, -9.015263582886822391, 70.96429948631303830 ) ) ;
#15158 = CARTESIAN_POINT ( 'NONE',  ( -17.15134141312287852, -7.364115244199362920, 70.67531166753866501 ) ) ;
#15159 = DIRECTION ( 'NONE',  ( -0.000000000000000000, -1.000000000000000000, -0.000000000000000000 ) ) ;
#15160 = ORIENTED_EDGE ( 'NONE', *, *, #26053, .T. ) ;
#15161 = CARTESIAN_POINT ( 'NONE',  ( -10.96962198434375146, -17.51872840680399790, 68.09721950251682188 ) ) ;
#15162 = EDGE_CURVE ( 'NONE', #5861, #7442, #10413, .T. ) ;
#15163 = ORIENTED_EDGE ( 'NONE', *, *, #22639, .F. ) ;
#15164 = ORIENTED_EDGE ( 'NONE', *, *, #38391, .T. ) ;
#15165 = VERTEX_POINT ( 'NONE', #5120 ) ;
#15166 = DIRECTION ( 'NONE',  ( -0.2737502900231349456, -0.9618007999124592589, 5.400150802763565238E-08 ) ) ;
#15167 = CARTESIAN_POINT ( 'NONE',  ( -13.32832405134409548, -21.03232224849095289, 61.66646320379408053 ) ) ;
#15168 = CARTESIAN_POINT ( 'NONE',  ( -12.84615363328625826, -20.17103110633857455, 72.09181604382622766 ) ) ;
#15169 = CARTESIAN_POINT ( 'NONE',  ( -10.03795483766491969, -13.83545689752550345, 57.64163354902277803 ) ) ;
#15170 =( BOUNDED_CURVE ( )  B_SPLINE_CURVE ( 3, ( #8968, #4527, #5516, #20039 ),
 .UNSPECIFIED., .F., .F. ) 
 B_SPLINE_CURVE_WITH_KNOTS ( ( 4, 4 ),
 ( 0.000000000000000000, 0.4074455897393726156 ),
 .UNSPECIFIED. ) 
 CURVE ( )  GEOMETRIC_REPRESENTATION_ITEM ( )  RATIONAL_B_SPLINE_CURVE ( ( 1.000000000000000000, 0.4567392136813217540, 0.3561768502900264921, 0.6983129098261142698 ) ) 
 REPRESENTATION_ITEM ( '' )  );
#15171 = CARTESIAN_POINT ( 'NONE',  ( -10.37818533259200748, -17.22973363664382873, 61.27247698181179913 ) ) ;
#15172 = LINE ( 'NONE', #14420, #1944 ) ;
#15173 = CARTESIAN_POINT ( 'NONE',  ( -17.42409385541300892, -14.80920654474439502, 75.49999999999994316 ) ) ;
#15174 = ORIENTED_EDGE ( 'NONE', *, *, #19799, .T. ) ;
#15175 = ORIENTED_EDGE ( 'NONE', *, *, #34889, .F. ) ;
#15176 = CARTESIAN_POINT ( 'NONE',  ( -10.37394849890712401, -14.76283852923608286, 71.61310637325181006 ) ) ;
#15177 = CARTESIAN_POINT ( 'NONE',  ( -13.92301192392296727, -8.232980258883593194, 74.37767385738736436 ) ) ;
#15178 = DIRECTION ( 'NONE',  ( -0.9243256318339804212, 0.3816046728418208134, -8.614662759602032238E-09 ) ) ;
#15179 = DIRECTION ( 'NONE',  ( -0.9926276493613469531, -0.06323820549165627691, 0.1033986416233890343 ) ) ;
#15180 = VERTEX_POINT ( 'NONE', #5363 ) ;
#15181 = CARTESIAN_POINT ( 'NONE',  ( -14.70534385650551989, -8.801233750844183135, 48.81488406609782515 ) ) ;
#15182 =( BOUNDED_CURVE ( )  B_SPLINE_CURVE ( 3, ( #23496, #35042, #45421, #1308 ),
 .UNSPECIFIED., .F., .F. ) 
 B_SPLINE_CURVE_WITH_KNOTS ( ( 4, 4 ),
 ( 0.9074455897393683967, 1.000000000000000000 ),
 .UNSPECIFIED. ) 
 CURVE ( )  GEOMETRIC_REPRESENTATION_ITEM ( )  RATIONAL_B_SPLINE_CURVE ( ( 0.6983129098260925094, 0.7760317562606977582, 0.8765941196520002920, 1.000000000000000000 ) ) 
 REPRESENTATION_ITEM ( '' )  );
#15183 = EDGE_CURVE ( 'NONE', #22634, #47594, #672, .T. ) ;
#15184 = ORIENTED_EDGE ( 'NONE', *, *, #33387, .F. ) ;
#15185 = EDGE_CURVE ( 'NONE', #29482, #17265, #34899, .T. ) ;
#15186 = ADVANCED_FACE ( 'NONE', ( #34662 ), #12031, .T. ) ;
#15187 = CARTESIAN_POINT ( 'NONE',  ( -17.01596769717176372, -7.370308014455987156, 74.07522855441366971 ) ) ;
#15188 = CARTESIAN_POINT ( 'NONE',  ( -12.31380156693488992, -10.02538874655004442, 60.85918086676540639 ) ) ;
#15189 = AXIS2_PLACEMENT_3D ( 'NONE', #21589, #24135, #40300 ) ;
#15190 = DIRECTION ( 'NONE',  ( 1.078386539787844256E-05, -7.293043934967424929E-06, 0.9999999999152597852 ) ) ;
#15191 = ORIENTED_EDGE ( 'NONE', *, *, #27519, .T. ) ;
#15192 = CARTESIAN_POINT ( 'NONE',  ( -14.22441497990486958, -8.081217732231424478, 67.44470516081543110 ) ) ;
#15193 =( BOUNDED_CURVE ( )  B_SPLINE_CURVE ( 3, ( #35974, #16537, #9419, #46609 ),
 .UNSPECIFIED., .F., .F. ) 
 B_SPLINE_CURVE_WITH_KNOTS ( ( 4, 4 ),
 ( 0.000000000000000000, 0.4074455897393700621 ),
 .UNSPECIFIED. ) 
 CURVE ( )  GEOMETRIC_REPRESENTATION_ITEM ( )  RATIONAL_B_SPLINE_CURVE ( ( 1.000000000000000000, 0.4567392136813238634, 0.3561768502900273248, 0.6983129098261103840 ) ) 
 REPRESENTATION_ITEM ( '' )  );
#15194 = ADVANCED_FACE ( 'NONE', ( #36346 ), #40302, .T. ) ;
#15195 = CARTESIAN_POINT ( 'NONE',  ( -10.90856645720024254, -17.50971350489534828, 64.51250748301919202 ) ) ;
#15196 = ORIENTED_EDGE ( 'NONE', *, *, #17958, .T. ) ;
#15197 = LINE ( 'NONE', #45275, #39904 ) ;
#15198 = CARTESIAN_POINT ( 'NONE',  ( -21.73853604213786639, -16.63919858500264937, 52.02966884056656482 ) ) ;
#15199 = CARTESIAN_POINT ( 'NONE',  ( -10.51729421260818498, -16.22293138110306998, 71.44750383217574097 ) ) ;
#15200 = ORIENTED_EDGE ( 'NONE', *, *, #37527, .T. ) ;
#15201 = CARTESIAN_POINT ( 'NONE',  ( -24.68464418333330102, -16.47883131643914467, 59.31670754753076835 ) ) ;
#15202 = VERTEX_POINT ( 'NONE', #14162 ) ;
#15203 = CARTESIAN_POINT ( 'NONE',  ( -10.03904597514415009, -13.82694077737217242, 57.56329639008353638 ) ) ;
#15204 = CARTESIAN_POINT ( 'NONE',  ( -24.75425692978680559, -16.14426119111164937, 62.70673273743753384 ) ) ;
#15205 = ORIENTED_EDGE ( 'NONE', *, *, #23115, .F. ) ;
#15206 = CARTESIAN_POINT ( 'NONE',  ( -22.26378936042422296, -19.94069658942875733, 62.23439075274148280 ) ) ;
#15208 = EDGE_CURVE ( 'NONE', #27480, #4575, #2547, .T. ) ;
#15207 = CARTESIAN_POINT ( 'NONE',  ( -24.38143469521110518, -15.58083332675401067, 73.00303748421107741 ) ) ;
#15209 = CARTESIAN_POINT ( 'NONE',  ( -20.31063670516350328, -8.430306149294633400, 70.36173336096577202 ) ) ;
#15210 = ORIENTED_EDGE ( 'NONE', *, *, #45495, .T. ) ;
#15211 = CARTESIAN_POINT ( 'NONE',  ( -21.42981021932851249, -20.54985930702059349, 72.75119662013757704 ) ) ;
#15212 = DIRECTION ( 'NONE',  ( -2.866981220435666553E-17, 1.000000000000000000, 1.190614954331866791E-16 ) ) ;
#15213 = DIRECTION ( 'NONE',  ( 0.9048399035850771543, 0.4257519804770706906, 1.330923649722295736E-08 ) ) ;
#15214 = VERTEX_POINT ( 'NONE', #32430 ) ;
#15215 = CARTESIAN_POINT ( 'NONE',  ( -19.24512995744831656, -8.048560962921746054, 63.62016385155983045 ) ) ;
#15216 = CARTESIAN_POINT ( 'NONE',  ( -21.75074122386538988, -8.744327870424561056, 70.33121307893182461 ) ) ;
#15217 = EDGE_CURVE ( 'NONE', #47695, #11292, #10454, .T. ) ;
#15218 = VECTOR ( 'NONE', #16058, 1000.000000000000000 ) ;
#15219 = ORIENTED_EDGE ( 'NONE', *, *, #26061, .F. ) ;
#15220 = EDGE_LOOP ( 'NONE', ( #39244, #9509, #22357, #9610 ) ) ;
#15221 = CARTESIAN_POINT ( 'NONE',  ( -10.48241187047983658, -15.71137557247682892, 61.32323669680387468 ) ) ;
#15222 = CARTESIAN_POINT ( 'NONE',  ( -24.02518650215770890, -17.29497017970488315, 72.97516058001660610 ) ) ;
#15223 = CARTESIAN_POINT ( 'NONE',  ( -22.92560359444879836, -19.23055950467793096, 62.49839992038752712 ) ) ;
#15224 = CARTESIAN_POINT ( 'NONE',  ( -24.87556905619337755, -15.80954572138182712, 54.02312124697527906 ) ) ;
#15225 = CARTESIAN_POINT ( 'NONE',  ( -22.24284385650551954, -8.811426318492348031, 52.18089403414751359 ) ) ;
#15226 = LINE ( 'NONE', #31001, #12447 ) ;
#15227 = CARTESIAN_POINT ( 'NONE',  ( -11.64339224431418529, -10.10844562305556771, 71.15548443915361077 ) ) ;
#15228 = DIRECTION ( 'NONE',  ( -0.03181436478788690625, -0.9994937949748078365, -6.982004198809110323E-09 ) ) ;
#15229 = CARTESIAN_POINT ( 'NONE',  ( -12.12844827754892485, -10.15526124722410195, 64.32914323983619909 ) ) ;
#15230 = ORIENTED_EDGE ( 'NONE', *, *, #23618, .T. ) ;
#15231 = CARTESIAN_POINT ( 'NONE',  ( -27.79065715166790795, -17.71243352067323329, 54.61912878955446615 ) ) ;
#15232 = SHAPE_REPRESENTATION_RELATIONSHIP ( 'NONE' , 'NONE' ,  #41459, #15583 ) ;
#15233 = CARTESIAN_POINT ( 'NONE',  ( -14.36038767613011302, -18.37140530287405227, 52.02966884056656482 ) ) ;
#15234 = VERTEX_POINT ( 'NONE', #28731 ) ;
#15235 = EDGE_LOOP ( 'NONE', ( #6733, #35095 ) ) ;
#15236 = ADVANCED_FACE ( 'NONE', ( #17628 ), #2136, .T. ) ;
#15237 = DIRECTION ( 'NONE',  ( 2.866981220435666553E-17, -1.000000000000000000, -1.190614954331866791E-16 ) ) ;
#15238 = LINE ( 'NONE', #44831, #15843 ) ;
#15239 = CARTESIAN_POINT ( 'NONE',  ( -13.29208520756706235, -21.00847154833298802, 61.63929462826596506 ) ) ;
#15240 = DIRECTION ( 'NONE',  ( -0.09077643883959131410, 0.9958712959773468043, 4.338678762321648664E-08 ) ) ;
#15241 = EDGE_LOOP ( 'NONE', ( #14054, #23903 ) ) ;
#15242 = CARTESIAN_POINT ( 'NONE',  ( -11.46028008028683942, -18.56947564720590194, 61.56238700194530367 ) ) ;
#15243 = AXIS2_PLACEMENT_3D ( 'NONE', #6530, #40017, #36533 ) ;
#15244 = ADVANCED_FACE ( 'NONE', ( #44017 ), #27417, .T. ) ;
#15245 = EDGE_CURVE ( 'NONE', #15772, #39638, #983, .T. ) ;
#15246 = DIRECTION ( 'NONE',  ( 0.6827297667453423591, 0.7306709694519485376, 5.176517822219623819E-09 ) ) ;
#15247 = ORIENTED_EDGE ( 'NONE', *, *, #4493, .F. ) ;
#15248 = EDGE_CURVE ( 'NONE', #36768, #46722, #35857, .T. ) ;
#15249 = CARTESIAN_POINT ( 'NONE',  ( -22.48964968825576705, -9.905448439006629968, 73.76689030015370463 ) ) ;
#15250 = CARTESIAN_POINT ( 'NONE',  ( -11.42587710518540334, -11.10406226247761019, 57.49431069621225276 ) ) ;
#15251 = ADVANCED_FACE ( 'NONE', ( #9786 ), #39809, .T. ) ;
#15252 = CARTESIAN_POINT ( 'NONE',  ( -10.42462062184586635, -14.89508117765250361, 75.09778901762284420 ) ) ;
#15253 = VERTEX_POINT ( 'NONE', #14397 ) ;
#15254 = CARTESIAN_POINT ( 'NONE',  ( -17.39761456938454742, -7.809256627251312644, 67.32039592144390383 ) ) ;
#15255 = ORIENTED_EDGE ( 'NONE', *, *, #33934, .T. ) ;
#15256 = B_SPLINE_CURVE_WITH_KNOTS ( 'NONE', 3,
 ( #44813, #29291, #14470, #29529, #17703, #40597, #25356, #14972, #7631, #40372 ),
 .UNSPECIFIED., .F., .F.,
 ( 4, 2, 2, 2, 4 ),
 ( 0.1272669073658270755, 0.2522669073488479907, 0.3772669073318688504, 0.5022669073148897656, 0.6272669072979106808 ),
 .UNSPECIFIED. ) ;
#15257 = DIRECTION ( 'NONE',  ( -3.071710424422018668E-17, 6.404604876783312462E-16, 1.000000000000000000 ) ) ;
#15258 = CARTESIAN_POINT ( 'NONE',  ( -11.49500183448703083, -10.99442376238782337, 57.22375354680192316 ) ) ;
#15259 = EDGE_LOOP ( 'NONE', ( #13736, #40887, #34731, #23681, #7485 ) ) ;
#15260 = CARTESIAN_POINT ( 'NONE',  ( -11.55897615675186785, -7.397247749063358135, 53.49999999999995026 ) ) ;
#15261 = EDGE_CURVE ( 'NONE', #12832, #38958, #3102, .T. ) ;
#15262 = CARTESIAN_POINT ( 'NONE',  ( -20.53034385650551386, -9.794322478646142471, 51.19202720610083190 ) ) ;
#15263 = LINE ( 'NONE', #22942, #35423 ) ;
#15264 =( BOUNDED_CURVE ( )  B_SPLINE_CURVE ( 2, ( #38663, #46055, #12796, #20188, #27336, #27820, #13029, #8639, #5673 ),
 .UNSPECIFIED., .F., .F. ) 
 B_SPLINE_CURVE_WITH_KNOTS ( ( 3, 2, 2, 2, 3 ),
 ( 0.06294472996427230571, 0.06392819047740837257, 0.06491165099054443943, 0.06589511150368049242, 0.06687857201681655928 ),
 .UNSPECIFIED. ) 
 CURVE ( )  GEOMETRIC_REPRESENTATION_ITEM ( )  RATIONAL_B_SPLINE_CURVE ( ( 0.9999999999999537037, 0.9238795325113330348, 1.000000000000000000, 0.9238795325112867385, 1.000000000000000000, 0.9238795325112867385, 1.000000000000000000, 0.9238795325112624246, 1.000000000000024425 ) ) 
 REPRESENTATION_ITEM ( '' )  );
#15265 = CARTESIAN_POINT ( 'NONE',  ( -12.08107559391734220, -20.00099389537635020, 61.54678633777153607 ) ) ;
#15266 = CARTESIAN_POINT ( 'NONE',  ( -22.27817919856018136, -9.157513542003881568, 59.83675792137641736 ) ) ;
#15267 = DIRECTION ( 'NONE',  ( 1.000000000000000000, 0.000000000000000000, 0.000000000000000000 ) ) ;
#15268 = ORIENTED_EDGE ( 'NONE', *, *, #5816, .F. ) ;
#15269 = CARTESIAN_POINT ( 'NONE',  ( -22.07409385541323488, -6.859212275519745994, 50.50378509014079498 ) ) ;
#15270 = DIRECTION ( 'NONE',  ( -3.071710424422018668E-17, 6.404604876783312462E-16, 1.000000000000000000 ) ) ;
#15271 = CARTESIAN_POINT ( 'NONE',  ( -22.36648328953754827, -20.38374146207719662, 62.33415536511054711 ) ) ;
#15272 = DIRECTION ( 'NONE',  ( -5.731567514496413899E-31, -1.020425574103664789E-16, -1.000000000000000000 ) ) ;
#15273 = CARTESIAN_POINT ( 'NONE',  ( -23.76950082168947986, -18.71306838267522821, 72.94181022443689244 ) ) ;
#15274 = ORIENTED_EDGE ( 'NONE', *, *, #35855, .T. ) ;
#15275 = ORIENTED_EDGE ( 'NONE', *, *, #27467, .T. ) ;
#15276 = CARTESIAN_POINT ( 'NONE',  ( -23.81302322525746362, -11.80978145726242978, 66.56647414731462220 ) ) ;
#15277 = CARTESIAN_POINT ( 'NONE',  ( -11.89178903705324863, -10.43929771899554737, 71.26893105542536944 ) ) ;
#15278 = ORIENTED_EDGE ( 'NONE', *, *, #33153, .T. ) ;
#15279 = CARTESIAN_POINT ( 'NONE',  ( -24.11881394502254849, -17.01995806294775448, 73.16863963025599560 ) ) ;
#15280 = CARTESIAN_POINT ( 'NONE',  ( -16.38254737672540884, -22.18621074043892349, 61.91601456499802225 ) ) ;
#15281 = CARTESIAN_POINT ( 'NONE',  ( -12.54283200749232918, -9.790123543357045932, 57.16105715312289703 ) ) ;
#15282 = DIRECTION ( 'NONE',  ( -1.000000000000000000, 0.000000000000000000, 0.000000000000000000 ) ) ;
#15283 = CARTESIAN_POINT ( 'NONE',  ( -18.15014757327930539, -21.82545121811569189, 61.87535875776518424 ) ) ;
#15284 = CARTESIAN_POINT ( 'NONE',  ( -19.58369474063720261, -21.93945548790455291, 62.11690869439961205 ) ) ;
#15285 = CARTESIAN_POINT ( 'NONE',  ( -46.92409385541305511, -15.80920654474410725, 61.49999999999999289 ) ) ;
#15286 = CIRCLE ( 'NONE', #12179, 2.000000000000001332 ) ;
#15287 = DIRECTION ( 'NONE',  ( -3.071710424422018668E-17, 6.404604876783312462E-16, 1.000000000000000000 ) ) ;
#15288 = VECTOR ( 'NONE', #5801, 1000.000000000000000 ) ;
#15289 = CARTESIAN_POINT ( 'NONE',  ( -24.86610167639389246, -14.46236660854407674, 66.29797298380238146 ) ) ;
#15290 = CARTESIAN_POINT ( 'NONE',  ( -11.57079330372311787, -10.20035596359355878, 71.16881880436550034 ) ) ;
#15291 = CARTESIAN_POINT ( 'NONE',  ( -47.13112723832431783, -12.89566876303303466, 70.50000000000000000 ) ) ;
#15292 = CARTESIAN_POINT ( 'NONE',  ( -24.25486363958986757, -13.06355980472538469, 63.11792038370487035 ) ) ;
#15293 = EDGE_CURVE ( 'NONE', #24724, #20623, #3773, .T. ) ;
#15294 = CARTESIAN_POINT ( 'NONE',  ( -23.56879427660422266, -11.34691063241640130, 73.77682139093690239 ) ) ;
#15295 = EDGE_LOOP ( 'NONE', ( #27275, #26854, #40771, #10255, #8753 ) ) ;
#15296 = ORIENTED_EDGE ( 'NONE', *, *, #26943, .F. ) ;
#15297 = CARTESIAN_POINT ( 'NONE',  ( -13.97409385541304161, -6.859212275519751323, 50.50378509014259265 ) ) ;
#15298 = ORIENTED_EDGE ( 'NONE', *, *, #2607, .T. ) ;
#15299 = ADVANCED_FACE ( 'NONE', ( #4105, #22818, #18861, #18598, #3591, #23057, #44989, #7312, #11236, #41510, #33362, #33610, #26747, #29954, #19104, #48652, #37810, #44489, #14638, #26249, #40777, #25756, #34111, #10991, #41263, #15384, #48406, #41766, #44737, #30448, #33128, #14892, #33869, #7550, #37551, #18110, #45227, #26012, #3856, #7059, #22072, #45462, #170, #37069, #22312, #37304, #15146, #30206, #11471, #48166, #26494, #8052, #7803, #402, #29457, #10739, #4822, #38539, #9246, #31156, #27225, #27463, #45943, #34350, #31401, #42004, #9005, #12686, #19341, #23543, #34845, #1114, #35334, #20076, #1604, #19845, #42496, #8277, #16112 ), #884, .T. ) ;
#15300 = CARTESIAN_POINT ( 'NONE',  ( -23.19909385541299685, -8.105421454601382081, 49.25000573077632993 ) ) ;
#15301 = CARTESIAN_POINT ( 'NONE',  ( -17.42409385541299471, -14.80920654474435594, 52.02966884056656482 ) ) ;
#15302 = CARTESIAN_POINT ( 'NONE',  ( -13.35550429318260512, -8.568184490765622385, 57.15463139269148485 ) ) ;
#15303 = CARTESIAN_POINT ( 'NONE',  ( -16.98831825750070479, -22.24652902502744922, 72.20897298418123000 ) ) ;
#15304 = EDGE_LOOP ( 'NONE', ( #24283, #1508, #29867, #28393, #40789 ) ) ;
#15305 = EDGE_CURVE ( 'NONE', #10765, #9098, #47978, .T. ) ;
#15306 = CARTESIAN_POINT ( 'NONE',  ( -18.24684318355141599, -9.624075539355219533, 50.77966884056655772 ) ) ;
#15307 = CARTESIAN_POINT ( 'NONE',  ( -14.81535805098777736, -7.777528402031247623, 47.99999999999994316 ) ) ;
#15308 = EDGE_CURVE ( 'NONE', #3400, #4198, #36787, .T. ) ;
#15309 = ORIENTED_EDGE ( 'NONE', *, *, #29970, .T. ) ;
#15310 =( BOUNDED_SURFACE ( )  B_SPLINE_SURFACE ( 3, 1, ( 
 ( #21382, #43786 ),
 ( #10762, #33154 ),
 ( #21848, #40086 ),
 ( #36370, #36843 ),
 ( #48430, #2650 ),
 ( #48190, #7085 ),
 ( #3130, #32686 ) ),
 .UNSPECIFIED., .T., .F., .F. ) 
 B_SPLINE_SURFACE_WITH_KNOTS ( ( 4, 3, 4 ),
 ( 2, 2 ),
 ( 0.000000000000000000, 0.5000000000000000000, 1.000000000000000000 ),
 ( 0.000000000000000000, 1.000000000000000000 ),
 .UNSPECIFIED. ) 
 GEOMETRIC_REPRESENTATION_ITEM ( )  RATIONAL_B_SPLINE_SURFACE ( (
 ( 1.000000000000000000, 1.000000000000000000),
 ( 0.3333333333333335369, 0.3333333333333330373),
 ( 0.3333333333333335369, 0.3333333333333330373),
 ( 1.000000000000000000, 1.000000000000000000),
 ( 0.3333333333333333703, 0.3333333333333333703),
 ( 0.3333333333333333703, 0.3333333333333333703),
 ( 1.000000000000000000, 1.000000000000000000) ) ) 
 REPRESENTATION_ITEM ( '' )  SURFACE ( )  );
#15311 = DIRECTION ( 'NONE',  ( 3.020324423671394282E-15, -0.4461977533473619473, -0.8949343913984794119 ) ) ;
#15312 = CARTESIAN_POINT ( 'NONE',  ( -23.95744587143639492, -17.32345433839075710, 69.42956382067292509 ) ) ;
#15313 = AXIS2_PLACEMENT_3D ( 'NONE', #38808, #35101, #42025 ) ;
#15314 = ORIENTED_EDGE ( 'NONE', *, *, #47727, .F. ) ;
#15315 = ADVANCED_FACE ( 'NONE', ( #23786 ), #27707, .T. ) ;
#15316 = FACE_OUTER_BOUND ( 'NONE', #40023, .T. ) ;
#15317 = CARTESIAN_POINT ( 'NONE',  ( -11.07356115161467436, -11.86355474871830573, 74.57456719742380358 ) ) ;
#15318 = CARTESIAN_POINT ( 'NONE',  ( -18.02409385541303877, -9.359200813967568422, 50.49621490985803263 ) ) ;
#15319 = ORIENTED_EDGE ( 'NONE', *, *, #14401, .T. ) ;
#15320 = CARTESIAN_POINT ( 'NONE',  ( -10.92333774552318104, -11.17005719542045483, 64.34220356397069907 ) ) ;
#15321 = VECTOR ( 'NONE', #7553, 1000.000000000000000 ) ;
#15322 = DIRECTION ( 'NONE',  ( -0.9811758422909350186, -0.1931164583992469319, -7.863147538403236401E-08 ) ) ;
#15323 = EDGE_CURVE ( 'NONE', #3327, #44193, #46672, .T. ) ;
#15324 = CARTESIAN_POINT ( 'NONE',  ( -18.37786432726835883, -21.79469297182707521, 69.10042588711679912 ) ) ;
#15325 = CARTESIAN_POINT ( 'NONE',  ( -24.49584582974870628, -12.46528025919705485, 73.49871492906470394 ) ) ;
#15326 = ORIENTED_EDGE ( 'NONE', *, *, #42888, .T. ) ;
#15327 = CARTESIAN_POINT ( 'NONE',  ( -24.71393967724174345, -16.34927462137609311, 59.23677039840046632 ) ) ;
#15328 = CYLINDRICAL_SURFACE ( 'NONE', #23500, 0.1499999999999953315 ) ;
#15330 =( BOUNDED_CURVE ( )  B_SPLINE_CURVE ( 3, ( #158, #37798, #23284, #38037 ),
 .UNSPECIFIED., .F., .F. ) 
 B_SPLINE_CURVE_WITH_KNOTS ( ( 4, 4 ),
 ( 1.570796326794896780, 1.780235837034217505 ),
 .UNSPECIFIED. ) 
 CURVE ( )  GEOMETRIC_REPRESENTATION_ITEM ( )  RATIONAL_B_SPLINE_CURVE ( ( 1.000000000000000000, 0.9963479302455154896, 0.9963479302455154896, 1.000000000000000000 ) ) 
 REPRESENTATION_ITEM ( '' )  );
#15329 = DIRECTION ( 'NONE',  ( -3.071710424422018668E-17, 6.404604876783312462E-16, 1.000000000000000000 ) ) ;
#15331 = CARTESIAN_POINT ( 'NONE',  ( -23.73810165963432084, -18.76483127932742789, 69.40716580542252245 ) ) ;
#15332 = CARTESIAN_POINT ( 'NONE',  ( -20.93445280450092127, -20.86546091266223968, 62.18759423706340073 ) ) ;
#15333 = DIRECTION ( 'NONE',  ( 4.115385489419890895E-17, 0.9999954153791273948, 0.003028072113818697231 ) ) ;
#15334 = CARTESIAN_POINT ( 'NONE',  ( -18.08034385650551812, -6.424090610841176385, 49.80797279389978627 ) ) ;
#15335 = ORIENTED_EDGE ( 'NONE', *, *, #24615, .T. ) ;
#15336 = CARTESIAN_POINT ( 'NONE',  ( -24.31944129331298399, -13.32629719641017729, 63.24753052856355140 ) ) ;
#15337 = CARTESIAN_POINT ( 'NONE',  ( -14.29947512317492730, -8.480563224953527879, 63.94546151666516209 ) ) ;
#15338 = ORIENTED_EDGE ( 'NONE', *, *, #48321, .T. ) ;
#15339 = CYLINDRICAL_SURFACE ( 'NONE', #12690, 2.000000000000001776 ) ;
#15340 = CARTESIAN_POINT ( 'NONE',  ( -21.71159385759798965, -8.990409506049200417, 49.61344411288074951 ) ) ;
#15341 = CARTESIAN_POINT ( 'NONE',  ( -10.72017361938626934, -12.61779402817458973, 57.21368711609748203 ) ) ;
#15342 = B_SPLINE_CURVE_WITH_KNOTS ( 'NONE', 3,
 ( #47359, #43908, #39225, #38980, #5255, #46629, #20275, #35279, #28632, #1554 ),
 .UNSPECIFIED., .F., .F.,
 ( 4, 2, 2, 2, 4 ),
 ( 0.1272669073658351802, 0.2522669073463199574, 0.3772669073268047901, 0.5022669073072896229, 0.6272669072877743446 ),
 .UNSPECIFIED. ) ;
#15343 = VERTEX_POINT ( 'NONE', #42738 ) ;
#15344 = CARTESIAN_POINT ( 'NONE',  ( -10.37497030826117417, -14.69804335084345581, 71.32782692816427073 ) ) ;
#15345 = CARTESIAN_POINT ( 'NONE',  ( -28.42409385541305511, -6.359206544744109735, 54.49999999999997158 ) ) ;
#15346 = FACE_OUTER_BOUND ( 'NONE', #43681, .T. ) ;
#15347 = ORIENTED_EDGE ( 'NONE', *, *, #36521, .T. ) ;
#15348 = CARTESIAN_POINT ( 'NONE',  ( -13.58034385650551812, -6.424090610841176385, 49.80797279389977916 ) ) ;
#15349 = CARTESIAN_POINT ( 'NONE',  ( -23.80338573481879294, -11.80731802715296119, 59.76763678108634537 ) ) ;
#15350 = CARTESIAN_POINT ( 'NONE',  ( -17.01690395770326347, -19.47798354061844961, 49.52966884056656482 ) ) ;
#15351 = EDGE_CURVE ( 'NONE', #15973, #42844, #30690, .T. ) ;
#15352 = CARTESIAN_POINT ( 'NONE',  ( -15.48396703021662546, -7.615489166865526904, 70.72334449499163611 ) ) ;
#15353 = CARTESIAN_POINT ( 'NONE',  ( -21.29196722032537537, -20.70380199363842877, 72.53918572867779346 ) ) ;
#15354 = ORIENTED_EDGE ( 'NONE', *, *, #14743, .T. ) ;
#15355 = EDGE_LOOP ( 'NONE', ( #9598, #25280 ) ) ;
#15356 = AXIS2_PLACEMENT_3D ( 'NONE', #25850, #22166, #29058 ) ;
#15357 = CARTESIAN_POINT ( 'NONE',  ( -13.27409385650551599, -9.792211528768504536, 50.49490371617623197 ) ) ;
#15358 = CARTESIAN_POINT ( 'NONE',  ( -20.00308622248979162, -8.244632374337111713, 70.13611736960565679 ) ) ;
#15359 = CARTESIAN_POINT ( 'NONE',  ( -16.14284385650552167, -8.811426318492348031, 52.18089403414751359 ) ) ;
#15360 = DIRECTION ( 'NONE',  ( 0.9687793358424821033, -0.2479245821708680464, 0.000000000000000000 ) ) ;
#15361 = CARTESIAN_POINT ( 'NONE',  ( -10.23569597183452728, -12.85201410577908732, 67.99478283741052564 ) ) ;
#15362 = EDGE_CURVE ( 'NONE', #8151, #39153, #45477, .T. ) ;
#15363 = CARTESIAN_POINT ( 'NONE',  ( -18.28326045751188289, -21.81039776412065834, 72.58511189374844719 ) ) ;
#15364 = DIRECTION ( 'NONE',  ( -1.000000000000000000, -2.866981220435666553E-17, 0.000000000000000000 ) ) ;
#15365 = EDGE_LOOP ( 'NONE', ( #24927, #16096, #35126, #19587, #17772 ) ) ;
#15366 = CARTESIAN_POINT ( 'NONE',  ( -22.99430652176234702, -19.05128528775244234, 62.54334036401282049 ) ) ;
#15367 = ORIENTED_EDGE ( 'NONE', *, *, #46303, .F. ) ;
#15368 = EDGE_CURVE ( 'NONE', #4639, #12198, #29282, .T. ) ;
#15369 = LINE ( 'NONE', #7044, #45733 ) ;
#15370 = CARTESIAN_POINT ( 'NONE',  ( -15.70730708645226237, -24.91091750872855215, 53.49999999999995026 ) ) ;
#15371 = CARTESIAN_POINT ( 'NONE',  ( -24.41897151118743636, -17.37347349776957017, 69.59835227440868266 ) ) ;
#15372 = CARTESIAN_POINT ( 'NONE',  ( -10.42546210075913748, -12.25520342886974845, 57.44361899967025664 ) ) ;
#15373 = ORIENTED_EDGE ( 'NONE', *, *, #46653, .F. ) ;
#15374 = DIRECTION ( 'NONE',  ( 3.071710424422018668E-17, -6.404604876783312462E-16, -1.000000000000000000 ) ) ;
#15375 = LINE ( 'NONE', #34104, #13966 ) ;
#15376 = EDGE_CURVE ( 'NONE', #2848, #13213, #32453, .T. ) ;
#15377 = CARTESIAN_POINT ( 'NONE',  ( -19.36122378369438835, -7.615284416629393149, 60.09946467050916397 ) ) ;
#15378 = CARTESIAN_POINT ( 'NONE',  ( -23.99312268326606201, -11.29471679256767125, 66.60709928216182618 ) ) ;
#15379 = ORIENTED_EDGE ( 'NONE', *, *, #19282, .F. ) ;
#15380 = DIRECTION ( 'NONE',  ( -5.215802026392426595E-06, 6.671378403414619972E-06, 0.9999999999641440152 ) ) ;
#15381 = CYLINDRICAL_SURFACE ( 'NONE', #36019, 0.1500000000000066835 ) ;
#15382 = FACE_OUTER_BOUND ( 'NONE', #14969, .T. ) ;
#15383 = CIRCLE ( 'NONE', #21693, 1.249999999999999334 ) ;
#15384 = FACE_BOUND ( 'NONE', #16372, .T. ) ;
#15385 = ITEM_DEFINED_TRANSFORMATION ( 'NONE', 'NONE', #5428,  #29031 ) ;
#15386 = ORIENTED_EDGE ( 'NONE', *, *, #18933, .F. ) ;
#15387 = DIRECTION ( 'NONE',  ( 2.842893050599252319E-07, -1.090087279701840163E-07, 0.9999999999999535927 ) ) ;
#15388 = CARTESIAN_POINT ( 'NONE',  ( -14.60689764421331738, -8.346551857622415582, 63.78978840692987262 ) ) ;
#15389 = CARTESIAN_POINT ( 'NONE',  ( -16.00544582274271477, -7.903112417841744453, 63.95538887075813506 ) ) ;
#15390 = ORIENTED_EDGE ( 'NONE', *, *, #37535, .F. ) ;
#15391 = CARTESIAN_POINT ( 'NONE',  ( -10.44483711275296933, -14.26928301035353819, 64.38803882970550774 ) ) ;
#15392 = VERTEX_POINT ( 'NONE', #46432 ) ;
#15393 = CARTESIAN_POINT ( 'NONE',  ( -12.27038830856583296, -10.07030047048361077, 64.25744141247331243 ) ) ;
#15394 = CARTESIAN_POINT ( 'NONE',  ( -27.42409385541305511, -25.10920654474410441, 81.99999999999998579 ) ) ;
#15396 = EDGE_CURVE ( 'NONE', #19337, #26266, #33657, .T. ) ;
#15395 = LINE ( 'NONE', #18609, #47148 ) ;
#15397 = ORIENTED_EDGE ( 'NONE', *, *, #45246, .F. ) ;
#15398 = ADVANCED_FACE ( 'NONE', ( #8509 ), #4336, .T. ) ;
#15399 = CARTESIAN_POINT ( 'NONE',  ( -22.46373187589079379, -16.28044704940516496, 50.77966884056655772 ) ) ;
#15400 = ORIENTED_EDGE ( 'NONE', *, *, #10769, .T. ) ;
#15401 = ADVANCED_FACE ( 'NONE', ( #32135 ), #30599, .T. ) ;
#15402 = EDGE_LOOP ( 'NONE', ( #21374, #44757, #40732, #26712 ) ) ;
#15403 = ORIENTED_EDGE ( 'NONE', *, *, #39745, .T. ) ;
#15404 = CARTESIAN_POINT ( 'NONE',  ( -20.25191534917340874, -8.350868906188830820, 70.26572394742477456 ) ) ;
#15405 = CARTESIAN_POINT ( 'NONE',  ( -22.80983080810246832, -13.62945529097500419, 53.69233794759167466 ) ) ;
#15406 = CARTESIAN_POINT ( 'NONE',  ( -12.56171917241870695, -20.45376946399996854, 71.99148991968543498 ) ) ;
#15407 = CARTESIAN_POINT ( 'NONE',  ( -20.60788153932096023, -8.518722016582884748, 63.32593600985608617 ) ) ;
#15408 = CARTESIAN_POINT ( 'NONE',  ( -19.14909385541296061, -8.112991634885936776, 51.74999426922435219 ) ) ;
#15409 = CARTESIAN_POINT ( 'NONE',  ( -12.69763806180496601, -20.04058448603118592, 68.62185382311069759 ) ) ;
#15410 = CARTESIAN_POINT ( 'NONE',  ( -12.50776634899986384, -20.40684016789016297, 71.92158251742569064 ) ) ;
#15411 = ORIENTED_EDGE ( 'NONE', *, *, #19637, .T. ) ;
#15412 = EDGE_LOOP ( 'NONE', ( #34231, #22287, #31036, #6822 ) ) ;
#15413 = FACE_OUTER_BOUND ( 'NONE', #31091, .T. ) ;
#15414 = B_SPLINE_CURVE_WITH_KNOTS ( 'NONE', 3,
 ( #22989, #33791, #44656, #7723, #18528, #88, #19031, #26670, #37975, #26184 ),
 .UNSPECIFIED., .F., .F.,
 ( 4, 2, 2, 2, 4 ),
 ( 0.1272669073658270200, 0.2522669073463124079, 0.3772669073267977957, 0.5022669073072831836, 0.6272669072877685714 ),
 .UNSPECIFIED. ) ;
#15415 = DIRECTION ( 'NONE',  ( 0.000000000000000000, 1.000000000000000000, 0.000000000000000000 ) ) ;
#15416 = CARTESIAN_POINT ( 'NONE',  ( -10.50673370502780557, -15.88996622876637588, 68.04938193442052352 ) ) ;
#15417 = CARTESIAN_POINT ( 'NONE',  ( -23.52687218415512760, -18.35477548540580273, 69.44938804596051796 ) ) ;
#15418 = ORIENTED_EDGE ( 'NONE', *, *, #2927, .T. ) ;
#15419 = CARTESIAN_POINT ( 'NONE',  ( -14.81784385650551528, -9.790100578890868377, 49.79778022625163203 ) ) ;
#15420 = AXIS2_PLACEMENT_3D ( 'NONE', #6430, #32981, #36920 ) ;
#15421 = AXIS2_PLACEMENT_3D ( 'NONE', #8314, #34641, #4866 ) ;
#15422 = EDGE_LOOP ( 'NONE', ( #9169, #31107, #44228, #11254, #38803 ) ) ;
#15423 = CARTESIAN_POINT ( 'NONE',  ( -11.71918404020638427, -18.95175453447548009, 71.70158022526054253 ) ) ;
#15424 = DIRECTION ( 'NONE',  ( 3.071710424422018668E-17, -6.404604876783312462E-16, -1.000000000000000000 ) ) ;
#15425 = FACE_OUTER_BOUND ( 'NONE', #5584, .T. ) ;
#15426 = VERTEX_POINT ( 'NONE', #40003 ) ;
#15427 = FACE_OUTER_BOUND ( 'NONE', #43975, .T. ) ;
#15428 = ADVANCED_FACE ( 'NONE', ( #20808 ), #6024, .F. ) ;
#15429 = CARTESIAN_POINT ( 'NONE',  ( -13.97958029355460852, -17.98703734140009303, 49.52966884056656482 ) ) ;
#15430 = CARTESIAN_POINT ( 'NONE',  ( -13.01616685277437568, -9.306763517318225709, 70.86397465682092900 ) ) ;
#15431 = ADVANCED_FACE ( 'NONE', ( #21047 ), #43223, .T. ) ;
#15432 = ORIENTED_EDGE ( 'NONE', *, *, #6809, .F. ) ;
#15433 = LINE ( 'NONE', #37358, #12380 ) ;
#15434 = LINE ( 'NONE', #7605, #18898 ) ;
#15435 = CARTESIAN_POINT ( 'NONE',  ( -23.98503169607928953, -17.39005800936845603, 66.22885190747201989 ) ) ;
#15436 = ORIENTED_EDGE ( 'NONE', *, *, #2845, .F. ) ;
#15437 = CARTESIAN_POINT ( 'NONE',  ( -12.25434508901797770, -20.17367074759813406, 65.05170324716399932 ) ) ;
#15438 = ORIENTED_EDGE ( 'NONE', *, *, #38567, .T. ) ;
#15439 = CARTESIAN_POINT ( 'NONE',  ( -24.72409385541305582, -14.90920654474413709, 60.91764705882351905 ) ) ;
#15440 = CARTESIAN_POINT ( 'NONE',  ( -14.93181132608235195, -7.787654600965993268, 57.03655263075181381 ) ) ;
#15441 = VERTEX_POINT ( 'NONE', #6272 ) ;
#15442 = CARTESIAN_POINT ( 'NONE',  ( -13.06813783877040969, -9.265530354883374287, 67.66470656304637998 ) ) ;
#15443 = CARTESIAN_POINT ( 'NONE',  ( -23.84087125894599168, -12.00869244310661266, 59.71065521759481953 ) ) ;
#15444 = CARTESIAN_POINT ( 'NONE',  ( -10.57487349103886132, -17.90974545538605867, 53.76227901944324117 ) ) ;
#15445 = ORIENTED_EDGE ( 'NONE', *, *, #4853, .T. ) ;
#15446 = DIRECTION ( 'NONE',  ( -2.872222159185455981E-06, 2.507089443456002334E-06, 0.9999999999927324801 ) ) ;
#15447 =( BOUNDED_CURVE ( )  B_SPLINE_CURVE ( 3, ( #39657, #35468, #35699, #27845 ),
 .UNSPECIFIED., .F., .F. ) 
 B_SPLINE_CURVE_WITH_KNOTS ( ( 4, 4 ),
 ( 0.5000000000000000000, 0.9074455897393628456 ),
 .UNSPECIFIED. ) 
 CURVE ( )  GEOMETRIC_REPRESENTATION_ITEM ( )  RATIONAL_B_SPLINE_CURVE ( ( 0.9999999999999765743, 0.4567392136813410164, 0.3561768502900499178, 0.6983129098260780765 ) ) 
 REPRESENTATION_ITEM ( '' )  );
#15448 = CARTESIAN_POINT ( 'NONE',  ( -22.25907719862886935, -19.87120158787481117, 65.98956406266549379 ) ) ;
#15449 = DIRECTION ( 'NONE',  ( -3.071710424422018668E-17, 6.404604876783312462E-16, 1.000000000000000000 ) ) ;
#15450 = VERTEX_POINT ( 'NONE', #9496 ) ;
#15451 = CARTESIAN_POINT ( 'NONE',  ( -23.83043768205027035, -11.86620487761972420, 59.63235732590894855 ) ) ;
#15452 = ADVANCED_FACE ( 'NONE', ( #32612 ), #1851, .F. ) ;
#15453 = AXIS2_PLACEMENT_3D ( 'NONE', #12334, #13045, #28076 ) ;
#15454 = VECTOR ( 'NONE', #5759, 1000.000000000000000 ) ;
#15455 = CARTESIAN_POINT ( 'NONE',  ( -21.73229268148169879, -8.731123941674052702, 70.17486588183628271 ) ) ;
#15456 = EDGE_CURVE ( 'NONE', #41019, #32914, #47834, .T. ) ;
#15457 = EDGE_CURVE ( 'NONE', #36238, #38209, #9157, .T. ) ;
#15458 = EDGE_CURVE ( 'NONE', #25120, #20357, #35600, .T. ) ;
#15459 = VERTEX_POINT ( 'NONE', #47874 ) ;
#15460 = ORIENTED_EDGE ( 'NONE', *, *, #19326, .F. ) ;
#15461 = CARTESIAN_POINT ( 'NONE',  ( -24.85185494555865660, -14.23383234075676640, 69.75301023497073061 ) ) ;
#15462 = CARTESIAN_POINT ( 'NONE',  ( -24.02419424914158341, -17.29788473263632298, 73.18336065054975847 ) ) ;
#15463 = CARTESIAN_POINT ( 'NONE',  ( -23.16117746674104438, -18.90708040007733359, 62.63934749780565880 ) ) ;
#15464 = AXIS2_PLACEMENT_3D ( 'NONE', #22576, #7568, #45011 ) ;
#15465 = CARTESIAN_POINT ( 'NONE',  ( -22.69284385650552238, -7.406986770994973490, 48.81910596585309747 ) ) ;
#15466 = CARTESIAN_POINT ( 'NONE',  ( -12.45759248923961060, -19.74223015388843194, 61.68213320638649577 ) ) ;
#15467 = CARTESIAN_POINT ( 'NONE',  ( -12.14795427363658575, -9.549397679475163159, 57.28273822603964049 ) ) ;
#15468 = DIRECTION ( 'NONE',  ( -3.071710424422018668E-17, 6.404604876783312462E-16, 1.000000000000000000 ) ) ;
#15469 =( BOUNDED_SURFACE ( )  B_SPLINE_SURFACE ( 3, 1, ( 
 ( #40604, #6889 ),
 ( #32739, #21902 ),
 ( #36905, #2701 ),
 ( #47299, #35945 ),
 ( #13533, #39653 ),
 ( #5924, #36185 ),
 ( #6410, #2471 ) ),
 .UNSPECIFIED., .T., .F., .F. ) 
 B_SPLINE_SURFACE_WITH_KNOTS ( ( 4, 3, 4 ),
 ( 2, 2 ),
 ( 0.000000000000000000, 0.5000000000000000000, 1.000000000000000000 ),
 ( 0.000000000000000000, 1.000000000000000000 ),
 .UNSPECIFIED. ) 
 GEOMETRIC_REPRESENTATION_ITEM ( )  RATIONAL_B_SPLINE_SURFACE ( (
 ( 1.000000000000000000, 1.000000000000000000),
 ( 0.3333333333333335369, 0.3333333333333330373),
 ( 0.3333333333333335369, 0.3333333333333330373),
 ( 1.000000000000000000, 1.000000000000000000),
 ( 0.3333333333333333703, 0.3333333333333333703),
 ( 0.3333333333333333703, 0.3333333333333333703),
 ( 1.000000000000000000, 1.000000000000000000) ) ) 
 REPRESENTATION_ITEM ( '' )  SURFACE ( )  );
#15470 = FACE_OUTER_BOUND ( 'NONE', #12050, .T. ) ;
#15471 = ORIENTED_EDGE ( 'NONE', *, *, #35779, .T. ) ;
#15472 = B_SPLINE_CURVE_WITH_KNOTS ( 'NONE', 1,
 ( #48253, #39910 ),
 .UNSPECIFIED., .F., .F.,
 ( 2, 2 ),
 ( 0.000000000000000000, 1.000000000000000000 ),
 .UNSPECIFIED. ) ;
#15473 = DIRECTION ( 'NONE',  ( 1.149299188226319421E-05, -1.849289876324834950E-06, 0.9999999999322456423 ) ) ;
#15474 = CARTESIAN_POINT ( 'NONE',  ( -21.85546194014773391, -9.390365834825972868, 59.94844577305733679 ) ) ;
#15475 = EDGE_LOOP ( 'NONE', ( #15963, #36303, #33127, #23703, #20995 ) ) ;
#15476 =( BOUNDED_CURVE ( )  B_SPLINE_CURVE ( 3, ( #5559, #40001, #43219, #13635 ),
 .UNSPECIFIED., .F., .F. ) 
 B_SPLINE_CURVE_WITH_KNOTS ( ( 4, 4 ),
 ( 0.5000000000000000000, 0.9074455897393666204 ),
 .UNSPECIFIED. ) 
 CURVE ( )  GEOMETRIC_REPRESENTATION_ITEM ( )  RATIONAL_B_SPLINE_CURVE ( ( 0.9999999999999905631, 0.4567392136813254178, 0.3561768502900344302, 0.6983129098261073864 ) ) 
 REPRESENTATION_ITEM ( '' )  );
#15477 = VERTEX_POINT ( 'NONE', #24267 ) ;
#15478 = EDGE_CURVE ( 'NONE', #43051, #45493, #21472, .T. ) ;
#15479 = CARTESIAN_POINT ( 'NONE',  ( -16.20683463515880973, -21.70255690700738782, 58.28585572422844052 ) ) ;
#15480 = CARTESIAN_POINT ( 'NONE',  ( -21.32332200014554857, -12.20934075487643966, 49.52966884056655772 ) ) ;
#15481 = CARTESIAN_POINT ( 'NONE',  ( -22.06477193427564387, -8.981018767459000074, 63.23507824025425350 ) ) ;
#15482 = CARTESIAN_POINT ( 'NONE',  ( -10.18577798186947625, -13.04535695669732220, 71.33111718294915704 ) ) ;
#15483 = VERTEX_POINT ( 'NONE', #14108 ) ;
#15484 = CARTESIAN_POINT ( 'NONE',  ( -13.72409385759798894, -9.359200813967568422, 50.49621490985803263 ) ) ;
#15485 = AXIS2_PLACEMENT_3D ( 'NONE', #38433, #15287, #22459 ) ;
#15486 = VECTOR ( 'NONE', #45581, 1000.000000000000000 ) ;
#15487 = CARTESIAN_POINT ( 'NONE',  ( -13.46273918380367185, -8.972896482542827457, 64.20946814027203686 ) ) ;
#15488 = ORIENTED_EDGE ( 'NONE', *, *, #7580, .T. ) ;
#15489 = EDGE_CURVE ( 'NONE', #23907, #21434, #29161, .T. ) ;
#15490 = AXIS2_PLACEMENT_3D ( 'NONE', #36032, #25451, #13620 ) ;
#15491 = CARTESIAN_POINT ( 'NONE',  ( -20.19231683483797113, -8.325423577284544407, 70.55100341277886855 ) ) ;
#15492 = B_SPLINE_CURVE_WITH_KNOTS ( 'NONE', 1,
 ( #22812, #3847 ),
 .UNSPECIFIED., .F., .F.,
 ( 2, 2 ),
 ( 0.000000000000000000, 1.000000000000000000 ),
 .UNSPECIFIED. ) ;
#15493 = DIRECTION ( 'NONE',  ( -3.413470714839332458E-33, 1.190614954331866791E-16, -1.000000000000000000 ) ) ;
#15494 = EDGE_LOOP ( 'NONE', ( #31623, #37571, #13676, #24271, #4395 ) ) ;
#15495 = FACE_OUTER_BOUND ( 'NONE', #18830, .T. ) ;
#15496 = ORIENTED_EDGE ( 'NONE', *, *, #28302, .T. ) ;
#15497 = CARTESIAN_POINT ( 'NONE',  ( -18.50932193227059486, -21.77517953109191140, 72.58510940649487964 ) ) ;
#15498 = FACE_OUTER_BOUND ( 'NONE', #14703, .T. ) ;
#15499 = ORIENTED_EDGE ( 'NONE', *, *, #40586, .T. ) ;
#15500 = CARTESIAN_POINT ( 'NONE',  ( -13.41424841794075462, -8.530288970272771110, 57.22613703607469660 ) ) ;
#15501 = CARTESIAN_POINT ( 'NONE',  ( -13.88293259567353743, -20.90532631576516565, 68.45625136994867432 ) ) ;
#15502 = CARTESIAN_POINT ( 'NONE',  ( -20.30534385650551599, -8.801233750844183135, 48.81488406609782515 ) ) ;
#15503 = CARTESIAN_POINT ( 'NONE',  ( -17.72419722990865054, -21.80277058550420577, 58.40553378253839156 ) ) ;
#15504 = CARTESIAN_POINT ( 'NONE',  ( -18.78584198798900928, -7.883846953673406155, 63.58656136513857149 ) ) ;
#15505 = CARTESIAN_POINT ( 'NONE',  ( -22.40225758545279788, -19.80633875317364456, 65.91241718764763391 ) ) ;
#15506 = ORIENTED_EDGE ( 'NONE', *, *, #8917, .T. ) ;
#15507 = CARTESIAN_POINT ( 'NONE',  ( -15.26018413780878724, -21.51894302366104483, 68.57592926692872481 ) ) ;
#15508 = DIRECTION ( 'NONE',  ( -0.3478314405900309603, -0.9375570856950864451, 0.000000000000000000 ) ) ;
#15509 = DIRECTION ( 'NONE',  ( 5.854827030937197869E-31, 1.020425574103664912E-16, 1.000000000000000000 ) ) ;
#15510 = DIRECTION ( 'NONE',  ( -0.000000000000000000, -1.000000000000000000, -0.000000000000000000 ) ) ;
#15511 = DIRECTION ( 'NONE',  ( 3.549360974554993999E-17, -6.371834667797928663E-18, -1.000000000000000000 ) ) ;
#15512 = EDGE_CURVE ( 'NONE', #5832, #32391, #4141, .T. ) ;
#15513 = EDGE_CURVE ( 'NONE', #34444, #14112, #17612, .T. ) ;
#15514 = ORIENTED_EDGE ( 'NONE', *, *, #36337, .T. ) ;
#15515 = VERTEX_POINT ( 'NONE', #44931 ) ;
#15516 = APPLICATION_CONTEXT ( 'automotive_design' ) ;
#15517 = CARTESIAN_POINT ( 'NONE',  ( -13.60167271156757707, -11.21037387301822363, 49.52966884056655772 ) ) ;
#15518 = CARTESIAN_POINT ( 'NONE',  ( -10.34868689528060060, -12.47656361335272734, 60.99864767591832049 ) ) ;
#15519 = EDGE_LOOP ( 'NONE', ( #22686, #45541, #19870, #16047, #6446 ) ) ;
#15520 = CARTESIAN_POINT ( 'NONE',  ( -12.81525634688827786, -20.14415600020443264, 72.10653672084445986 ) ) ;
#15521 = CARTESIAN_POINT ( 'NONE',  ( -15.19548991633585011, -21.91815178685365595, 68.76088227238139439 ) ) ;
#15522 = CARTESIAN_POINT ( 'NONE',  ( -10.26942273409980722, -12.73178763592770579, 64.40689592259661822 ) ) ;
#15523 = CARTESIAN_POINT ( 'NONE',  ( -10.46600813091865412, -15.57464811048514619, 57.79466158264115450 ) ) ;
#15524 = B_SPLINE_CURVE_WITH_KNOTS ( 'NONE', 3,
 ( #44507, #28522, #6827, #7081, #36839, #3126, #22094, #3370, #10043, #13710 ),
 .UNSPECIFIED., .F., .F.,
 ( 4, 2, 2, 2, 4 ),
 ( 0.6272669072878274132, 0.7522669073073278145, 0.8772669073268283269, 1.002266907346328839, 1.127266907365829240 ),
 .UNSPECIFIED. ) ;
#15525 = CARTESIAN_POINT ( 'NONE',  ( -14.36817892824948650, -8.455618309860652104, 67.54503025475185041 ) ) ;
#15526 = CARTESIAN_POINT ( 'NONE',  ( -19.59054600911842670, -21.93742321824504415, 62.13357111270039468 ) ) ;
#15527 = AXIS2_PLACEMENT_3D ( 'NONE', #4250, #15543, #27617 ) ;
#15528 = DIRECTION ( 'NONE',  ( -3.071710424422018668E-17, 6.404604876783312462E-16, 1.000000000000000000 ) ) ;
#15529 = AXIS2_PLACEMENT_3D ( 'NONE', #43272, #1892, #27988 ) ;
#15530 = EDGE_CURVE ( 'NONE', #28527, #7211, #34303, .T. ) ;
#15531 = EDGE_CURVE ( 'NONE', #32823, #17138, #25822, .T. ) ;
#15532 = FACE_OUTER_BOUND ( 'NONE', #25507, .T. ) ;
#15533 =( LENGTH_UNIT ( ) NAMED_UNIT ( * ) SI_UNIT ( .MILLI., .METRE. ) );
#15534 = ADVANCED_FACE ( 'NONE', ( #7745 ), #37750, .T. ) ;
#15535 = CARTESIAN_POINT ( 'NONE',  ( -20.98629261354270170, -17.87291272402722342, 52.02966884056656482 ) ) ;
#15536 = VECTOR ( 'NONE', #41696, 1000.000000000000000 ) ;
#15537 = CARTESIAN_POINT ( 'NONE',  ( -13.79232177786185432, -20.79486811282113123, 68.52795486457198137 ) ) ;
#15538 = CARTESIAN_POINT ( 'NONE',  ( -19.92776479198160189, -21.39998277484045275, 72.41950795000725805 ) ) ;
#15539 = FACE_OUTER_BOUND ( 'NONE', #9847, .T. ) ;
#15540 = VECTOR ( 'NONE', #17940, 1000.000000000000000 ) ;
#15541 = ORIENTED_EDGE ( 'NONE', *, *, #30697, .F. ) ;
#15542 = ORIENTED_EDGE ( 'NONE', *, *, #38444, .F. ) ;
#15543 = DIRECTION ( 'NONE',  ( 0.7107718805962432995, 0.7034225854731135374, 7.722840060723789693E-09 ) ) ;
#15544 = VERTEX_POINT ( 'NONE', #15092 ) ;
#15545 = EDGE_CURVE ( 'NONE', #29624, #8171, #48491, .T. ) ;
#15546 = CARTESIAN_POINT ( 'NONE',  ( -17.42409385541299471, -14.80920654474435771, 49.52966884056655772 ) ) ;
#15547 = CARTESIAN_POINT ( 'NONE',  ( -10.38863864971416184, -14.24588297309210816, 57.60391932725825370 ) ) ;
#15548 = CARTESIAN_POINT ( 'NONE',  ( -11.26665320750704602, -11.47952451810412455, 64.43416648033296212 ) ) ;
#15549 = CARTESIAN_POINT ( 'NONE',  ( -10.40888601095206312, -14.10966482229656194, 61.21821293885882653 ) ) ;
#15550 = ORIENTED_EDGE ( 'NONE', *, *, #3491, .F. ) ;
#15551 = CARTESIAN_POINT ( 'NONE',  ( -16.01976337179375776, -7.492708285372152943, 63.77736896427055058 ) ) ;
#15552 = AXIS2_PLACEMENT_3D ( 'NONE', #996, #33982, #11838 ) ;
#15553 = CARTESIAN_POINT ( 'NONE',  ( -18.55557756536243375, -7.850556297346193979, 73.84064430960019365 ) ) ;
#15554 = CIRCLE ( 'NONE', #22681, 2.000000000000001776 ) ;
#15555 = ORIENTED_EDGE ( 'NONE', *, *, #4313, .T. ) ;
#15556 = CARTESIAN_POINT ( 'NONE',  ( -24.45577199812615632, -12.20047074031916168, 53.49999999999994316 ) ) ;
#15557 = VECTOR ( 'NONE', #16790, 1000.000000000000000 ) ;
#15558 = CIRCLE ( 'NONE', #47848, 2.000000000000001332 ) ;
#15559 = ORIENTED_EDGE ( 'NONE', *, *, #26105, .F. ) ;
#15560 = CARTESIAN_POINT ( 'NONE',  ( -23.24415167771102020, -18.79314401478295338, 62.23918030722157368 ) ) ;
#15561 = CARTESIAN_POINT ( 'NONE',  ( -22.17715676677442715, -20.54607711729781983, 58.87168751005452805 ) ) ;
#15562 = CARTESIAN_POINT ( 'NONE',  ( -24.04524516174978643, -12.53718734719852002, 73.24225551612813945 ) ) ;
#15563 = ORIENTED_EDGE ( 'NONE', *, *, #873, .F. ) ;
#15564 = DIRECTION ( 'NONE',  ( -2.584300828889512628E-08, -1.497441464807615962E-06, 0.9999999999988784527 ) ) ;
#15565 = CARTESIAN_POINT ( 'NONE',  ( -11.67943375510494874, -18.89645239624664796, 68.50217487844219022 ) ) ;
#15566 = VECTOR ( 'NONE', #45232, 1000.000000000000000 ) ;
#15567 = ADVANCED_FACE ( 'NONE', ( #48595 ), #37566, .T. ) ;
#15568 = CARTESIAN_POINT ( 'NONE',  ( -14.54969778468464270, -21.68242161614711705, 58.35956174891157389 ) ) ;
#15569 = CARTESIAN_POINT ( 'NONE',  ( -24.17147434587301191, -12.75550446831573126, 73.65714286828524848 ) ) ;
#15570 = ORIENTED_EDGE ( 'NONE', *, *, #20444, .T. ) ;
#15571 = FACE_OUTER_BOUND ( 'NONE', #29875, .T. ) ;
#15572 = DIRECTION ( 'NONE',  ( 0.9687793358424821033, -0.2479245821708680464, 0.000000000000000000 ) ) ;
#15573 = CARTESIAN_POINT ( 'NONE',  ( -19.25408589567127038, -10.49476435801948071, 49.52966884056655772 ) ) ;
#15574 = LINE ( 'NONE', #38479, #32926 ) ;
#15575 = CARTESIAN_POINT ( 'NONE',  ( -22.58588533274201282, -20.18224782263116523, 69.36073240021890740 ) ) ;
#15576 = CARTESIAN_POINT ( 'NONE',  ( -20.61159385650551812, -6.922745924619793101, 51.69366785382590024 ) ) ;
#15577 = ADVANCED_FACE ( 'NONE', ( #19049 ), #40971, .T. ) ;
#15578 = EDGE_LOOP ( 'NONE', ( #14179, #16781, #29208, #39346 ) ) ;
#15579 = DIRECTION ( 'NONE',  ( -3.071710424422018668E-17, 6.404604876783312462E-16, 1.000000000000000000 ) ) ;
#15580 = CARTESIAN_POINT ( 'NONE',  ( -24.26085839341466155, -16.31265863350449408, 59.42332382718851136 ) ) ;
#15581 = ORIENTED_EDGE ( 'NONE', *, *, #9280, .F. ) ;
#15582 = DIRECTION ( 'NONE',  ( -0.03181436478788691319, -0.9994937949748079475, -6.982004198809111150E-09 ) ) ;
#15583 = ADVANCED_BREP_SHAPE_REPRESENTATION ( '', ( #76, #29031 ), #42412 ) ;
#15584 = CARTESIAN_POINT ( 'NONE',  ( -45.50908060261262023, -14.20920654474410760, 70.87000000000000455 ) ) ;
#15585 = CARTESIAN_POINT ( 'NONE',  ( -14.60831034098102066, -21.21965606200325993, 58.27690872140736644 ) ) ;
#15586 = B_SPLINE_CURVE_WITH_KNOTS ( 'NONE', 1,
 ( #27992, #9057 ),
 .UNSPECIFIED., .F., .F.,
 ( 2, 2 ),
 ( 0.000000000000000000, 1.000000000000000000 ),
 .UNSPECIFIED. ) ;
#15587 = VERTEX_POINT ( 'NONE', #7499 ) ;
#15588 = CARTESIAN_POINT ( 'NONE',  ( -25.31403878743076774, -21.34684298153750603, 53.49999999999995026 ) ) ;
#15589 = CARTESIAN_POINT ( 'NONE',  ( -16.79871736827016449, -7.783984993247369921, 73.84529564069914898 ) ) ;
#15590 = EDGE_CURVE ( 'NONE', #1214, #12470, #37457, .T. ) ;
#15591 = CARTESIAN_POINT ( 'NONE',  ( -10.66160605790631344, -13.00123564105898666, 68.03832347539896830 ) ) ;
#15592 = ORIENTED_EDGE ( 'NONE', *, *, #23072, .F. ) ;
#15593 = CARTESIAN_POINT ( 'NONE',  ( -16.16784385650552025, -6.428312510596451368, 51.20221977374900035 ) ) ;
#15594 = ADVANCED_FACE ( 'NONE', ( #45172 ), #22668, .T. ) ;
#15595 = VECTOR ( 'NONE', #35571, 1000.000000000000000 ) ;
#15596 = EDGE_CURVE ( 'NONE', #1510, #14770, #8869, .T. ) ;
#15597 = CYLINDRICAL_SURFACE ( 'NONE', #19313, 0.3999999999999978018 ) ;
#15598 = AXIS2_PLACEMENT_3D ( 'NONE', #11011, #42024, #23311 ) ;
#15599 = CARTESIAN_POINT ( 'NONE',  ( -24.80132792067086811, -15.84796731252138180, 69.73318694624859404 ) ) ;
#15600 = CARTESIAN_POINT ( 'NONE',  ( -14.02608879878888182, -8.179082098857648475, 70.86811127254848941 ) ) ;
#15601 = CARTESIAN_POINT ( 'NONE',  ( -23.08260857892799578, -18.93003297495478776, 62.35406880915004280 ) ) ;
#15602 = VECTOR ( 'NONE', #8961, 1000.000000000000000 ) ;
#15603 = AXIS2_PLACEMENT_3D ( 'NONE', #47637, #10218, #28678 ) ;
#15604 = ORIENTED_EDGE ( 'NONE', *, *, #34953, .F. ) ;
#15605 = EDGE_LOOP ( 'NONE', ( #46800, #33448 ) ) ;
#15606 = CARTESIAN_POINT ( 'NONE',  ( -14.51159385650551492, -6.922745924619793101, 51.69366785382590024 ) ) ;
#15607 = CARTESIAN_POINT ( 'NONE',  ( -24.40329140489778936, -15.80613695201593671, 69.53307515782529435 ) ) ;
#15608 = DIRECTION ( 'NONE',  ( 0.6380325334150259708, -0.7700094066334539633, 0.000000000000000000 ) ) ;
#15609 = AXIS2_PLACEMENT_3D ( 'NONE', #18350, #37297, #44983 ) ;
#15610 = CARTESIAN_POINT ( 'NONE',  ( -16.19792114999740562, -7.866354181730329742, 60.48556343814865954 ) ) ;
#15611 =( BOUNDED_SURFACE ( )  B_SPLINE_SURFACE ( 3, 1, ( 
 ( #24577, #47458 ),
 ( #28738, #47211 ),
 ( #39574, #13455 ),
 ( #31705, #46732 ),
 ( #9792, #5850 ),
 ( #21110, #35862 ),
 ( #17402, #10021 ) ),
 .UNSPECIFIED., .T., .F., .F. ) 
 B_SPLINE_SURFACE_WITH_KNOTS ( ( 4, 3, 4 ),
 ( 2, 2 ),
 ( 0.000000000000000000, 0.5000000000000000000, 1.000000000000000000 ),
 ( 0.000000000000000000, 1.000000000000000000 ),
 .UNSPECIFIED. ) 
 GEOMETRIC_REPRESENTATION_ITEM ( )  RATIONAL_B_SPLINE_SURFACE ( (
 ( 1.000000000000000000, 1.000000000000000000),
 ( 0.3333333333333335369, 0.3333333333333330373),
 ( 0.3333333333333335369, 0.3333333333333330373),
 ( 1.000000000000000000, 1.000000000000000000),
 ( 0.3333333333333333703, 0.3333333333333333703),
 ( 0.3333333333333333703, 0.3333333333333333703),
 ( 1.000000000000000000, 1.000000000000000000) ) ) 
 REPRESENTATION_ITEM ( '' )  SURFACE ( )  );
#15612 = CARTESIAN_POINT ( 'NONE',  ( -17.77920954038207668, -22.25082405446125122, 58.59048702730397196 ) ) ;
#15613 = CARTESIAN_POINT ( 'NONE',  ( -11.01408789448753822, -11.01258660117674104, 60.82885777859402054 ) ) ;
#15614 = CARTESIAN_POINT ( 'NONE',  ( -13.54822921233619226, -20.69819393533649077, 61.51646323540209949 ) ) ;
#15615 = VERTEX_POINT ( 'NONE', #23007 ) ;
#15616 = CARTESIAN_POINT ( 'NONE',  ( -12.21065591164131092, -19.56036527704336692, 61.48858610352198184 ) ) ;
#15617 = B_SPLINE_CURVE_WITH_KNOTS ( 'NONE', 3,
 ( #37507, #48603, #10467, #25963, #29170, #40982, #48123, #22026, #7265, #18554 ),
 .UNSPECIFIED., .F., .F.,
 ( 4, 2, 2, 2, 4 ),
 ( 0.1272669073658323213, 0.2522669073442346255, 0.3772669073226370129, 0.5022669073010392893, 0.6272669072794416767 ),
 .UNSPECIFIED. ) ;
#15618 =( BOUNDED_SURFACE ( )  B_SPLINE_SURFACE ( 3, 1, ( 
 ( #26649, #48311 ),
 ( #14543, #3261 ),
 ( #41664, #7216 ),
 ( #29861, #37214 ),
 ( #33773, #26166 ),
 ( #18510, #7955 ),
 ( #3749, #7706 ) ),
 .UNSPECIFIED., .T., .F., .F. ) 
 B_SPLINE_SURFACE_WITH_KNOTS ( ( 4, 3, 4 ),
 ( 2, 2 ),
 ( 0.000000000000000000, 0.5000000000000000000, 1.000000000000000000 ),
 ( 0.000000000000000000, 1.000000000000000000 ),
 .UNSPECIFIED. ) 
 GEOMETRIC_REPRESENTATION_ITEM ( )  RATIONAL_B_SPLINE_SURFACE ( (
 ( 1.000000000000000000, 1.000000000000000000),
 ( 0.3333333333333335369, 0.3333333333333330373),
 ( 0.3333333333333335369, 0.3333333333333330373),
 ( 1.000000000000000000, 1.000000000000000000),
 ( 0.3333333333333333703, 0.3333333333333333703),
 ( 0.3333333333333333703, 0.3333333333333333703),
 ( 1.000000000000000000, 1.000000000000000000) ) ) 
 REPRESENTATION_ITEM ( '' )  SURFACE ( )  );
#15619 = ORIENTED_EDGE ( 'NONE', *, *, #8682, .F. ) ;
#15620 = CARTESIAN_POINT ( 'NONE',  ( -12.52591642561268515, -9.195683996340104471, 74.50418400381258266 ) ) ;
#15621 = CARTESIAN_POINT ( 'NONE',  ( -15.07292840516123000, -21.45564092615730090, 65.10596683003562646 ) ) ;
#15622 = CARTESIAN_POINT ( 'NONE',  ( -24.42389991426342988, -17.36022673893785750, 69.55193308739468705 ) ) ;
#15623 = CARTESIAN_POINT ( 'NONE',  ( -20.75354924259569245, -21.52967727414722887, 47.99999999999994316 ) ) ;
#15624 = VERTEX_POINT ( 'NONE', #8947 ) ;
#15625 = CYLINDRICAL_SURFACE ( 'NONE', #35161, 0.3999999999999978018 ) ;
#15626 = AXIS2_PLACEMENT_3D ( 'NONE', #17210, #24865, #16725 ) ;
#15627 = CARTESIAN_POINT ( 'NONE',  ( -19.85909577874797449, -21.37257635846961890, 72.46322212860958700 ) ) ;
#15628 = PRODUCT_DEFINITION_FORMATION_WITH_SPECIFIED_SOURCE ( 'ANY', '', #859, .NOT_KNOWN. ) ;
#15629 = ADVANCED_FACE ( 'NONE', ( #46370 ), #4763, .T. ) ;
#15630 = DIRECTION ( 'NONE',  ( -3.413470714839332458E-33, 1.190614954331866791E-16, -1.000000000000000000 ) ) ;
#15631 = CARTESIAN_POINT ( 'NONE',  ( -19.36518065869528726, -8.031383756764064685, 59.97565108339750850 ) ) ;
#15632 = ORIENTED_EDGE ( 'NONE', *, *, #26673, .F. ) ;
#15633 = DIRECTION ( 'NONE',  ( -9.632611953450936153E-07, 3.816342149705755051E-07, 0.9999999999994632072 ) ) ;
#15634 = DIRECTION ( 'NONE',  ( 1.224646799147353207E-16, 1.000000000000000000, -1.912410701131276611E-32 ) ) ;
#15635 = AXIS2_PLACEMENT_3D ( 'NONE', #11139, #29360, #41409 ) ;
#15637 = LINE ( 'NONE', #20807, #10536 ) ;
#15636 = AXIS2_PLACEMENT_3D ( 'NONE', #46123, #27404, #42439 ) ;
#15638 = DIRECTION ( 'NONE',  ( 3.071710424422018668E-17, -6.404604876783312462E-16, -1.000000000000000000 ) ) ;
#15639 = VERTEX_POINT ( 'NONE', #8222 ) ;
#15640 = CARTESIAN_POINT ( 'NONE',  ( -24.74075724160099554, -16.21284971877490122, 62.77824058731629009 ) ) ;
#15641 = CARTESIAN_POINT ( 'NONE',  ( -14.08659385541286468, -7.222650657623884918, 49.61879703869455227 ) ) ;
#15642 = CARTESIAN_POINT ( 'NONE',  ( -50.42609385541305755, -14.80920654474415699, 62.92941176470587550 ) ) ;
#15643 = CARTESIAN_POINT ( 'NONE',  ( -15.95707318215220205, -7.504986700048139170, 63.85506303619484214 ) ) ;
#15644 = ORIENTED_EDGE ( 'NONE', *, *, #13673, .T. ) ;
#15645 = CARTESIAN_POINT ( 'NONE',  ( -10.58454466348024425, -16.55148359085594478, 71.60317204484042009 ) ) ;
#15646 = AXIS2_PLACEMENT_3D ( 'NONE', #7317, #22317, #22824 ) ;
#15647 = ORIENTED_EDGE ( 'NONE', *, *, #18095, .T. ) ;
#15648 = B_SPLINE_CURVE_WITH_KNOTS ( 'NONE', 1,
 ( #9110, #503 ),
 .UNSPECIFIED., .F., .F.,
 ( 2, 2 ),
 ( 0.000000000000000000, 1.000000000000000000 ),
 .UNSPECIFIED. ) ;
#15649 = CARTESIAN_POINT ( 'NONE',  ( -20.53534356219854118, -19.36092059621579509, 53.88362224778186516 ) ) ;
#15650 = CARTESIAN_POINT ( 'NONE',  ( -16.76012850172728719, -22.22957059519031020, 68.79537020757767607 ) ) ;
#15651 = ORIENTED_EDGE ( 'NONE', *, *, #38603, .F. ) ;
#15652 = DIRECTION ( 'NONE',  ( -3.413470714839332458E-33, 1.190614954331866791E-16, -1.000000000000000000 ) ) ;
#15653 = ORIENTED_EDGE ( 'NONE', *, *, #18291, .F. ) ;
#15654 = EDGE_LOOP ( 'NONE', ( #22186, #4338 ) ) ;
#15655 = VERTEX_POINT ( 'NONE', #38725 ) ;
#15656 = EDGE_CURVE ( 'NONE', #25645, #41118, #19288, .T. ) ;
#15657 = DIRECTION ( 'NONE',  ( 0.000000000000000000, 0.000000000000000000, 1.000000000000000000 ) ) ;
#15658 = CARTESIAN_POINT ( 'NONE',  ( -16.55451525393793233, -12.46531383050667863, 75.49999999999994316 ) ) ;
#15659 = ADVANCED_FACE ( 'NONE', ( #11658 ), #20020, .F. ) ;
#15660 = LINE ( 'NONE', #19612, #2743 ) ;
#15661 = CARTESIAN_POINT ( 'NONE',  ( -24.15197288150306321, -12.87620330113281497, 66.58781343342795367 ) ) ;
#15662 = CARTESIAN_POINT ( 'NONE',  ( -11.82099675438171005, -9.899106633794131582, 64.21409753874590365 ) ) ;
#15663 = CARTESIAN_POINT ( 'NONE',  ( -20.04909385541303024, -8.112991634885936776, 51.74999426922423851 ) ) ;
#15664 = ORIENTED_EDGE ( 'NONE', *, *, #21495, .T. ) ;
#15665 = ORIENTED_EDGE ( 'NONE', *, *, #45246, .T. ) ;
#15666 = EDGE_CURVE ( 'NONE', #21656, #19435, #42532, .T. ) ;
#15667 = CARTESIAN_POINT ( 'NONE',  ( -24.43827367352892210, -15.52193379869737377, 73.28831629023289906 ) ) ;
#15668 = DIRECTION ( 'NONE',  ( 0.3124635249310679930, 0.8422251632096489082, -0.4393441931380591692 ) ) ;
#15669 = AXIS2_PLACEMENT_3D ( 'NONE', #951, #37373, #33676 ) ;
#15670 = FACE_OUTER_BOUND ( 'NONE', #28595, .T. ) ;
#15671 = DIRECTION ( 'NONE',  ( -0.5497669574358330369, 0.8353180786453389128, 7.898837271846008747E-08 ) ) ;
#15672 = ORIENTED_EDGE ( 'NONE', *, *, #18878, .F. ) ;
#15673 = EDGE_CURVE ( 'NONE', #44868, #5874, #23482, .T. ) ;
#15674 = CARTESIAN_POINT ( 'NONE',  ( -14.42409385650551457, -6.426201560718813433, 50.50509628382439331 ) ) ;
#15675 = EDGE_CURVE ( 'NONE', #38891, #12034, #47550, .T. ) ;
#15676 = AXIS2_PLACEMENT_3D ( 'NONE', #48482, #21190, #3429 ) ;
#15677 = AXIS2_PLACEMENT_3D ( 'NONE', #33883, #17467, #41042 ) ;
#15678 = ORIENTED_EDGE ( 'NONE', *, *, #35148, .T. ) ;
#15679 = CARTESIAN_POINT ( 'NONE',  ( -17.42409385541299471, -14.80920654474435594, 52.02966884056656482 ) ) ;
#15680 = CARTESIAN_POINT ( 'NONE',  ( -15.37172156182068328, -21.50163546728593289, 68.59095364069538903 ) ) ;
#15681 = CARTESIAN_POINT ( 'NONE',  ( -10.02107422201081732, -13.96720754792729480, 57.56169656168945181 ) ) ;
#15682 = VERTEX_POINT ( 'NONE', #34538 ) ;
#15683 = DIRECTION ( 'NONE',  ( 1.224646799147353207E-16, 1.000000000000000000, -1.912410701131276611E-32 ) ) ;
#15684 = CARTESIAN_POINT ( 'NONE',  ( -12.36756753426621813, -9.896138138887707214, 57.37463480816234096 ) ) ;
#15685 = ORIENTED_EDGE ( 'NONE', *, *, #3819, .F. ) ;
#15686 = CARTESIAN_POINT ( 'NONE',  ( -10.44902896174112428, -15.40082452545022562, 57.56792826000953056 ) ) ;
#15687 = EDGE_CURVE ( 'NONE', #445, #41870, #39354, .T. ) ;
#15688 = DIRECTION ( 'NONE',  ( 3.071710424422018668E-17, -6.404604876783312462E-16, -1.000000000000000000 ) ) ;
#15689 = CARTESIAN_POINT ( 'NONE',  ( -12.36892846946874336, -20.28168252396862670, 68.43683184314359380 ) ) ;
#15690 = EDGE_LOOP ( 'NONE', ( #2337, #42465 ) ) ;
#15691 = DIRECTION ( 'NONE',  ( 2.191687980765842865E-06, -1.258878960415826265E-05, -0.9999999999183594168 ) ) ;
#15692 = EDGE_LOOP ( 'NONE', ( #38565, #12964, #22530, #13858 ) ) ;
#15693 = CARTESIAN_POINT ( 'NONE',  ( -10.57990114081760957, -13.11695186304741334, 71.22300718686659593 ) ) ;
#15694 = CARTESIAN_POINT ( 'NONE',  ( -14.73368791995220839, -7.861157911666011522, 56.96344736924808672 ) ) ;
#15695 = ORIENTED_EDGE ( 'NONE', *, *, #25095, .T. ) ;
#15696 = CARTESIAN_POINT ( 'NONE',  ( -10.83536383905390998, -17.31742040078651357, 64.62739380450889826 ) ) ;
#15697 = DIRECTION ( 'NONE',  ( -0.9979768094191902028, -0.06357898915123888495, 6.487762650558939457E-18 ) ) ;
#15698 = FACE_OUTER_BOUND ( 'NONE', #37868, .T. ) ;
#15699 = VECTOR ( 'NONE', #44418, 1000.000000000000000 ) ;
#15700 = ORIENTED_EDGE ( 'NONE', *, *, #27020, .T. ) ;
#15701 = DIRECTION ( 'NONE',  ( -3.071710424422018668E-17, 6.404604876783312462E-16, 1.000000000000000000 ) ) ;
#15702 = CARTESIAN_POINT ( 'NONE',  ( -16.30881325926348424, -7.898512564620374654, 60.50028524973911459 ) ) ;
#15703 = CARTESIAN_POINT ( 'NONE',  ( -11.95563469220200581, -9.749529029264454749, 60.73635005636825923 ) ) ;
#15704 = VERTEX_POINT ( 'NONE', #1290 ) ;
#15705 = EDGE_CURVE ( 'NONE', #31278, #41929, #8525, .T. ) ;
#15706 = CARTESIAN_POINT ( 'NONE',  ( -12.36756753426621813, -9.896138138887707214, 57.37463480816234096 ) ) ;
#15707 = CIRCLE ( 'NONE', #22846, 5.249999999999998224 ) ;
#15708 = DIRECTION ( 'NONE',  ( 0.3163880819683246859, 0.8528035521334704772, -0.4154812667942318627 ) ) ;
#15709 = EDGE_LOOP ( 'NONE', ( #9949, #19828, #6053, #46026, #31143 ) ) ;
#15710 = ORIENTED_EDGE ( 'NONE', *, *, #43023, .T. ) ;
#15711 = DIRECTION ( 'NONE',  ( 1.069388062422745569E-05, -2.778940570413862605E-06, -0.9999999999389592720 ) ) ;
#15712 = CARTESIAN_POINT ( 'NONE',  ( -24.07704370891654122, -17.14264987453632827, 72.89808101046213551 ) ) ;
#15713 = DIRECTION ( 'NONE',  ( -3.071710424422018668E-17, 6.404604876783312462E-16, 1.000000000000000000 ) ) ;
#15714 = AXIS2_PLACEMENT_3D ( 'NONE', #19063, #18309, #30165 ) ;
#15715 = CARTESIAN_POINT ( 'NONE',  ( -22.01784385650551812, -9.790100578890868377, 49.79778022625162492 ) ) ;
#15716 = CARTESIAN_POINT ( 'NONE',  ( -20.13271805750754595, -8.299978134201072777, 70.53628287813307907 ) ) ;
#15717 = CARTESIAN_POINT ( 'NONE',  ( -12.60227155074094441, -19.95281705956671559, 68.35129494334645983 ) ) ;
#15718 = LINE ( 'NONE', #5641, #45998 ) ;
#15719 = CARTESIAN_POINT ( 'NONE',  ( -9.974309423965010524, -14.87247496791766821, 74.90504757659225277 ) ) ;
#15720 = EDGE_LOOP ( 'NONE', ( #17273, #2673 ) ) ;
#15721 = EDGE_CURVE ( 'NONE', #26463, #20224, #15825, .T. ) ;
#15722 = CARTESIAN_POINT ( 'NONE',  ( -22.94192455449829993, -9.803488759991966006, 70.05532601532212311 ) ) ;
#15723 = ADVANCED_FACE ( 'NONE', ( #579 ), #45889, .T. ) ;
#15724 = CARTESIAN_POINT ( 'NONE',  ( -10.03292950473385403, -13.87467889623203554, 57.54801398733246742 ) ) ;
#15725 = EDGE_CURVE ( 'NONE', #25294, #47754, #16301, .T. ) ;
#15726 = CARTESIAN_POINT ( 'NONE',  ( -24.38152189803567538, -12.22801735019761793, 54.27143602781901421 ) ) ;
#15727 = ORIENTED_EDGE ( 'NONE', *, *, #20472, .F. ) ;
#15728 = VERTEX_POINT ( 'NONE', #27167 ) ;
#15729 = LINE ( 'NONE', #26593, #43789 ) ;
#15730 = DIRECTION ( 'NONE',  ( 0.9466432954593471116, 0.3222832157619555660, 8.771047036255756069E-09 ) ) ;
#15731 = VECTOR ( 'NONE', #22931, 1000.000000000000000 ) ;
#15732 = CARTESIAN_POINT ( 'NONE',  ( -15.39389095703113952, -21.97733419268598709, 72.23070866474378704 ) ) ;
#15733 = CARTESIAN_POINT ( 'NONE',  ( -10.16748990304072464, -13.12235252378331651, 71.39323974795351546 ) ) ;
#15734 = AXIS2_PLACEMENT_3D ( 'NONE', #42615, #27813, #46298 ) ;
#15735 = EDGE_CURVE ( 'NONE', #3842, #4984, #8451, .T. ) ;
#15736 = ORIENTED_EDGE ( 'NONE', *, *, #45298, .F. ) ;
#15737 = AXIS2_PLACEMENT_3D ( 'NONE', #33572, #33834, #130 ) ;
#15738 = ADVANCED_FACE ( 'NONE', ( #12381 ), #46122, .T. ) ;
#15739 = CARTESIAN_POINT ( 'NONE',  ( -23.55638888376047646, -11.43265673080018097, 69.90827408357159811 ) ) ;
#15740 = CARTESIAN_POINT ( 'NONE',  ( -23.08261055559088248, -18.93003034027461950, 62.65406880913197796 ) ) ;
#15741 = EDGE_CURVE ( 'NONE', #11741, #41372, #9186, .T. ) ;
#15742 = ADVANCED_FACE ( 'NONE', ( #28387, #9677 ), #17275, .T. ) ;
#15743 = ORIENTED_EDGE ( 'NONE', *, *, #46058, .T. ) ;
#15744 = VECTOR ( 'NONE', #131, 1000.000000000000227 ) ;
#15745 = FACE_OUTER_BOUND ( 'NONE', #7872, .T. ) ;
#15746 =( BOUNDED_CURVE ( )  B_SPLINE_CURVE ( 3, ( #40025, #32850, #39534, #46923 ),
 .UNSPECIFIED., .F., .F. ) 
 B_SPLINE_CURVE_WITH_KNOTS ( ( 4, 4 ),
 ( 0.000000000000000000, 0.4074455897393662873 ),
 .UNSPECIFIED. ) 
 CURVE ( )  GEOMETRIC_REPRESENTATION_ITEM ( )  RATIONAL_B_SPLINE_CURVE ( ( 1.000000000000000000, 0.4567392136813360759, 0.3561768502900318212, 0.6983129098260872913 ) ) 
 REPRESENTATION_ITEM ( '' )  );
#15747 = VERTEX_POINT ( 'NONE', #35515 ) ;
#15748 = CARTESIAN_POINT ( 'NONE',  ( -11.53247046633659245, -18.68106308600668441, 64.74707076449911369 ) ) ;
#15749 = ORIENTED_EDGE ( 'NONE', *, *, #19653, .T. ) ;
#15750 = CARTESIAN_POINT ( 'NONE',  ( -50.42409385541305511, -15.80920654474410725, 74.99999999999998579 ) ) ;
#15751 = CARTESIAN_POINT ( 'NONE',  ( -11.42587710518540334, -11.10406226247761019, 57.49431069621225276 ) ) ;
#15752 = ORIENTED_EDGE ( 'NONE', *, *, #17013, .F. ) ;
#15753 = DIRECTION ( 'NONE',  ( 7.484513349675954647E-07, -7.898531916559714080E-07, -0.9999999999994080291 ) ) ;
#15754 = CARTESIAN_POINT ( 'NONE',  ( -12.79725838692604434, -20.12850099319811292, 71.80653676770127447 ) ) ;
#15755 = CARTESIAN_POINT ( 'NONE',  ( -18.39284385650552167, -7.406986770994972602, 48.81910596585309747 ) ) ;
#15756 = CARTESIAN_POINT ( 'NONE',  ( -24.47110706704248528, -14.59897147552597474, 63.00736729327273622 ) ) ;
#15757 = LINE ( 'NONE', #23413, #31596 ) ;
#15758 = DIRECTION ( 'NONE',  ( 0.9687793358424817702, -0.2479245821708686570, 0.000000000000000000 ) ) ;
#15759 = EDGE_LOOP ( 'NONE', ( #654, #12577, #30085, #20652, #44126 ) ) ;
#15761 = CARTESIAN_POINT ( 'NONE',  ( -10.44202778021669609, -14.30845378979165794, 64.68803863533310050 ) ) ;
#15760 =( BOUNDED_CURVE ( )  B_SPLINE_CURVE ( 3, ( #19425, #14981, #45071, #41851 ),
 .UNSPECIFIED., .F., .F. ) 
 B_SPLINE_CURVE_WITH_KNOTS ( ( 4, 4 ),
 ( 0.000000000000000000, 0.4074455897393688408 ),
 .UNSPECIFIED. ) 
 CURVE ( )  GEOMETRIC_REPRESENTATION_ITEM ( )  RATIONAL_B_SPLINE_CURVE ( ( 1.000000000000000000, 0.4567392136813259174, 0.3561768502900280464, 0.6983129098261063872 ) ) 
 REPRESENTATION_ITEM ( '' )  );
#15762 = CARTESIAN_POINT ( 'NONE',  ( -16.39284385541304800, -8.630756214087126565, 51.74842643355248129 ) ) ;
#15763 = DIRECTION ( 'NONE',  ( 0.8083598999316399247, 0.5886886037477750966, 6.671815825018553389E-08 ) ) ;
#15764 = CARTESIAN_POINT ( 'NONE',  ( -15.80316865820435446, -9.815700611529287301, 49.52966884056655772 ) ) ;
#15765 = CARTESIAN_POINT ( 'NONE',  ( -12.90354087724769272, -8.887350501024684490, 67.49447389996370816 ) ) ;
#15766 = EDGE_CURVE ( 'NONE', #35214, #22721, #8566, .T. ) ;
#15767 = ORIENTED_EDGE ( 'NONE', *, *, #7866, .T. ) ;
#15768 = ORIENTED_EDGE ( 'NONE', *, *, #7729, .F. ) ;
#15769 = CIRCLE ( 'NONE', #4794, 2.000000000000001776 ) ;
#15770 = CARTESIAN_POINT ( 'NONE',  ( -21.94242186726961208, -9.397052521110282441, 60.00699132926281010 ) ) ;
#15771 = CARTESIAN_POINT ( 'NONE',  ( -24.33947722655236845, -16.19878214197559529, 66.15505208431230244 ) ) ;
#15772 = VERTEX_POINT ( 'NONE', #47345 ) ;
#15773 = CARTESIAN_POINT ( 'NONE',  ( -10.43298842381219238, -15.77843866184169208, 57.72359922229868801 ) ) ;
#15774 = CARTESIAN_POINT ( 'NONE',  ( -15.12888584993918428, -21.89692032561032775, 68.83238837976321634 ) ) ;
#15775 = CARTESIAN_POINT ( 'NONE',  ( -20.92409385759799179, -9.359200813967568422, 50.49621490985803263 ) ) ;
#15776 = CARTESIAN_POINT ( 'NONE',  ( -18.92409385541305511, -14.80920654474410547, 48.99999999999997868 ) ) ;
#15777 = CARTESIAN_POINT ( 'NONE',  ( -12.05128958966154329, -19.97034025487388931, 61.57491367064827159 ) ) ;
#15778 = CARTESIAN_POINT ( 'NONE',  ( -19.50843993236927432, -21.96177808838975665, 62.11008241541560437 ) ) ;
#15779 = VECTOR ( 'NONE', #33404, 1000.000000000000114 ) ;
#15780 = CARTESIAN_POINT ( 'NONE',  ( -14.03172754404545053, -8.686077560366827655, 74.48489347840799724 ) ) ;
#15781 =( BOUNDED_SURFACE ( )  B_SPLINE_SURFACE ( 3, 1, ( 
 ( #37529, #18840 ),
 ( #25736, #18575 ),
 ( #48631, #45205 ),
 ( #38763, #35062 ),
 ( #4800, #16343 ),
 ( #15863, #45693 ),
 ( #5044, #16095 ) ),
 .UNSPECIFIED., .T., .F., .F. ) 
 B_SPLINE_SURFACE_WITH_KNOTS ( ( 4, 3, 4 ),
 ( 2, 2 ),
 ( 0.000000000000000000, 0.5000000000000000000, 1.000000000000000000 ),
 ( 0.000000000000000000, 1.000000000000000000 ),
 .UNSPECIFIED. ) 
 GEOMETRIC_REPRESENTATION_ITEM ( )  RATIONAL_B_SPLINE_SURFACE ( (
 ( 1.000000000000000000, 1.000000000000000000),
 ( 0.3333333333333335369, 0.3333333333333330373),
 ( 0.3333333333333335369, 0.3333333333333330373),
 ( 1.000000000000000000, 1.000000000000000000),
 ( 0.3333333333333333703, 0.3333333333333333703),
 ( 0.3333333333333333703, 0.3333333333333333703),
 ( 1.000000000000000000, 1.000000000000000000) ) ) 
 REPRESENTATION_ITEM ( '' )  SURFACE ( )  );
#15782 = VERTEX_POINT ( 'NONE', #39697 ) ;
#15783 = DIRECTION ( 'NONE',  ( -1.616182858256117057E-16, -0.003028072113818697231, 0.9999954153791273948 ) ) ;
#15784 = CARTESIAN_POINT ( 'NONE',  ( -50.42609385541305755, -14.80920654474427600, 73.09411764705880898 ) ) ;
#15785 = CARTESIAN_POINT ( 'NONE',  ( -24.00901317767523935, -17.32824147414624960, 69.42811846502259243 ) ) ;
#15786 = CARTESIAN_POINT ( 'NONE',  ( -6.424093855413055110, -6.859206544744110623, 47.99999999999998579 ) ) ;
#15787 = LINE ( 'NONE', #20217, #11187 ) ;
#15788 = CARTESIAN_POINT ( 'NONE',  ( -14.89095676091066345, -21.33490639913799924, 61.93600435359637402 ) ) ;
#15789 = ORIENTED_EDGE ( 'NONE', *, *, #44457, .F. ) ;
#15790 = VERTEX_POINT ( 'NONE', #13573 ) ;
#15791 = CARTESIAN_POINT ( 'NONE',  ( -19.67573413203048460, -21.49838315979392789, 72.54911470401957274 ) ) ;
#15792 = ORIENTED_EDGE ( 'NONE', *, *, #35991, .T. ) ;
#15793 = CARTESIAN_POINT ( 'NONE',  ( -19.14088062437382831, -4.707495580760234333, 53.49999999999995026 ) ) ;
#15794 = AXIS2_PLACEMENT_3D ( 'NONE', #41316, #2500, #45277 ) ;
#15795 = CARTESIAN_POINT ( 'NONE',  ( -10.45740709548926262, -13.70915569549963031, 57.86313879094461754 ) ) ;
#15796 = ORIENTED_EDGE ( 'NONE', *, *, #10452, .T. ) ;
#15797 = CARTESIAN_POINT ( 'NONE',  ( -10.82471902208573766, -11.35211385731556710, 67.81202917830380272 ) ) ;
#15798 = AXIS2_PLACEMENT_3D ( 'NONE', #16148, #34384, #8546 ) ;
#15799 = LINE ( 'NONE', #11391, #26100 ) ;
#15800 = EDGE_CURVE ( 'NONE', #37303, #4227, #25260, .T. ) ;
#15801 = EDGE_CURVE ( 'NONE', #10524, #16810, #32072, .T. ) ;
#15802 = DIRECTION ( 'NONE',  ( -3.071710424422018668E-17, 6.404604876783312462E-16, 1.000000000000000000 ) ) ;
#15803 = ORIENTED_EDGE ( 'NONE', *, *, #24140, .T. ) ;
#15804 = AXIS2_PLACEMENT_3D ( 'NONE', #16179, #38608, #15945 ) ;
#15805 = CARTESIAN_POINT ( 'NONE',  ( -20.94465790601859467, -8.243431112063134947, 59.95629843672877257 ) ) ;
#15806 = CARTESIAN_POINT ( 'NONE',  ( -46.29409385541305255, -12.91120565595569758, 69.30071302485083606 ) ) ;
#15807 = ORIENTED_EDGE ( 'NONE', *, *, #27015, .F. ) ;
#15808 = DIRECTION ( 'NONE',  ( 0.000000000000000000, 1.000000000000000000, -0.000000000000000000 ) ) ;
#15809 = AXIS2_PLACEMENT_3D ( 'NONE', #9657, #35492, #31808 ) ;
#15810 = CARTESIAN_POINT ( 'NONE',  ( -12.24819225201853001, -20.16768402423936024, 64.97336598306215194 ) ) ;
#15811 = EDGE_LOOP ( 'NONE', ( #44615, #29176, #13184, #3144 ) ) ;
#15812 = ADVANCED_FACE ( 'NONE', ( #27886 ), #31870, .T. ) ;
#15813 = ADVANCED_FACE ( 'NONE', ( #32547 ), #28132, .T. ) ;
#15814 = CARTESIAN_POINT ( 'NONE',  ( -23.46647660864419294, -19.16733412182131246, 62.39760931945144051 ) ) ;
#15815 = CARTESIAN_POINT ( 'NONE',  ( -16.57921203443829583, -21.81142124131518756, 69.11049422539112186 ) ) ;
#15816 = DIRECTION ( 'NONE',  ( 2.231660450020913271E-16, 0.9999954153791273948, 0.003028072113822188795 ) ) ;
#15817 = ORIENTED_EDGE ( 'NONE', *, *, #42149, .T. ) ;
#15818 = CARTESIAN_POINT ( 'NONE',  ( -23.22746095445554815, -10.13763477365454868, 63.17162361582423813 ) ) ;
#15819 = CARTESIAN_POINT ( 'NONE',  ( -17.72419709140651278, -21.80277058947482516, 58.70553378253836030 ) ) ;
#15820 = CIRCLE ( 'NONE', #140, 1.999999999999999556 ) ;
#15821 = FACE_OUTER_BOUND ( 'NONE', #5035, .T. ) ;
#15822 = CARTESIAN_POINT ( 'NONE',  ( -21.50966673221228120, -17.12947588552333045, 52.02966884056656482 ) ) ;
#15823 = CARTESIAN_POINT ( 'NONE',  ( -8.424093855413060439, -6.359206544744109735, 47.99999999999998579 ) ) ;
#15824 = CARTESIAN_POINT ( 'NONE',  ( -20.21425406316526363, -8.334789581166827332, 70.25100338998272775 ) ) ;
#15825 = LINE ( 'NONE', #34293, #1404 ) ;
#15826 = DIRECTION ( 'NONE',  ( -0.6973657521612035559, 0.7167154300785205656, -1.015100525525034718E-08 ) ) ;
#15827 = CARTESIAN_POINT ( 'NONE',  ( -10.95381465013825206, -17.48043978162002077, 68.39721944380028162 ) ) ;
#15828 = CARTESIAN_POINT ( 'NONE',  ( -19.20534385650551457, -8.801233750844183135, 48.81488406609782515 ) ) ;
#15829 = EDGE_CURVE ( 'NONE', #4057, #47942, #5086, .T. ) ;
#15830 = CIRCLE ( 'NONE', #12676, 1.249999999999999556 ) ;
#15831 = ORIENTED_EDGE ( 'NONE', *, *, #44575, .F. ) ;
#15832 = CARTESIAN_POINT ( 'NONE',  ( -16.58751243259469277, -21.80939447449397051, 65.37564390318223673 ) ) ;
#15833 = CARTESIAN_POINT ( 'NONE',  ( -10.47425561207849753, -17.49314520081206936, 64.81234810402725088 ) ) ;
#15834 = ORIENTED_EDGE ( 'NONE', *, *, #27608, .T. ) ;
#15835 = B_SPLINE_CURVE_WITH_KNOTS ( 'NONE', 3,
 ( #32026, #34748, #27115, #16018, #8409, #28082, #31062, #5205, #24160, #39165 ),
 .UNSPECIFIED., .F., .F.,
 ( 4, 2, 2, 2, 4 ),
 ( 0.000000000000000000, 0.2500000000000000000, 0.5000000000000000000, 0.7500000000000000000, 1.000000000000000000 ),
 .UNSPECIFIED. ) ;
#15836 = CARTESIAN_POINT ( 'NONE',  ( -35.42409385541304800, -7.059211358595575803, 50.50317947571981847 ) ) ;
#15837 = CARTESIAN_POINT ( 'NONE',  ( -23.88415222675040184, -17.63235122089636775, 62.47360984996718258 ) ) ;
#15838 = CARTESIAN_POINT ( 'NONE',  ( -12.78427029111582236, -20.05066579198349075, 68.56330852931057507 ) ) ;
#15839 = CARTESIAN_POINT ( 'NONE',  ( -36.42409385541304800, -9.359200813967566646, 50.49621490985803263 ) ) ;
#15840 = ORIENTED_EDGE ( 'NONE', *, *, #44706, .F. ) ;
#15841 = CARTESIAN_POINT ( 'NONE',  ( -18.25923033419348940, -22.21300364388852344, 69.00170051292239748 ) ) ;
#15842 = CARTESIAN_POINT ( 'NONE',  ( -10.41921500249975807, -15.63170790598816140, 64.92260423241262401 ) ) ;
#15843 = VECTOR ( 'NONE', #14730, 1000.000000000000000 ) ;
#15844 = CARTESIAN_POINT ( 'NONE',  ( -14.56205194875994735, -21.68753530842563748, 58.26643629975792038 ) ) ;
#15845 = ORIENTED_EDGE ( 'NONE', *, *, #9691, .F. ) ;
#15846 = DIRECTION ( 'NONE',  ( 0.9687793358424821033, -0.2479245821708680464, 0.000000000000000000 ) ) ;
#15847 = CIRCLE ( 'NONE', #17430, 1.249999999999999556 ) ;
#15848 = CARTESIAN_POINT ( 'NONE',  ( -23.80338573481879294, -11.80731802715296119, 59.76763678108634537 ) ) ;
#15849 = DIRECTION ( 'NONE',  ( 0.4182840851231336421, -0.9083162577718748576, 8.112345261759808545E-09 ) ) ;
#15850 = DIRECTION ( 'NONE',  ( -3.071710424422018668E-17, 6.404604876783312462E-16, 1.000000000000000000 ) ) ;
#15851 = CARTESIAN_POINT ( 'NONE',  ( -23.10700766261894046, -18.89652940832406358, 62.65406835416833786 ) ) ;
#15852 = ORIENTED_EDGE ( 'NONE', *, *, #48186, .F. ) ;
#15853 = ORIENTED_EDGE ( 'NONE', *, *, #19543, .F. ) ;
#15854 = CARTESIAN_POINT ( 'NONE',  ( -21.62409385541304374, -9.359200813967568422, 50.49621490985803263 ) ) ;
#15855 = CARTESIAN_POINT ( 'NONE',  ( -21.24554616535955631, -21.20453920045676810, 65.76949338751086316 ) ) ;
#15856 = CARTESIAN_POINT ( 'NONE',  ( -23.37964394754908781, -11.13058451656118386, 73.37695695401920659 ) ) ;
#15857 = AXIS2_PLACEMENT_3D ( 'NONE', #41741, #23038, #23766 ) ;
#15858 = CARTESIAN_POINT ( 'NONE',  ( -20.31413516131974717, -8.378470924821744603, 67.06632013881642251 ) ) ;
#15859 = AXIS2_PLACEMENT_3D ( 'NONE', #43477, #24990, #5133 ) ;
#15860 = CARTESIAN_POINT ( 'NONE',  ( -24.72409385541305582, -15.80920654474410725, 65.99999999999998579 ) ) ;
#15861 = EDGE_CURVE ( 'NONE', #39071, #29156, #47092, .T. ) ;
#15862 = CARTESIAN_POINT ( 'NONE',  ( -20.47364684392118050, -8.506973744139683546, 66.85274300213296783 ) ) ;
#15863 = CARTESIAN_POINT ( 'NONE',  ( -14.25645962476006368, -8.507545769726087670, 74.61443249008125633 ) ) ;
#15864 = CARTESIAN_POINT ( 'NONE',  ( -11.50273595086851763, -11.07590776185467263, 57.20903212540526539 ) ) ;
#15865 = ORIENTED_EDGE ( 'NONE', *, *, #8442, .T. ) ;
#15866 = CARTESIAN_POINT ( 'NONE',  ( -21.19335628676919470, -20.70964401715573189, 72.63519632848037588 ) ) ;
#15867 = DIRECTION ( 'NONE',  ( 3.071710424422018668E-17, -6.404604876783312462E-16, -1.000000000000000000 ) ) ;
#15868 = ORIENTED_EDGE ( 'NONE', *, *, #32968, .F. ) ;
#15869 = EDGE_CURVE ( 'NONE', #13117, #15068, #30087, .T. ) ;
#15870 = ADVANCED_FACE ( 'NONE', ( #44147 ), #33007, .T. ) ;
#15871 = FACE_OUTER_BOUND ( 'NONE', #44811, .T. ) ;
#15872 = FACE_OUTER_BOUND ( 'NONE', #27751, .T. ) ;
#15873 = ORIENTED_EDGE ( 'NONE', *, *, #45753, .F. ) ;
#15874 = CARTESIAN_POINT ( 'NONE',  ( -9.534148923395315833, -8.271570107951246698, 53.49999999999995026 ) ) ;
#15875 = EDGE_CURVE ( 'NONE', #47624, #38508, #11640, .T. ) ;
#15876 = VECTOR ( 'NONE', #29059, 1000.000000000000000 ) ;
#15877 = VERTEX_POINT ( 'NONE', #40651 ) ;
#15878 = CARTESIAN_POINT ( 'NONE',  ( -10.83008762082782006, -12.29245259246931354, 60.94286399630310314 ) ) ;
#15879 = EDGE_CURVE ( 'NONE', #37877, #2353, #11118, .T. ) ;
#15880 = LINE ( 'NONE', #4330, #17184 ) ;
#15881 = CARTESIAN_POINT ( 'NONE',  ( -20.93791933404421002, -8.239859431045912785, 59.94851102954661570 ) ) ;
#15882 = VERTEX_POINT ( 'NONE', #29093 ) ;
#15883 = CARTESIAN_POINT ( 'NONE',  ( -45.92409385541306932, -16.70920654474410938, 70.13000000000000966 ) ) ;
#15884 = CARTESIAN_POINT ( 'NONE',  ( -24.05845721068777010, -12.57644527891515551, 73.54225570276561541 ) ) ;
#15885 = CARTESIAN_POINT ( 'NONE',  ( -10.41531639268335496, -14.04517892474411589, 60.93293405735092705 ) ) ;
#15886 = DIRECTION ( 'NONE',  ( -5.731567514496413899E-31, -1.020425574103664789E-16, -1.000000000000000000 ) ) ;
#15887 = CARTESIAN_POINT ( 'NONE',  ( -24.35389707626741185, -16.10709931453380861, 62.87856533165624029 ) ) ;
#15888 = CARTESIAN_POINT ( 'NONE',  ( -14.19909385541286362, -8.105421454601380304, 49.25000573077609545 ) ) ;
#15889 = EDGE_CURVE ( 'NONE', #19236, #46816, #13245, .T. ) ;
#15890 = DIRECTION ( 'NONE',  ( 0.9048399035850771543, 0.4257519804770706906, 1.330923649722295736E-08 ) ) ;
#15891 = VERTEX_POINT ( 'NONE', #10397 ) ;
#15892 = PLANE ( 'NONE',  #31535 ) ;
#15893 = ORIENTED_EDGE ( 'NONE', *, *, #45664, .T. ) ;
#15894 = CARTESIAN_POINT ( 'NONE',  ( -11.19247825287758857, -11.62036905852712110, 67.91864580735541779 ) ) ;
#15895 = CARTESIAN_POINT ( 'NONE',  ( -11.05034076241727625, -11.79557573020262318, 71.37388789199357575 ) ) ;
#15896 = EDGE_LOOP ( 'NONE', ( #9647, #25368 ) ) ;
#15897 = DIRECTION ( 'NONE',  ( 0.9848822020395751053, -0.1732254256905498280, -7.367703375118635757E-08 ) ) ;
#15898 = FACE_BOUND ( 'NONE', #9767, .T. ) ;
#15899 = VERTEX_POINT ( 'NONE', #3470 ) ;
#15900 = EDGE_LOOP ( 'NONE', ( #3240, #19577, #8313, #44205, #21133 ) ) ;
#15901 = ORIENTED_EDGE ( 'NONE', *, *, #28820, .F. ) ;
#15902 = CARTESIAN_POINT ( 'NONE',  ( -10.43098718212803000, -15.70539730037032911, 61.32316937334011442 ) ) ;
#15903 = DIRECTION ( 'NONE',  ( 1.000000000000000000, 2.866981220435666553E-17, 0.000000000000000000 ) ) ;
#15904 = CARTESIAN_POINT ( 'NONE',  ( -16.65185932245351808, -21.81708442718849383, 65.51092266128213737 ) ) ;
#15905 =( BOUNDED_SURFACE ( )  B_SPLINE_SURFACE ( 3, 1, ( 
 ( #41204, #48108 ),
 ( #37743, #3784 ),
 ( #18794, #33801 ),
 ( #21764, #15085 ),
 ( #36750, #41440 ),
 ( #7738, #48341 ),
 ( #22752, #3039 ) ),
 .UNSPECIFIED., .T., .F., .F. ) 
 B_SPLINE_SURFACE_WITH_KNOTS ( ( 4, 3, 4 ),
 ( 2, 2 ),
 ( 0.000000000000000000, 0.5000000000000000000, 1.000000000000000000 ),
 ( 0.000000000000000000, 1.000000000000000000 ),
 .UNSPECIFIED. ) 
 GEOMETRIC_REPRESENTATION_ITEM ( )  RATIONAL_B_SPLINE_SURFACE ( (
 ( 1.000000000000000000, 1.000000000000000000),
 ( 0.3333333333333335369, 0.3333333333333330373),
 ( 0.3333333333333335369, 0.3333333333333330373),
 ( 1.000000000000000000, 1.000000000000000000),
 ( 0.3333333333333333703, 0.3333333333333333703),
 ( 0.3333333333333333703, 0.3333333333333333703),
 ( 1.000000000000000000, 1.000000000000000000) ) ) 
 REPRESENTATION_ITEM ( '' )  SURFACE ( )  );
#15906 = CARTESIAN_POINT ( 'NONE',  ( -21.27305602007818663, -8.962297277456373834, 73.88663334704315844 ) ) ;
#15907 = CARTESIAN_POINT ( 'NONE',  ( -11.83648969670631068, -9.881597305254256725, 64.12890704636625117 ) ) ;
#15908 = DIRECTION ( 'NONE',  ( -0.9918916210775228226, -0.1270866320121812332, 6.503929234589264523E-08 ) ) ;
#15909 = VERTEX_POINT ( 'NONE', #41150 ) ;
#15910 = ORIENTED_EDGE ( 'NONE', *, *, #26350, .T. ) ;
#15911 = DIRECTION ( 'NONE',  ( -3.071710424422018668E-17, 6.404604876783312462E-16, 1.000000000000000000 ) ) ;
#15912 = CARTESIAN_POINT ( 'NONE',  ( -13.73367451952834095, -20.81619193053765926, 65.28628851148928902 ) ) ;
#15913 = DIRECTION ( 'NONE',  ( 8.329294198805576557E-07, -2.487164606213012505E-06, 0.9999999999965599740 ) ) ;
#15914 = DIRECTION ( 'NONE',  ( 0.3478314405900309603, 0.9375570856950864451, -9.567072274253696421E-17 ) ) ;
#15915 = ORIENTED_EDGE ( 'NONE', *, *, #1713, .F. ) ;
#15916 = ADVANCED_FACE ( 'NONE', ( #3234 ), #33245, .T. ) ;
#15917 = CARTESIAN_POINT ( 'NONE',  ( -14.14284385650552167, -8.811426318492348031, 52.18089403414752070 ) ) ;
#15918 =( BOUNDED_CURVE ( )  B_SPLINE_CURVE ( 3, ( #22649, #2942, #4, #29303 ),
 .UNSPECIFIED., .F., .F. ) 
 B_SPLINE_CURVE_WITH_KNOTS ( ( 4, 4 ),
 ( 1.570796326794896558, 1.780235837034217727 ),
 .UNSPECIFIED. ) 
 CURVE ( )  GEOMETRIC_REPRESENTATION_ITEM ( )  RATIONAL_B_SPLINE_CURVE ( ( 1.000000000000000000, 0.9963479302455154896, 0.9963479302455154896, 1.000000000000000000 ) ) 
 REPRESENTATION_ITEM ( '' )  );
#15919 = VERTEX_POINT ( 'NONE', #26372 ) ;
#15920 = DIRECTION ( 'NONE',  ( -3.071710424422018668E-17, 6.404604876783312462E-16, 1.000000000000000000 ) ) ;
#15921 = ADVANCED_FACE ( 'NONE', ( #47807 ), #1368, .T. ) ;
#15922 = CARTESIAN_POINT ( 'NONE',  ( -10.51729497052147977, -16.22293520194095606, 71.74750383215044280 ) ) ;
#15923 = CARTESIAN_POINT ( 'NONE',  ( -10.04821600842096174, -15.85811274820897410, 64.62276192103250594 ) ) ;
#15924 = ORIENTED_EDGE ( 'NONE', *, *, #15185, .F. ) ;
#15925 = DIRECTION ( 'NONE',  ( 0.000000000000000000, 0.000000000000000000, -1.000000000000000000 ) ) ;
#15926 = CARTESIAN_POINT ( 'NONE',  ( -11.60526899143904345, -18.79015832504765271, 68.23161775275829655 ) ) ;
#15927 = CARTESIAN_POINT ( 'NONE',  ( -12.15286730501820678, -9.544433317881530598, 57.34581436681493471 ) ) ;
#15928 = EDGE_CURVE ( 'NONE', #48327, #38900, #28207, .T. ) ;
#15929 = VERTEX_POINT ( 'NONE', #3724 ) ;
#15930 = CARTESIAN_POINT ( 'NONE',  ( -12.24833890097646005, -19.59612930767528738, 58.22682369889817267 ) ) ;
#15931 = ADVANCED_FACE ( 'NONE', ( #21706 ), #14765, .T. ) ;
#15932 = CARTESIAN_POINT ( 'NONE',  ( -17.36175868705992897, -7.359389033274929659, 67.06393689457253515 ) ) ;
#15933 = CARTESIAN_POINT ( 'NONE',  ( -11.46875891826176819, -18.48806303968299858, 61.27710833525312495 ) ) ;
#15934 = ORIENTED_EDGE ( 'NONE', *, *, #42800, .T. ) ;
#15935 = CARTESIAN_POINT ( 'NONE',  ( -10.38847021856859421, -14.31440148336201545, 60.80332504197532728 ) ) ;
#15936 = ORIENTED_EDGE ( 'NONE', *, *, #23779, .T. ) ;
#15937 = CARTESIAN_POINT ( 'NONE',  ( -9.975463547418753407, -14.66361225716259575, 71.43508524632446210 ) ) ;
#15938 = DIRECTION ( 'NONE',  ( 0.9687793358424819923, -0.2479245821708680464, 0.000000000000000000 ) ) ;
#15939 = EDGE_CURVE ( 'NONE', #6635, #28650, #7431, .T. ) ;
#15940 = EDGE_LOOP ( 'NONE', ( #25746, #25959, #10701, #8973, #15390 ) ) ;
#15941 = CARTESIAN_POINT ( 'NONE',  ( -16.22845603143158755, -22.16339683637704638, 61.94223519165076652 ) ) ;
#15942 = CARTESIAN_POINT ( 'NONE',  ( -17.98657259272421172, -21.83703102787368167, 62.16063850355641307 ) ) ;
#15943 = CARTESIAN_POINT ( 'NONE',  ( -14.21750986585362320, -8.084461106059640301, 67.43691998704751711 ) ) ;
#15944 = VERTEX_POINT ( 'NONE', #45110 ) ;
#15945 = DIRECTION ( 'NONE',  ( -1.077913161506870186E-05, 7.121115479698836302E-06, 0.9999999999165498643 ) ) ;
#15946 = EDGE_CURVE ( 'NONE', #44664, #35872, #22691, .T. ) ;
#15947 = CARTESIAN_POINT ( 'NONE',  ( -21.34628024798174550, -12.22231469401973847, 52.02966884056656482 ) ) ;
#15948 = DIRECTION ( 'NONE',  ( 0.000000000000000000, 0.000000000000000000, 1.000000000000000000 ) ) ;
#15949 = CYLINDRICAL_SURFACE ( 'NONE', #2291, 0.1499999999999948874 ) ;
#15950 = ORIENTED_EDGE ( 'NONE', *, *, #26544, .F. ) ;
#15951 = DIRECTION ( 'NONE',  ( -0.9180681052388980357, 0.3964226963016366789, 0.000000000000000000 ) ) ;
#15952 = CARTESIAN_POINT ( 'NONE',  ( -21.84598475011588903, -8.812495317756813051, 70.31787921227815730 ) ) ;
#15953 = VERTEX_POINT ( 'NONE', #2983 ) ;
#15954 = VERTEX_POINT ( 'NONE', #17992 ) ;
#15955 = LINE ( 'NONE', #19914, #20448 ) ;
#15956 = DIRECTION ( 'NONE',  ( -3.071710424422018668E-17, 6.404604876783312462E-16, 1.000000000000000000 ) ) ;
#15957 = CARTESIAN_POINT ( 'NONE',  ( -21.44055400477819973, -12.39439182751215718, 49.52966884056655772 ) ) ;
#15958 = CARTESIAN_POINT ( 'NONE',  ( -13.21784385759799108, -6.860780111191488118, 51.02154966934377711 ) ) ;
#15959 = CARTESIAN_POINT ( 'NONE',  ( -24.82767328945774210, -13.97813652794827988, 73.16625576376715401 ) ) ;
#15960 = CARTESIAN_POINT ( 'NONE',  ( -12.69763806180496601, -20.04058448603118592, 68.62185382311069759 ) ) ;
#15961 = CARTESIAN_POINT ( 'NONE',  ( -10.72530867274958410, -17.00760959713300835, 57.97288447305809456 ) ) ;
#15962 = CARTESIAN_POINT ( 'NONE',  ( -10.56317305444034105, -16.44707251114675728, 71.44750086157920066 ) ) ;
#15963 = ORIENTED_EDGE ( 'NONE', *, *, #21918, .F. ) ;
#15964 = ORIENTED_EDGE ( 'NONE', *, *, #39882, .T. ) ;
#15965 = CARTESIAN_POINT ( 'NONE',  ( -11.32522400900782067, -11.27219014254736074, 60.96413645226084554 ) ) ;
#15966 = AXIS2_PLACEMENT_3D ( 'NONE', #1594, #28435, #39510 ) ;
#15967 = CARTESIAN_POINT ( 'NONE',  ( -14.60783614669699304, -21.70648650955843806, 58.35113213314874514 ) ) ;
#15968 = CARTESIAN_POINT ( 'NONE',  ( -10.93232766038821424, -17.55941949638709687, 68.38249893951126523 ) ) ;
#15969 = CARTESIAN_POINT ( 'NONE',  ( -18.66311988809301425, -7.868636481342422329, 70.65595886192740238 ) ) ;
#15970 = ADVANCED_FACE ( 'NONE', ( #21949 ), #41939, .T. ) ;
#15971 = VERTEX_POINT ( 'NONE', #12979 ) ;
#15972 = B_SPLINE_CURVE_WITH_KNOTS ( 'NONE', 1,
 ( #41269, #30213 ),
 .UNSPECIFIED., .F., .F.,
 ( 2, 2 ),
 ( 0.000000000000000000, 1.000000000000000000 ),
 .UNSPECIFIED. ) ;
#15973 = VERTEX_POINT ( 'NONE', #16913 ) ;
#15974 = CYLINDRICAL_SURFACE ( 'NONE', #22539, 0.1500000000000065448 ) ;
#15975 = CARTESIAN_POINT ( 'NONE',  ( -24.86969121598721344, -14.53217971827670496, 66.36947994509128534 ) ) ;
#15976 = DIRECTION ( 'NONE',  ( 1.000000000000000000, -1.224646799147353207E-16, 6.695352868347749370E-17 ) ) ;
#15977 = CARTESIAN_POINT ( 'NONE',  ( -24.03161744405940325, -17.27608056677072312, 73.29824685711943744 ) ) ;
#15978 = EDGE_LOOP ( 'NONE', ( #9361, #10794, #42316, #10950 ) ) ;
#15979 = CARTESIAN_POINT ( 'NONE',  ( -13.10126076353387603, -9.301845420481674509, 70.92095663008969098 ) ) ;
#15980 = CARTESIAN_POINT ( 'NONE',  ( -24.80769047312930553, -15.80232199467591947, 69.71802767292497549 ) ) ;
#15981 = EDGE_LOOP ( 'NONE', ( #38939, #16903 ) ) ;
#15982 = EDGE_CURVE ( 'NONE', #39713, #21906, #5373, .T. ) ;
#15983 = CARTESIAN_POINT ( 'NONE',  ( -20.00946575929301474, -8.250368826910309039, 74.02096600124984604 ) ) ;
#15984 = FACE_OUTER_BOUND ( 'NONE', #35198, .T. ) ;
#15985 = ORIENTED_EDGE ( 'NONE', *, *, #42754, .T. ) ;
#15986 = B_SPLINE_CURVE_WITH_KNOTS ( 'NONE', 3,
 ( #16712, #46292, #23891, #42109, #34458, #9109, #746, #8373, #23397, #38393 ),
 .UNSPECIFIED., .F., .F.,
 ( 4, 2, 2, 2, 4 ),
 ( 0.000000000000000000, 0.2500000000000000000, 0.5000000000000000000, 0.7500000000000000000, 1.000000000000000000 ),
 .UNSPECIFIED. ) ;
#15987 = CARTESIAN_POINT ( 'NONE',  ( -23.66133310609451712, -18.88359296917171903, 69.40876596050124192 ) ) ;
#15988 = ORIENTED_EDGE ( 'NONE', *, *, #16553, .T. ) ;
#15989 = FACE_OUTER_BOUND ( 'NONE', #39228, .T. ) ;
#15990 = EDGE_CURVE ( 'NONE', #10407, #36695, #10105, .T. ) ;
#15991 = CARTESIAN_POINT ( 'NONE',  ( -19.26584314952366128, -21.56270023830151317, 58.82507339201525554 ) ) ;
#15992 = VERTEX_POINT ( 'NONE', #20390 ) ;
#15993 = CARTESIAN_POINT ( 'NONE',  ( -21.42170527289675164, -17.27794275993632667, 49.52966884056655772 ) ) ;
#15994 = CARTESIAN_POINT ( 'NONE',  ( -10.28660183209414569, -12.67406856256811309, 64.46847312737159541 ) ) ;
#15995 = AXIS2_PLACEMENT_3D ( 'NONE', #5004, #5487, #5958 ) ;
#15996 = CARTESIAN_POINT ( 'NONE',  ( -18.22409385650551528, -6.426201560718813433, 50.50509628382439331 ) ) ;
#15997 = FACE_OUTER_BOUND ( 'NONE', #9340, .T. ) ;
#15998 = EDGE_CURVE ( 'NONE', #16885, #22869, #949, .T. ) ;
#15999 = CARTESIAN_POINT ( 'NONE',  ( -19.17403394478084522, -7.567564808342563509, 63.47443287871421091 ) ) ;
#16000 = CARTESIAN_POINT ( 'NONE',  ( -13.39423282786765590, -8.543200923198597252, 57.16978962524147789 ) ) ;
#16001 = ORIENTED_EDGE ( 'NONE', *, *, #10035, .F. ) ;
#16002 = LINE ( 'NONE', #519, #3493 ) ;
#16003 = CARTESIAN_POINT ( 'NONE',  ( -13.18342752238402582, -20.93459749068556874, 58.09004124675303160 ) ) ;
#16004 = DIRECTION ( 'NONE',  ( -1.000000000000000000, 0.000000000000000000, 0.000000000000000000 ) ) ;
#16005 = CARTESIAN_POINT ( 'NONE',  ( -27.42409385541305511, -25.10920654474410441, 54.99999999999997868 ) ) ;
#16006 = PLANE ( 'NONE',  #16030 ) ;
#16007 = ORIENTED_EDGE ( 'NONE', *, *, #19760, .F. ) ;
#16008 = ORIENTED_EDGE ( 'NONE', *, *, #8083, .F. ) ;
#16009 = CARTESIAN_POINT ( 'NONE',  ( -18.63018860987378389, -7.457396320151260305, 73.95569119842126327 ) ) ;
#16010 = DIRECTION ( 'NONE',  ( 5.104528489711356381E-07, 5.317498756133547718E-07, 0.9999999999997283284 ) ) ;
#16011 = ORIENTED_EDGE ( 'NONE', *, *, #32984, .F. ) ;
#16012 = CARTESIAN_POINT ( 'NONE',  ( -22.28468842640968006, -19.91619389767071269, 65.98949666203347419 ) ) ;
#16013 = CARTESIAN_POINT ( 'NONE',  ( -20.01098570613759975, -18.73139293731311383, 49.52966884056656482 ) ) ;
#16014 = CARTESIAN_POINT ( 'NONE',  ( -22.21784385759799108, -6.860780111191487229, 51.02154966934377001 ) ) ;
#16015 = CARTESIAN_POINT ( 'NONE',  ( -10.48067351556794158, -16.03044098841782628, 68.27767830705533925 ) ) ;
#16016 = EDGE_CURVE ( 'NONE', #20234, #48679, #46736, .T. ) ;
#16017 = CARTESIAN_POINT ( 'NONE',  ( -21.60438134605806226, -20.97601912272344293, 72.70163284247159652 ) ) ;
#16018 = CARTESIAN_POINT ( 'NONE',  ( -15.82706446313400939, -7.992505727924407388, 70.68160198162291863 ) ) ;
#16019 = CARTESIAN_POINT ( 'NONE',  ( -14.09914643654217947, -8.649277595337252933, 74.49954655170296292 ) ) ;
#16020 = EDGE_CURVE ( 'NONE', #14239, #37402, #2105, .T. ) ;
#16021 = ORIENTED_EDGE ( 'NONE', *, *, #29551, .F. ) ;
#16022 = CARTESIAN_POINT ( 'NONE',  ( -17.42409385541306222, -14.80920654474411080, 82.49999999999998579 ) ) ;
#16023 = EDGE_CURVE ( 'NONE', #20442, #28963, #3853, .T. ) ;
#16024 = DIRECTION ( 'NONE',  ( -3.071710424422018668E-17, 6.404604876783312462E-16, 1.000000000000000000 ) ) ;
#16025 = DIRECTION ( 'NONE',  ( 1.000000000000000000, -4.164305804376849788E-17, 1.614929280266638808E-16 ) ) ;
#16026 = CARTESIAN_POINT ( 'NONE',  ( -17.59211730330735435, -7.811223398082945302, 63.85057029380297422 ) ) ;
#16027 = CARTESIAN_POINT ( 'NONE',  ( -30.42409385541305156, -6.859206544744110623, 52.99999999999997158 ) ) ;
#16028 = ORIENTED_EDGE ( 'NONE', *, *, #11107, .F. ) ;
#16029 = EDGE_LOOP ( 'NONE', ( #48018, #21146, #25549, #20060, #44973 ) ) ;
#16030 = AXIS2_PLACEMENT_3D ( 'NONE', #2460, #14237, #21429 ) ;
#16031 = FACE_OUTER_BOUND ( 'NONE', #23754, .T. ) ;
#16032 = ORIENTED_EDGE ( 'NONE', *, *, #11511, .T. ) ;
#16033 = CARTESIAN_POINT ( 'NONE',  ( -11.34829033918305718, -18.40080557649748272, 64.89140246238697785 ) ) ;
#16034 = VECTOR ( 'NONE', #47635, 1000.000000000000000 ) ;
#16035 = CARTESIAN_POINT ( 'NONE',  ( -18.48682678124872680, -7.839616045628057250, 74.13504580984984216 ) ) ;
#16036 =( BOUNDED_SURFACE ( )  B_SPLINE_SURFACE ( 3, 1, ( 
 ( #36593, #24819 ),
 ( #17653, #32906 ),
 ( #39588, #25062 ),
 ( #17417, #44036 ),
 ( #29236, #48184 ),
 ( #21377, #13472 ),
 ( #2157, #43298 ) ),
 .UNSPECIFIED., .T., .F., .F. ) 
 B_SPLINE_SURFACE_WITH_KNOTS ( ( 4, 3, 4 ),
 ( 2, 2 ),
 ( 0.000000000000000000, 0.5000000000000000000, 1.000000000000000000 ),
 ( 0.000000000000000000, 1.000000000000000000 ),
 .UNSPECIFIED. ) 
 GEOMETRIC_REPRESENTATION_ITEM ( )  RATIONAL_B_SPLINE_SURFACE ( (
 ( 1.000000000000000000, 1.000000000000000000),
 ( 0.3333333333333335369, 0.3333333333333330373),
 ( 0.3333333333333335369, 0.3333333333333330373),
 ( 1.000000000000000000, 1.000000000000000000),
 ( 0.3333333333333333703, 0.3333333333333333703),
 ( 0.3333333333333333703, 0.3333333333333333703),
 ( 1.000000000000000000, 1.000000000000000000) ) ) 
 REPRESENTATION_ITEM ( '' )  SURFACE ( )  );
#16037 = EDGE_LOOP ( 'NONE', ( #9648, #21640, #48640, #45482, #26104 ) ) ;
#16038 = DIRECTION ( 'NONE',  ( -3.071710424422018668E-17, 6.404604876783312462E-16, 1.000000000000000000 ) ) ;
#16039 = CARTESIAN_POINT ( 'NONE',  ( -11.23900738907041941, -11.53116396801028287, 64.37555317960440959 ) ) ;
#16040 = VERTEX_POINT ( 'NONE', #16433 ) ;
#16041 = CARTESIAN_POINT ( 'NONE',  ( -17.42409385541299471, -14.80920654474435771, 49.52966884056655772 ) ) ;
#16042 = CYLINDRICAL_SURFACE ( 'NONE', #44629, 0.1499999999999977185 ) ;
#16043 = VERTEX_POINT ( 'NONE', #1907 ) ;
#16044 = CARTESIAN_POINT ( 'NONE',  ( -19.60932529797995727, -21.51514414075818493, 69.34971148877966129 ) ) ;
#16045 =( BOUNDED_CURVE ( )  B_SPLINE_CURVE ( 3, ( #32384, #10687, #13638, #21541 ),
 .UNSPECIFIED., .F., .F. ) 
 B_SPLINE_CURVE_WITH_KNOTS ( ( 4, 4 ),
 ( 0.9074455897393624015, 1.000000000000000000 ),
 .UNSPECIFIED. ) 
 CURVE ( )  GEOMETRIC_REPRESENTATION_ITEM ( )  RATIONAL_B_SPLINE_CURVE ( ( 0.6983129098260905110, 0.7760317562606959818, 0.8765941196519991818, 1.000000000000000000 ) ) 
 REPRESENTATION_ITEM ( '' )  );
#16046 = CARTESIAN_POINT ( 'NONE',  ( -13.53974279883776255, -21.16658004109286040, 65.16345737345569944 ) ) ;
#16047 = ORIENTED_EDGE ( 'NONE', *, *, #29658, .F. ) ;
#16048 = CARTESIAN_POINT ( 'NONE',  ( -11.14521337614216101, -10.79921377940424954, 57.33186350582411706 ) ) ;
#16049 = DIRECTION ( 'NONE',  ( -5.551115123125782702E-17, -1.232595164407830946E-32, -1.000000000000000000 ) ) ;
#16050 = ADVANCED_FACE ( 'NONE', ( #8583 ), #31948, .T. ) ;
#16051 = CARTESIAN_POINT ( 'NONE',  ( -17.22979626510402085, -7.361617988748135666, 70.66848571475107121 ) ) ;
#16052 = ORIENTED_EDGE ( 'NONE', *, *, #8939, .T. ) ;
#16053 = CARTESIAN_POINT ( 'NONE',  ( -19.71243449262119896, -21.42506837973052214, 68.95099091562512683 ) ) ;
#16054 = CARTESIAN_POINT ( 'NONE',  ( -17.76560209638259025, -21.80099384504234550, 58.70553380167749680 ) ) ;
#16055 = CARTESIAN_POINT ( 'NONE',  ( -11.59533477946176738, -10.16928643397592325, 71.07618957754787914 ) ) ;
#16056 = CARTESIAN_POINT ( 'NONE',  ( -21.24416713127566325, -21.20535426119284139, 65.62808000370414163 ) ) ;
#16057 = CARTESIAN_POINT ( 'NONE',  ( -18.67235195658554403, -19.33882101600501713, 49.52966884056656482 ) ) ;
#16058 = DIRECTION ( 'NONE',  ( -3.071710424422018668E-17, 6.404604876783312462E-16, 1.000000000000000000 ) ) ;
#16059 =( BOUNDED_SURFACE ( )  B_SPLINE_SURFACE ( 3, 1, ( 
 ( #44952, #11205 ),
 ( #19068, #15352 ),
 ( #11432, #45430 ),
 ( #11683, #26710 ),
 ( #41725, #46642 ),
 ( #1814, #1083 ),
 ( #1568, #31619 ) ),
 .UNSPECIFIED., .T., .F., .F. ) 
 B_SPLINE_SURFACE_WITH_KNOTS ( ( 4, 3, 4 ),
 ( 2, 2 ),
 ( 0.000000000000000000, 0.5000000000000000000, 1.000000000000000000 ),
 ( 0.000000000000000000, 1.000000000000000000 ),
 .UNSPECIFIED. ) 
 GEOMETRIC_REPRESENTATION_ITEM ( )  RATIONAL_B_SPLINE_SURFACE ( (
 ( 1.000000000000000000, 1.000000000000000000),
 ( 0.3333333333333335369, 0.3333333333333330373),
 ( 0.3333333333333335369, 0.3333333333333330373),
 ( 1.000000000000000000, 1.000000000000000000),
 ( 0.3333333333333333703, 0.3333333333333333703),
 ( 0.3333333333333333703, 0.3333333333333333703),
 ( 1.000000000000000000, 1.000000000000000000) ) ) 
 REPRESENTATION_ITEM ( '' )  SURFACE ( )  );
#16060 = CARTESIAN_POINT ( 'NONE',  ( -19.85891393954322837, -21.37210614461000446, 47.99999999999994316 ) ) ;
#16061 = DIRECTION ( 'NONE',  ( 0.9774082387306984865, -0.2113602016968848807, 7.903122840289808494E-08 ) ) ;
#16062 = CARTESIAN_POINT ( 'NONE',  ( -11.10681587527927938, -11.67891925637714401, 71.10332952723315714 ) ) ;
#16063 = CARTESIAN_POINT ( 'NONE',  ( -14.59284385650551741, -7.406986770994972602, 48.81910596585309747 ) ) ;
#16064 = AXIS2_PLACEMENT_3D ( 'NONE', #47281, #20928, #28564 ) ;
#16065 = ORIENTED_EDGE ( 'NONE', *, *, #32650, .F. ) ;
#16066 = CARTESIAN_POINT ( 'NONE',  ( -21.66247382830096768, -9.170857770714572865, 63.19153610464900339 ) ) ;
#16067 = CARTESIAN_POINT ( 'NONE',  ( -11.02793337088870729, -10.98921060197374722, 60.87224103154665045 ) ) ;
#16068 = EDGE_LOOP ( 'NONE', ( #37, #1050, #28071, #46616, #45351 ) ) ;
#16069 = CARTESIAN_POINT ( 'NONE',  ( -24.72409385541305582, -14.80920654474415699, 62.92941176470587550 ) ) ;
#16070 = CARTESIAN_POINT ( 'NONE',  ( -10.78171168112265832, -12.44661727924501449, 57.62857332509076969 ) ) ;
#16071 = CARTESIAN_POINT ( 'NONE',  ( -23.26235167723834962, -10.18112620132981228, 63.19469118497043780 ) ) ;
#16072 = CARTESIAN_POINT ( 'NONE',  ( -20.51885330616224579, -21.64595032723701706, 54.15157107980257933 ) ) ;
#16073 = VERTEX_POINT ( 'NONE', #34910 ) ;
#16074 = CARTESIAN_POINT ( 'NONE',  ( -24.40552668661833735, -14.29970115358017502, 66.37395989550236663 ) ) ;
#16075 = EDGE_CURVE ( 'NONE', #5574, #32131, #19738, .T. ) ;
#16076 = FACE_OUTER_BOUND ( 'NONE', #4257, .T. ) ;
#16077 = CARTESIAN_POINT ( 'NONE',  ( -24.02981955162125516, -11.36410642080215894, 66.60027269894509061 ) ) ;
#16078 = ADVANCED_FACE ( 'NONE', ( #46249 ), #19937, .T. ) ;
#16079 = EDGE_CURVE ( 'NONE', #23975, #6043, #38472, .T. ) ;
#16080 = ORIENTED_EDGE ( 'NONE', *, *, #2685, .F. ) ;
#16081 = CARTESIAN_POINT ( 'NONE',  ( -17.53499440593470737, -7.752105970505813737, 70.63468544436783247 ) ) ;
#16082 = CARTESIAN_POINT ( 'NONE',  ( -24.17899325218984785, -11.66673737571591296, 59.66731058339561855 ) ) ;
#16083 = CARTESIAN_POINT ( 'NONE',  ( -10.40245588357037043, -14.17414831712846990, 61.20349182037644198 ) ) ;
#16084 = CARTESIAN_POINT ( 'NONE',  ( -21.75000248771700129, -8.743799152774244021, 70.23108901470999399 ) ) ;
#16085 = DIRECTION ( 'NONE',  ( 2.526377665399295826E-06, 1.273612633031948423E-05, -0.9999999999157042074 ) ) ;
#16086 = ORIENTED_EDGE ( 'NONE', *, *, #32853, .T. ) ;
#16087 = ORIENTED_EDGE ( 'NONE', *, *, #3325, .F. ) ;
#16088 = CARTESIAN_POINT ( 'NONE',  ( -20.55534385541304232, -8.623186033802570094, 49.24843789510466507 ) ) ;
#16089 = CARTESIAN_POINT ( 'NONE',  ( -24.72409385541305582, -14.80920654474421205, 67.95882352941174531 ) ) ;
#16090 = DIRECTION ( 'NONE',  ( 0.7915359335728472390, 0.6111226275167354061, 5.146443701300905010E-08 ) ) ;
#16091 = VECTOR ( 'NONE', #5367, 1000.000000000000114 ) ;
#16092 = CARTESIAN_POINT ( 'NONE',  ( -10.81484411697162962, -17.11524594140972155, 61.15743118925659161 ) ) ;
#16093 = EDGE_CURVE ( 'NONE', #19353, #25093, #36355, .T. ) ;
#16094 = VECTOR ( 'NONE', #27509, 1000.000000000000000 ) ;
#16095 = CARTESIAN_POINT ( 'NONE',  ( -13.85393748347032528, -8.270264590973253505, 74.38449983516251507 ) ) ;
#16096 = ORIENTED_EDGE ( 'NONE', *, *, #31645, .T. ) ;
#16097 = CARTESIAN_POINT ( 'NONE',  ( -40.64308517176574753, -25.10920654474410441, 77.24806946917840378 ) ) ;
#16098 = CARTESIAN_POINT ( 'NONE',  ( -10.38888248908913958, -14.35051868308065437, 64.68244075910853041 ) ) ;
#16099 = ORIENTED_EDGE ( 'NONE', *, *, #14486, .F. ) ;
#16100 = CARTESIAN_POINT ( 'NONE',  ( -13.36402663293916682, -21.05582000094733530, 61.63833528390372152 ) ) ;
#16101 = EDGE_LOOP ( 'NONE', ( #18168, #36620, #14495, #17187, #16291 ) ) ;
#16102 = LINE ( 'NONE', #15623, #12810 ) ;
#16103 = EDGE_CURVE ( 'NONE', #16763, #25179, #26848, .T. ) ;
#16104 = CARTESIAN_POINT ( 'NONE',  ( -21.92407967000237790, -20.23628646485057914, 58.76442916245459003 ) ) ;
#16105 = EDGE_CURVE ( 'NONE', #37668, #40518, #42228, .T. ) ;
#16106 = CARTESIAN_POINT ( 'NONE',  ( -15.13863373983067717, -21.47863424849249014, 65.40036913793611006 ) ) ;
#16107 = CARTESIAN_POINT ( 'NONE',  ( -22.48114103837971101, -19.64927616005747879, 72.64400547034465205 ) ) ;
#16108 = EDGE_LOOP ( 'NONE', ( #13318, #32866, #40552, #35273, #2531 ) ) ;
#16109 = CARTESIAN_POINT ( 'NONE',  ( -18.71262049920375503, -21.74350751539899562, 72.17022092985547488 ) ) ;
#16110 = CARTESIAN_POINT ( 'NONE',  ( -17.77063367917941861, -22.25119205618777585, 58.51215086126244103 ) ) ;
#16111 = CARTESIAN_POINT ( 'NONE',  ( -10.88583436550758776, -11.23762803245173103, 64.30915376540053785 ) ) ;
#16112 = FACE_BOUND ( 'NONE', #10605, .T. ) ;
#16113 = ITEM_DEFINED_TRANSFORMATION ( 'NONE', 'NONE', #3890,  #29031 ) ;
#16114 = B_SPLINE_CURVE_WITH_KNOTS ( 'NONE', 1,
 ( #13368, #17552 ),
 .UNSPECIFIED., .F., .F.,
 ( 2, 2 ),
 ( 0.000000000000000000, 1.000000000000000000 ),
 .UNSPECIFIED. ) ;
#16115 = CARTESIAN_POINT ( 'NONE',  ( -22.83929682888979329, -10.29453308790037980, 66.55654356380499337 ) ) ;
#16116 = CYLINDRICAL_SURFACE ( 'NONE', #35787, 0.1499999999999985234 ) ;
#16117 = B_SPLINE_CURVE_WITH_KNOTS ( 'NONE', 3,
 ( #8349, #11547, #1185, #19675, #7875, #7632, #12040, #22637, #37633, #26573 ),
 .UNSPECIFIED., .F., .F.,
 ( 4, 2, 2, 2, 4 ),
 ( 0.6272669072878104268, 0.7522669073073157131, 0.8772669073268208884, 1.002266907346326175, 1.127266907365831461 ),
 .UNSPECIFIED. ) ;
#16118 = CARTESIAN_POINT ( 'NONE',  ( -36.42409385541304800, -9.359200813967566646, 50.49621490985803263 ) ) ;
#16119 = ORIENTED_EDGE ( 'NONE', *, *, #22985, .T. ) ;
#16120 = CARTESIAN_POINT ( 'NONE',  ( -12.08002915394404120, -10.28786663478488350, 67.79896886176341297 ) ) ;
#16121 = VERTEX_POINT ( 'NONE', #48175 ) ;
#16122 = CARTESIAN_POINT ( 'NONE',  ( -20.08713612207380450, -21.76716563359125800, 72.56625224360259097 ) ) ;
#16123 = LINE ( 'NONE', #15394, #19590 ) ;
#16124 = B_SPLINE_CURVE_WITH_KNOTS ( 'NONE', 3,
 ( #29592, #3737, #41163, #52, #6946, #11609, #3990, #7693, #44623, #21962 ),
 .UNSPECIFIED., .F., .F.,
 ( 4, 2, 2, 2, 4 ),
 ( 0.000000000000000000, 0.2500000000000000000, 0.5000000000000000000, 0.7500000000000000000, 1.000000000000000000 ),
 .UNSPECIFIED. ) ;
#16125 = ORIENTED_EDGE ( 'NONE', *, *, #20351, .T. ) ;
#16126 = CYLINDRICAL_SURFACE ( 'NONE', #1204, 0.1499999999999994671 ) ;
#16127 = AXIS2_PLACEMENT_3D ( 'NONE', #17769, #32797, #3253 ) ;
#16128 = FACE_BOUND ( 'NONE', #37477, .T. ) ;
#16129 = ORIENTED_EDGE ( 'NONE', *, *, #10303, .T. ) ;
#16130 = EDGE_CURVE ( 'NONE', #24230, #6612, #17640, .T. ) ;
#16131 = ADVANCED_FACE ( 'NONE', ( #5854 ), #9872, .T. ) ;
#16132 = ORIENTED_EDGE ( 'NONE', *, *, #13890, .F. ) ;
#16133 = VERTEX_POINT ( 'NONE', #21115 ) ;
#16134 = CARTESIAN_POINT ( 'NONE',  ( -18.25645571269274825, -21.81792545032241293, 62.03103110229211836 ) ) ;
#16135 = CARTESIAN_POINT ( 'NONE',  ( -13.14999064602648637, -9.265557826385967033, 67.37942786034257381 ) ) ;
#16136 = CARTESIAN_POINT ( 'NONE',  ( -24.44055745662519641, -14.11932379769929113, 73.13743607903229815 ) ) ;
#16137 = FACE_OUTER_BOUND ( 'NONE', #28248, .T. ) ;
#16138 = CARTESIAN_POINT ( 'NONE',  ( -12.65491863400508876, -19.93331718326324165, 68.33657436096362403 ) ) ;
#16139 = CARTESIAN_POINT ( 'NONE',  ( -10.75331649400429868, -16.93069871048427544, 57.68760548944693056 ) ) ;
#16140 = ORIENTED_EDGE ( 'NONE', *, *, #436, .T. ) ;
#16141 = VERTEX_POINT ( 'NONE', #36112 ) ;
#16142 = EDGE_CURVE ( 'NONE', #9880, #5480, #13851, .T. ) ;
#16143 = ADVANCED_FACE ( 'NONE', ( #6580, #36582 ), #40786, .F. ) ;
#16144 = CARTESIAN_POINT ( 'NONE',  ( -22.61159385650551457, -6.922745924619793101, 51.69366785382590024 ) ) ;
#16145 = EDGE_CURVE ( 'NONE', #10344, #43128, #20218, .T. ) ;
#16146 = CARTESIAN_POINT ( 'NONE',  ( -21.29196722032537537, -20.70380199363843232, 72.53918572867779346 ) ) ;
#16147 = CARTESIAN_POINT ( 'NONE',  ( -10.52311507911083055, -15.98310348350391230, 68.27767878681093805 ) ) ;
#16148 = CARTESIAN_POINT ( 'NONE',  ( -12.73887154267113253, -15.16169402761809870, 52.02966884056656482 ) ) ;
#16149 = ADVANCED_FACE ( 'NONE', ( #14903 ), #34359, .T. ) ;
#16150 = ORIENTED_EDGE ( 'NONE', *, *, #24281, .T. ) ;
#16151 = CARTESIAN_POINT ( 'NONE',  ( -22.94909385650551314, -8.104110260919577868, 48.81699501597546487 ) ) ;
#16152 = ORIENTED_EDGE ( 'NONE', *, *, #12760, .F. ) ;
#16153 = DIRECTION ( 'NONE',  ( -0.5881408891789769999, -0.8087584895849666555, 7.565907428972491290E-08 ) ) ;
#16154 = ADVANCED_FACE ( 'NONE', ( #41041 ), #26757, .T. ) ;
#16155 = CARTESIAN_POINT ( 'NONE',  ( -12.41310947992116098, -19.76871611099698001, 61.68206578716802113 ) ) ;
#16156 = CARTESIAN_POINT ( 'NONE',  ( -17.42409385541300892, -14.80920654474439679, 47.99999999999994316 ) ) ;
#16157 = ORIENTED_EDGE ( 'NONE', *, *, #44079, .T. ) ;
#16158 = FACE_OUTER_BOUND ( 'NONE', #33277, .T. ) ;
#16159 = LINE ( 'NONE', #38830, #2358 ) ;
#16160 = CARTESIAN_POINT ( 'NONE',  ( -10.71605034603323148, -17.00400043661996108, 64.77172137060364321 ) ) ;
#16161 = DIRECTION ( 'NONE',  ( 1.000000000000000000, 0.000000000000000000, 0.000000000000000000 ) ) ;
#16162 =( REPRESENTATION_RELATIONSHIP ('NONE','NONE', #2768, #34837 ) REPRESENTATION_RELATIONSHIP_WITH_TRANSFORMATION ( #16113 )SHAPE_REPRESENTATION_RELATIONSHIP( ) );
#16163 = ORIENTED_EDGE ( 'NONE', *, *, #2829, .F. ) ;
#16164 = CARTESIAN_POINT ( 'NONE',  ( -10.45256735519816615, -15.43993469624229853, 57.56792809193251514 ) ) ;
#16165 = CARTESIAN_POINT ( 'NONE',  ( -23.85748962928175132, -11.92509172808648543, 59.49707787073156595 ) ) ;
#16166 = CARTESIAN_POINT ( 'NONE',  ( -12.40538999107997498, -20.31523868419091272, 68.52152871938794476 ) ) ;
#16167 = ORIENTED_EDGE ( 'NONE', *, *, #5052, .T. ) ;
#16168 = FACE_OUTER_BOUND ( 'NONE', #29755, .T. ) ;
#16169 = ORIENTED_EDGE ( 'NONE', *, *, #19039, .T. ) ;
#16170 = CARTESIAN_POINT ( 'NONE',  ( -15.06305009558132646, -21.87596932251961590, 65.21941411614068329 ) ) ;
#16171 = DIRECTION ( 'NONE',  ( 0.9294853595766542353, 0.3688590060343623911, 0.000000000000000000 ) ) ;
#16172 = B_SPLINE_CURVE_WITH_KNOTS ( 'NONE', 1,
 ( #25533, #3124 ),
 .UNSPECIFIED., .F., .F.,
 ( 2, 2 ),
 ( 0.000000000000000000, 1.000000000000000000 ),
 .UNSPECIFIED. ) ;
#16173 = ORIENTED_EDGE ( 'NONE', *, *, #13543, .F. ) ;
#16174 = CARTESIAN_POINT ( 'NONE',  ( -22.19081608276703221, -20.53467296680696563, 58.96454102209866477 ) ) ;
#16175 = CARTESIAN_POINT ( 'NONE',  ( -46.29409385541305255, -12.76354662275040219, 69.95698270748289360 ) ) ;
#16176 = CARTESIAN_POINT ( 'NONE',  ( -24.25372049150513831, -13.26839097538318946, 63.06094141181949198 ) ) ;
#16177 = CARTESIAN_POINT ( 'NONE',  ( -10.43073325114686511, -14.50439929630985603, 68.15800126138398696 ) ) ;
#16178 = VERTEX_POINT ( 'NONE', #30217 ) ;
#16179 = CARTESIAN_POINT ( 'NONE',  ( -21.34582024633207098, -20.66775256773563285, 72.67446429491059234 ) ) ;
#16180 = DIRECTION ( 'NONE',  ( -0.8604039311673230550, -0.5096126717731922495, 7.110477544621476444E-08 ) ) ;
#16181 = EDGE_CURVE ( 'NONE', #22557, #39502, #32629, .T. ) ;
#16182 = CARTESIAN_POINT ( 'NONE',  ( -23.58525830889974984, -18.99772868593042219, 65.86743475655129032 ) ) ;
#16183 =( BOUNDED_CURVE ( )  B_SPLINE_CURVE ( 3, ( #28190, #20571, #32377, #47630 ),
 .UNSPECIFIED., .F., .F. ) 
 B_SPLINE_CURVE_WITH_KNOTS ( ( 4, 4 ),
 ( 0.9074455897393697290, 1.000000000000000000 ),
 .UNSPECIFIED. ) 
 CURVE ( )  GEOMETRIC_REPRESENTATION_ITEM ( )  RATIONAL_B_SPLINE_CURVE ( ( 0.6983129098260940637, 0.7760317562606990904, 0.8765941196520010692, 1.000000000000000000 ) ) 
 REPRESENTATION_ITEM ( '' )  );
#16184 = CARTESIAN_POINT ( 'NONE',  ( -22.27817919856018136, -9.157513542003881568, 59.83675792137641736 ) ) ;
#16185 = ORIENTED_EDGE ( 'NONE', *, *, #33872, .T. ) ;
#16186 = CARTESIAN_POINT ( 'NONE',  ( -15.68463861365884249, -7.564349260043091938, 67.25351876580783994 ) ) ;
#16187 = CARTESIAN_POINT ( 'NONE',  ( -33.42409385541304800, -8.109206544743658540, 50.50000000000030553 ) ) ;
#16188 = EDGE_CURVE ( 'NONE', #35450, #12002, #44749, .T. ) ;
#16189 = ORIENTED_EDGE ( 'NONE', *, *, #34171, .T. ) ;
#16190 = ORIENTED_EDGE ( 'NONE', *, *, #20467, .F. ) ;
#16191 = CYLINDRICAL_SURFACE ( 'NONE', #2366, 1.999999999999999556 ) ;
#16192 = CARTESIAN_POINT ( 'NONE',  ( -23.83833621072449560, -17.61232891644574394, 62.47360984984814536 ) ) ;
#16193 = FACE_OUTER_BOUND ( 'NONE', #8236, .T. ) ;
#16194 = CARTESIAN_POINT ( 'NONE',  ( -20.21784385650551386, -9.790100578890868377, 49.79778022625163203 ) ) ;
#16195 = DIRECTION ( 'NONE',  ( 1.000000000000000000, -0.000000000000000000, 0.000000000000000000 ) ) ;
#16196 = DIRECTION ( 'NONE',  ( 3.071710424422018668E-17, -6.404604876783312462E-16, -1.000000000000000000 ) ) ;
#16197 =( BOUNDED_CURVE ( )  B_SPLINE_CURVE ( 3, ( #14055, #37195, #29104, #36956 ),
 .UNSPECIFIED., .F., .F. ) 
 B_SPLINE_CURVE_WITH_KNOTS ( ( 4, 4 ),
 ( 0.9074455897393632897, 1.000000000000000000 ),
 .UNSPECIFIED. ) 
 CURVE ( )  GEOMETRIC_REPRESENTATION_ITEM ( )  RATIONAL_B_SPLINE_CURVE ( ( 0.6983129098260867362, 0.7760317562606927622, 0.8765941196519971834, 1.000000000000000000 ) ) 
 REPRESENTATION_ITEM ( '' )  );
#16198 = CARTESIAN_POINT ( 'NONE',  ( -12.36756753426621813, -9.896138138887707214, 57.37463480816234096 ) ) ;
#16199 = AXIS2_PLACEMENT_3D ( 'NONE', #19562, #26715, #20293 ) ;
#16200 = ORIENTED_EDGE ( 'NONE', *, *, #30101, .F. ) ;
#16201 = EDGE_LOOP ( 'NONE', ( #30559, #19071, #11646, #22029, #26713 ) ) ;
#16202 = CARTESIAN_POINT ( 'NONE',  ( -10.99586753834015695, -11.04334891231907534, 60.86381058728009208 ) ) ;
#16203 = DIRECTION ( 'NONE',  ( 1.000000000000000000, 0.000000000000000000, 0.000000000000000000 ) ) ;
#16204 = EDGE_CURVE ( 'NONE', #6133, #24855, #7070, .T. ) ;
#16205 = CARTESIAN_POINT ( 'NONE',  ( -22.74909385541299400, -8.112991634885936776, 51.74999426922429535 ) ) ;
#16206 = CARTESIAN_POINT ( 'NONE',  ( -22.88264614489240856, -10.34704276773305764, 63.35713876973677827 ) ) ;
#16207 = EDGE_CURVE ( 'NONE', #21537, #12524, #30307, .T. ) ;
#16208 = ORIENTED_EDGE ( 'NONE', *, *, #16858, .T. ) ;
#16209 = CARTESIAN_POINT ( 'NONE',  ( -14.13242279744181573, -8.574497162196568212, 74.21426705364891063 ) ) ;
#16210 = CARTESIAN_POINT ( 'NONE',  ( -10.78031428196279329, -11.32923628920978310, 53.49999999999994316 ) ) ;
#16211 = CARTESIAN_POINT ( 'NONE',  ( -17.17171767447154096, -7.760110763219655539, 67.22859634205599377 ) ) ;
#16212 = CARTESIAN_POINT ( 'NONE',  ( -15.83638662446498380, -7.530183628806756957, 67.30153828690920648 ) ) ;
#16213 = EDGE_CURVE ( 'NONE', #19324, #20830, #33710, .T. ) ;
#16214 = ORIENTED_EDGE ( 'NONE', *, *, #550, .T. ) ;
#16215 = DIRECTION ( 'NONE',  ( -3.071710424422018668E-17, 6.404604876783312462E-16, 1.000000000000000000 ) ) ;
#16216 = DIRECTION ( 'NONE',  ( -5.731567514496413899E-31, -1.020425574103664789E-16, -1.000000000000000000 ) ) ;
#16217 = PRODUCT_DEFINITION ( 'UNKNOWN', '', #46344, #38610 ) ;
#16218 = ORIENTED_EDGE ( 'NONE', *, *, #45271, .F. ) ;
#16219 = CARTESIAN_POINT ( 'NONE',  ( -22.63560516303400050, -20.13310814558360917, 69.28922553891734992 ) ) ;
#16220 = PLANE ( 'NONE',  #10802 ) ;
#16221 = ORIENTED_EDGE ( 'NONE', *, *, #34838, .F. ) ;
#16222 = CARTESIAN_POINT ( 'NONE',  ( -23.69601271365505823, -18.82994329453045168, 69.48646111030700467 ) ) ;
#16223 = AXIS2_PLACEMENT_3D ( 'NONE', #11070, #33439, #3931 ) ;
#16224 = AXIS2_PLACEMENT_3D ( 'NONE', #37397, #33458, #2947 ) ;
#16225 = ORIENTED_EDGE ( 'NONE', *, *, #30544, .T. ) ;
#16226 = DIRECTION ( 'NONE',  ( 1.206829990107966821E-05, 1.995688255855010801E-06, 0.9999999999251867333 ) ) ;
#16227 = DIRECTION ( 'NONE',  ( 1.000000000000000000, 0.000000000000000000, -9.637352644315596475E-17 ) ) ;
#16228 = ORIENTED_EDGE ( 'NONE', *, *, #4722, .T. ) ;
#16229 = CARTESIAN_POINT ( 'NONE',  ( -24.23700366861210753, -17.82382531738836562, 62.73006892227505915 ) ) ;
#16230 = CARTESIAN_POINT ( 'NONE',  ( -10.37462440636232053, -14.89569459299594278, 75.09778901493891112 ) ) ;
#16231 = CARTESIAN_POINT ( 'NONE',  ( -17.26784385650551457, -6.428312510596451368, 51.20221977374900035 ) ) ;
#16232 = CARTESIAN_POINT ( 'NONE',  ( -12.01398263875733718, -10.36526583719368233, 71.04063403505170982 ) ) ;
#16233 = CIRCLE ( 'NONE', #39845, 2.000000000000001776 ) ;
#16234 = EDGE_CURVE ( 'NONE', #40830, #47966, #4117, .T. ) ;
#16235 = CARTESIAN_POINT ( 'NONE',  ( -18.53667165497532920, -10.24437071140730993, 52.02966884056656482 ) ) ;
#16236 = CARTESIAN_POINT ( 'NONE',  ( -14.66844689667836299, -21.73163918518723037, 61.82255689998408599 ) ) ;
#16237 = ORIENTED_EDGE ( 'NONE', *, *, #5260, .T. ) ;
#16238 = CARTESIAN_POINT ( 'NONE',  ( -12.27729925481933471, -9.991218852276039897, 60.55918086709623083 ) ) ;
#16239 = CARTESIAN_POINT ( 'NONE',  ( -11.97212546196701943, -10.32690635925306211, 74.58318462221375000 ) ) ;
#16240 = DIRECTION ( 'NONE',  ( 1.000000000000000000, 1.669677910507523057E-21, 6.493791346278465266E-22 ) ) ;
#16241 = CARTESIAN_POINT ( 'NONE',  ( -48.42409385541304800, -27.10920654474410796, 47.99999999999998579 ) ) ;
#16242 = CARTESIAN_POINT ( 'NONE',  ( -12.20424117383341311, -20.12491952255346206, 65.12320790045656338 ) ) ;
#16243 = ORIENTED_EDGE ( 'NONE', *, *, #2089, .F. ) ;
#16244 = ORIENTED_EDGE ( 'NONE', *, *, #27858, .T. ) ;
#16245 = FACE_OUTER_BOUND ( 'NONE', #10592, .T. ) ;
#16246 = CARTESIAN_POINT ( 'NONE',  ( -10.33669513760112224, -12.51310759931308070, 60.99127726887360978 ) ) ;
#16247 = EDGE_LOOP ( 'NONE', ( #7069, #47814, #41802, #48290, #27109 ) ) ;
#16248 = CARTESIAN_POINT ( 'NONE',  ( -24.35072239393756632, -15.82005629120157231, 66.17210830061728188 ) ) ;
#16249 = CARTESIAN_POINT ( 'NONE',  ( -15.77564557227241160, -7.543859306641682139, 67.23983639585463834 ) ) ;
#16250 = CARTESIAN_POINT ( 'NONE',  ( -10.27590366065288485, -12.71001274655382041, 64.37497800382601554 ) ) ;
#16251 = CARTESIAN_POINT ( 'NONE',  ( -15.56465948913149333, -7.543361525925791788, 53.27966884056655061 ) ) ;
#16252 = CARTESIAN_POINT ( 'NONE',  ( -17.07160637253920044, -10.12398423200249731, 49.52966884056655772 ) ) ;
#16253 = CYLINDRICAL_SURFACE ( 'NONE', #24739, 5.249999999999998224 ) ;
#16254 = FACE_OUTER_BOUND ( 'NONE', #46797, .T. ) ;
#16255 = ORIENTED_EDGE ( 'NONE', *, *, #7501, .F. ) ;
#16256 = CARTESIAN_POINT ( 'NONE',  ( -42.04247620835423049, -14.80920654474420139, 66.05294117647058272 ) ) ;
#16257 = FILL_AREA_STYLE_COLOUR ( '', #38407 ) ;
#16258 = ADVANCED_FACE ( 'NONE', ( #45730 ), #22321, .F. ) ;
#16259 = CARTESIAN_POINT ( 'NONE',  ( -23.25757715627672795, -10.17517474196413474, 63.18690702823881367 ) ) ;
#16260 = CARTESIAN_POINT ( 'NONE',  ( -13.84034316733854730, -20.82276307383959946, 68.47241820953060198 ) ) ;
#16261 = CARTESIAN_POINT ( 'NONE',  ( -17.42127804818254688, -7.759166751185505362, 67.02039588450487884 ) ) ;
#16262 = EDGE_CURVE ( 'NONE', #38614, #9358, #12484, .T. ) ;
#16263 = EDGE_LOOP ( 'NONE', ( #8338, #30862, #43426, #37071 ) ) ;
#16264 = VECTOR ( 'NONE', #35947, 1000.000000000000227 ) ;
#16265 = ORIENTED_EDGE ( 'NONE', *, *, #4037, .T. ) ;
#16266 = AXIS2_PLACEMENT_3D ( 'NONE', #17294, #9204, #24224 ) ;
#16267 = CARTESIAN_POINT ( 'NONE',  ( -19.79646526366146375, -21.45124607735644062, 72.81967355032548994 ) ) ;
#16268 = EDGE_CURVE ( 'NONE', #26197, #39806, #27311, .T. ) ;
#16269 = ORIENTED_EDGE ( 'NONE', *, *, #2131, .T. ) ;
#16270 = CARTESIAN_POINT ( 'NONE',  ( -23.36784385541299613, -9.357632978295908899, 49.97845033065679843 ) ) ;
#16271 = B_SPLINE_CURVE_WITH_KNOTS ( 'NONE', 3,
 ( #5778, #13375, #17317, #6003, #9474, #17065, #10439, #43692, #21026, #24963 ),
 .UNSPECIFIED., .F., .F.,
 ( 4, 2, 2, 2, 4 ),
 ( 0.000000000000000000, 0.2500000000000000000, 0.5000000000000000000, 0.7500000000000000000, 1.000000000000000000 ),
 .UNSPECIFIED. ) ;
#16272 = CARTESIAN_POINT ( 'NONE',  ( -10.96069643151774109, -18.51437482595545347, 57.92219192461608657 ) ) ;
#16273 =( BOUNDED_CURVE ( )  B_SPLINE_CURVE ( 3, ( #18261, #7213, #14788, #29856 ),
 .UNSPECIFIED., .F., .F. ) 
 B_SPLINE_CURVE_WITH_KNOTS ( ( 4, 4 ),
 ( 0.000000000000000000, 0.4074455897393664539 ),
 .UNSPECIFIED. ) 
 CURVE ( )  GEOMETRIC_REPRESENTATION_ITEM ( )  RATIONAL_B_SPLINE_CURVE ( ( 1.000000000000000000, 0.4567392136813308579, 0.3561768502900298783, 0.6983129098260970613 ) ) 
 REPRESENTATION_ITEM ( '' )  );
#16274 = EDGE_CURVE ( 'NONE', #29274, #42743, #18474, .T. ) ;
#16275 = EDGE_CURVE ( 'NONE', #29613, #43808, #9252, .T. ) ;
#16276 = VERTEX_POINT ( 'NONE', #5568 ) ;
#16277 = CARTESIAN_POINT ( 'NONE',  ( -17.42409385541300892, -14.80920654474439679, 56.49999999999994316 ) ) ;
#16278 = DIRECTION ( 'NONE',  ( 0.8839923186919885767, -0.4675014229855998793, 2.842058574697910297E-08 ) ) ;
#16279 = ORIENTED_EDGE ( 'NONE', *, *, #12621, .T. ) ;
#16280 = CARTESIAN_POINT ( 'NONE',  ( -17.72634068467203505, -21.85272461955047874, 58.70553378267869959 ) ) ;
#16281 = CARTESIAN_POINT ( 'NONE',  ( -10.47141000957850743, -13.99617255615227940, 57.46327426011240647 ) ) ;
#16282 = ORIENTED_EDGE ( 'NONE', *, *, #46524, .T. ) ;
#16283 = CARTESIAN_POINT ( 'NONE',  ( -10.82281966776723792, -12.48006615504498207, 57.32857332801585670 ) ) ;
#16284 = EDGE_CURVE ( 'NONE', #44255, #30207, #8778, .T. ) ;
#16285 = LINE ( 'NONE', #9171, #32210 ) ;
#16286 = EDGE_CURVE ( 'NONE', #445, #12446, #11982, .T. ) ;
#16287 = ORIENTED_EDGE ( 'NONE', *, *, #24122, .T. ) ;
#16288 = DIRECTION ( 'NONE',  ( 0.9939059412784551073, 0.1102314832132140626, 5.576311685107536405E-08 ) ) ;
#16289 = CARTESIAN_POINT ( 'NONE',  ( -22.23205057465639456, -20.50024631022522925, 58.94159781348408700 ) ) ;
#16290 = CARTESIAN_POINT ( 'NONE',  ( -42.68438797306012589, -14.90920654474413709, 60.91764705882351905 ) ) ;
#16291 = ORIENTED_EDGE ( 'NONE', *, *, #30824, .F. ) ;
#16292 = DIRECTION ( 'NONE',  ( -4.115385489419834812E-17, -0.9999954153791273948, -0.003028072113822188795 ) ) ;
#16293 = PLANE ( 'NONE',  #48557 ) ;
#16294 = EDGE_CURVE ( 'NONE', #31052, #34094, #37599, .T. ) ;
#16295 = CARTESIAN_POINT ( 'NONE',  ( -16.20999063017906749, -7.914000527602912172, 63.89841002104740397 ) ) ;
#16296 = CARTESIAN_POINT ( 'NONE',  ( -21.12380683100872858, -21.27649256055507365, 65.77109308171978341 ) ) ;
#16297 = CARTESIAN_POINT ( 'NONE',  ( -10.97703272106552319, -11.95613849865247680, 74.85280472847954059 ) ) ;
#16298 = CARTESIAN_POINT ( 'NONE',  ( -14.78754745127378634, -8.270772244812135909, 60.61996282000563241 ) ) ;
#16299 = CIRCLE ( 'NONE', #19482, 1.999999999999999556 ) ;
#16300 = VECTOR ( 'NONE', #35724, 1000.000000000000000 ) ;
#16301 = LINE ( 'NONE', #38225, #26589 ) ;
#16302 = CARTESIAN_POINT ( 'NONE',  ( -10.35661267713556022, -12.45241038966069347, 60.91358145539074798 ) ) ;
#16303 = CARTESIAN_POINT ( 'NONE',  ( -19.92499704562962037, -21.82691083785356057, 69.03508226000913339 ) ) ;
#16304 = CARTESIAN_POINT ( 'NONE',  ( -15.99909385650551741, -8.114302828567740988, 52.18300498402516041 ) ) ;
#16305 = EDGE_LOOP ( 'NONE', ( #11579, #36179, #38347, #46550, #40039 ) ) ;
#16306 = DIRECTION ( 'NONE',  ( -0.000000000000000000, -1.000000000000000000, -0.000000000000000000 ) ) ;
#16307 = ORIENTED_EDGE ( 'NONE', *, *, #47467, .T. ) ;
#16308 = CARTESIAN_POINT ( 'NONE',  ( -14.11063322135152909, -21.03236308526469855, 72.21135587486895702 ) ) ;
#16309 = DIRECTION ( 'NONE',  ( 3.071710424422018668E-17, -6.404604876783312462E-16, -1.000000000000000000 ) ) ;
#16310 = CARTESIAN_POINT ( 'NONE',  ( -16.15533939627269078, -22.15042573278388005, 58.39247240179898313 ) ) ;
#16311 = AXIS2_PLACEMENT_3D ( 'NONE', #27040, #42066, #38606 ) ;
#16312 = CARTESIAN_POINT ( 'NONE',  ( -24.46714309859813241, -14.49289777169556714, 66.18852495040353290 ) ) ;
#16313 = CARTESIAN_POINT ( 'NONE',  ( -18.78767905735283605, -20.13749289187802916, 54.07175714974878389 ) ) ;
#16314 = ORIENTED_EDGE ( 'NONE', *, *, #37527, .F. ) ;
#16315 = ADVANCED_FACE ( 'NONE', ( #30940 ), #32165, .T. ) ;
#16316 = LINE ( 'NONE', #2042, #20790 ) ;
#16317 = CARTESIAN_POINT ( 'NONE',  ( -14.28913879486226435, -8.050816564744696535, 67.37479651646088996 ) ) ;
#16318 = CARTESIAN_POINT ( 'NONE',  ( -14.54881252626503851, -21.68205518681590149, 58.27343714710344358 ) ) ;
#16319 = ORIENTED_EDGE ( 'NONE', *, *, #6496, .T. ) ;
#16320 = CARTESIAN_POINT ( 'NONE',  ( -18.46801905451614445, -7.836623195388688679, 74.12592262855558545 ) ) ;
#16321 = CARTESIAN_POINT ( 'NONE',  ( -17.42409385541299471, -14.80920654474438614, 2.029618040566568027 ) ) ;
#16322 = DIRECTION ( 'NONE',  ( 0.000000000000000000, 0.000000000000000000, 1.000000000000000000 ) ) ;
#16323 =( BOUNDED_CURVE ( )  B_SPLINE_CURVE ( 3, ( #32020, #44328, #17706, #40375 ),
 .UNSPECIFIED., .F., .F. ) 
 B_SPLINE_CURVE_WITH_KNOTS ( ( 4, 4 ),
 ( 0.9074455897393643999, 1.000000000000000000 ),
 .UNSPECIFIED. ) 
 CURVE ( )  GEOMETRIC_REPRESENTATION_ITEM ( )  RATIONAL_B_SPLINE_CURVE ( ( 0.6983129098260918433, 0.7760317562606970920, 0.8765941196519998480, 1.000000000000000000 ) ) 
 REPRESENTATION_ITEM ( '' )  );
#16324 = CARTESIAN_POINT ( 'NONE',  ( -21.72530822383671634, -8.726125037250696437, 70.25319750298596944 ) ) ;
#16325 = B_SPLINE_CURVE_WITH_KNOTS ( 'NONE', 1,
 ( #18965, #33971 ),
 .UNSPECIFIED., .F., .F.,
 ( 2, 2 ),
 ( 0.000000000000000000, 1.000000000000000000 ),
 .UNSPECIFIED. ) ;
#16326 = CARTESIAN_POINT ( 'NONE',  ( -14.51911023200684703, -18.48675360735851925, 52.02966884056656482 ) ) ;
#16327 = ORIENTED_EDGE ( 'NONE', *, *, #35573, .F. ) ;
#16328 = ORIENTED_EDGE ( 'NONE', *, *, #38164, .T. ) ;
#16329 = CARTESIAN_POINT ( 'NONE',  ( -22.97409385541304516, -6.859212275519751323, 50.50378509014259265 ) ) ;
#16330 = EDGE_CURVE ( 'NONE', #46532, #34511, #36872, .T. ) ;
#16331 = B_SPLINE_CURVE_WITH_KNOTS ( 'NONE', 3,
 ( #1520, #12606, #42664, #8927, #16529, #31566, #35723, #40168, #35965, #27865 ),
 .UNSPECIFIED., .F., .F.,
 ( 4, 2, 2, 2, 4 ),
 ( 0.6272669072782128818, 0.7522669073001225781, 0.8772669073220322744, 1.002266907343941860, 1.127266907365851667 ),
 .UNSPECIFIED. ) ;
#16332 = CARTESIAN_POINT ( 'NONE',  ( -18.78767905735283605, -20.13749289187802916, 53.49899999999994549 ) ) ;
#16333 = EDGE_CURVE ( 'NONE', #10419, #22869, #34477, .T. ) ;
#16334 = VECTOR ( 'NONE', #18045, 999.9999999999998863 ) ;
#16335 = CARTESIAN_POINT ( 'NONE',  ( -15.29626560849200878, -8.084834557582363246, 73.96496852212565898 ) ) ;
#16336 =( BOUNDED_SURFACE ( )  B_SPLINE_SURFACE ( 3, 1, ( 
 ( #35034, #31113 ),
 ( #3869, #44752 ),
 ( #835, #4774 ),
 ( #27661, #41045 ),
 ( #42693, #11251 ),
 ( #1302, #33887 ),
 ( #19798, #3609 ) ),
 .UNSPECIFIED., .T., .F., .F. ) 
 B_SPLINE_SURFACE_WITH_KNOTS ( ( 4, 3, 4 ),
 ( 2, 2 ),
 ( 0.000000000000000000, 0.5000000000000000000, 1.000000000000000000 ),
 ( 0.000000000000000000, 1.000000000000000000 ),
 .UNSPECIFIED. ) 
 GEOMETRIC_REPRESENTATION_ITEM ( )  RATIONAL_B_SPLINE_SURFACE ( (
 ( 1.000000000000000000, 1.000000000000000000),
 ( 0.3333333333333335369, 0.3333333333333330373),
 ( 0.3333333333333335369, 0.3333333333333330373),
 ( 1.000000000000000000, 1.000000000000000000),
 ( 0.3333333333333333703, 0.3333333333333333703),
 ( 0.3333333333333333703, 0.3333333333333333703),
 ( 1.000000000000000000, 1.000000000000000000) ) ) 
 REPRESENTATION_ITEM ( '' )  SURFACE ( )  );
#16337 = AXIS2_PLACEMENT_3D ( 'NONE', #4511, #23733, #41947 ) ;
#16338 = AXIS2_PLACEMENT_3D ( 'NONE', #22428, #3462, #18471 ) ;
#16339 = DIRECTION ( 'NONE',  ( 0.000000000000000000, -1.912410701131276611E-32, -1.000000000000000000 ) ) ;
#16340 = CARTESIAN_POINT ( 'NONE',  ( -24.31537953241868522, -17.64020703937282519, 66.06640318968284475 ) ) ;
#16341 = VERTEX_POINT ( 'NONE', #35090 ) ;
#16343 = CARTESIAN_POINT ( 'NONE',  ( -13.97837889017616320, -8.203094814523453238, 74.38609903144701718 ) ) ;
#16342 = B_SPLINE_CURVE_WITH_KNOTS ( 'NONE', 1,
 ( #20097, #12462 ),
 .UNSPECIFIED., .F., .F.,
 ( 2, 2 ),
 ( 0.000000000000000000, 1.000000000000000000 ),
 .UNSPECIFIED. ) ;
#16344 = CARTESIAN_POINT ( 'NONE',  ( -24.00901317767524290, -17.32824147414624960, 69.42811846502259243 ) ) ;
#16345 = EDGE_LOOP ( 'NONE', ( #3404, #32388 ) ) ;
#16346 = CARTESIAN_POINT ( 'NONE',  ( -21.20679145237652108, -20.70065047275357273, 72.75276402661107511 ) ) ;
#16347 = EDGE_CURVE ( 'NONE', #33723, #16869, #16380, .T. ) ;
#16348 = VECTOR ( 'NONE', #5349, 1000.000000000000114 ) ;
#16349 = CARTESIAN_POINT ( 'NONE',  ( -36.42409385541304800, -8.109206544743658540, 50.50000000000030553 ) ) ;
#16350 = ADVANCED_FACE ( 'NONE', ( #46678 ), #42980, .T. ) ;
#16351 =( BOUNDED_CURVE ( )  B_SPLINE_CURVE ( 3, ( #22760, #37752, #19051, #31103 ),
 .UNSPECIFIED., .F., .F. ) 
 B_SPLINE_CURVE_WITH_KNOTS ( ( 4, 4 ),
 ( 0.000000000000000000, 0.4074455897393624015 ),
 .UNSPECIFIED. ) 
 CURVE ( )  GEOMETRIC_REPRESENTATION_ITEM ( )  RATIONAL_B_SPLINE_CURVE ( ( 1.000000000000000000, 0.4567392136813347436, 0.3561768502900313216, 0.6983129098260898449 ) ) 
 REPRESENTATION_ITEM ( '' )  );
#16352 = B_SPLINE_CURVE_WITH_KNOTS ( 'NONE', 3,
 ( #27169, #3793, #12148, #41707, #4765, #19790, #33811, #7993, #109, #23009 ),
 .UNSPECIFIED., .F., .F.,
 ( 4, 2, 2, 2, 4 ),
 ( 0.000000000000000000, 0.2500000000000000000, 0.5000000000000000000, 0.7500000000000000000, 1.000000000000000000 ),
 .UNSPECIFIED. ) ;
#16353 = VERTEX_POINT ( 'NONE', #38547 ) ;
#16354 = CARTESIAN_POINT ( 'NONE',  ( -13.97409385541301496, -6.859212275519754876, 50.50378509014287687 ) ) ;
#16355 = CARTESIAN_POINT ( 'NONE',  ( -9.974039711714500100, -14.85049230159630618, 74.93745556479784398 ) ) ;
#16356 = EDGE_CURVE ( 'NONE', #25757, #46361, #8475, .T. ) ;
#16358 = EDGE_CURVE ( 'NONE', #16476, #45570, #28922, .T. ) ;
#16357 = EDGE_LOOP ( 'NONE', ( #17924, #1070, #29299, #46668 ) ) ;
#16359 = FACE_OUTER_BOUND ( 'NONE', #48026, .T. ) ;
#16360 = CARTESIAN_POINT ( 'NONE',  ( -16.97946044980448121, -21.84517136462328324, 72.31543221430108304 ) ) ;
#16361 = CARTESIAN_POINT ( 'NONE',  ( -10.35423477582964225, -12.45965686662758110, 60.90579408580234855 ) ) ;
#16362 = CARTESIAN_POINT ( 'NONE',  ( -11.53247254227971652, -18.68106628708273931, 65.04707076447483871 ) ) ;
#16363 = ORIENTED_EDGE ( 'NONE', *, *, #30362, .T. ) ;
#16364 = CARTESIAN_POINT ( 'NONE',  ( -18.84068548446033731, -21.72355622379298978, 72.44077832767429470 ) ) ;
#16365 = FACE_OUTER_BOUND ( 'NONE', #6150, .T. ) ;
#16366 = CARTESIAN_POINT ( 'NONE',  ( -23.48344415125163565, -18.41350569598871090, 73.04896097104848707 ) ) ;
#16367 = PRODUCT_CONTEXT ( 'NONE', #44189, 'mechanical' ) ;
#16368 = CARTESIAN_POINT ( 'NONE',  ( -50.42609385541305755, -14.90920654474425433, 71.98235294117645822 ) ) ;
#16369 = CARTESIAN_POINT ( 'NONE',  ( -14.22253886256124389, -8.524026329579788452, 67.46795094879617238 ) ) ;
#16370 = CIRCLE ( 'NONE', #17126, 5.249999999999998224 ) ;
#16371 = DIRECTION ( 'NONE',  ( 2.866981220435666553E-17, -1.000000000000000000, -1.190614954331866791E-16 ) ) ;
#16372 = EDGE_LOOP ( 'NONE', ( #6384, #40578 ) ) ;
#16373 = DIRECTION ( 'NONE',  ( 0.9999889394985580493, 0.004703284017506803583, -7.734398264755851970E-09 ) ) ;
#16374 = ORIENTED_EDGE ( 'NONE', *, *, #10445, .F. ) ;
#16375 = AXIS2_PLACEMENT_3D ( 'NONE', #48481, #32962, #10351 ) ;
#16376 = CARTESIAN_POINT ( 'NONE',  ( -11.37338168604670408, -19.15691247995520996, 71.87341272242258583 ) ) ;
#16377 = CARTESIAN_POINT ( 'NONE',  ( -11.99468485875942925, -10.30643380866937697, 64.23734308384325686 ) ) ;
#16378 = EDGE_LOOP ( 'NONE', ( #22366, #28883, #3320, #46148, #23890 ) ) ;
#16379 = CARTESIAN_POINT ( 'NONE',  ( 18.57590614458695200, 2.144561833755798563, 49.27104351578929453 ) ) ;
#16380 = CIRCLE ( 'NONE', #14000, 4.686499999999998778 ) ;
#16381 = VECTOR ( 'NONE', #12441, 1000.000000000000000 ) ;
#16382 = CARTESIAN_POINT ( 'NONE',  ( -20.37299750454370439, -8.405577324698720432, 66.78104082189589974 ) ) ;
#16383 = VERTEX_POINT ( 'NONE', #24993 ) ;
#16384 = EDGE_CURVE ( 'NONE', #24660, #8287, #28426, .T. ) ;
#16385 = ORIENTED_EDGE ( 'NONE', *, *, #8880, .F. ) ;
#16386 = ORIENTED_EDGE ( 'NONE', *, *, #17312, .T. ) ;
#16387 = FACE_OUTER_BOUND ( 'NONE', #33611, .T. ) ;
#16388 = AXIS2_PLACEMENT_3D ( 'NONE', #3095, #22306, #18103 ) ;
#16389 = CARTESIAN_POINT ( 'NONE',  ( -24.72409385541305582, -14.80920654474414810, 61.02352941176469869 ) ) ;
#16390 = CARTESIAN_POINT ( 'NONE',  ( -14.54749350918766204, -8.372447261038935551, 64.07506791522041567 ) ) ;
#16391 = CARTESIAN_POINT ( 'NONE',  ( -21.36284794767689377, -21.13297080501056513, 69.16954792666395235 ) ) ;
#16392 = CARTESIAN_POINT ( 'NONE',  ( -13.40431825323822146, -9.078389689080667679, 60.72484859302592497 ) ) ;
#16393 = EDGE_LOOP ( 'NONE', ( #8201, #14413, #2416, #10846 ) ) ;
#16394 = ORIENTED_EDGE ( 'NONE', *, *, #41055, .T. ) ;
#16395 = B_SPLINE_CURVE_WITH_KNOTS ( 'NONE', 1,
 ( #45037, #19576 ),
 .UNSPECIFIED., .F., .F.,
 ( 2, 2 ),
 ( 0.000000000000000000, 1.000000000000000000 ),
 .UNSPECIFIED. ) ;
#16396 = CARTESIAN_POINT ( 'NONE',  ( -24.72409385541305582, -14.80920654474422271, 68.96470588235293064 ) ) ;
#16397 = CARTESIAN_POINT ( 'NONE',  ( -22.52619951119469022, -19.67884242972143483, 69.05929390617204433 ) ) ;
#16398 = CARTESIAN_POINT ( 'NONE',  ( -24.87417962317557496, -14.80849170857717567, 59.42795673386487465 ) ) ;
#16399 = LINE ( 'NONE', #31428, #16581 ) ;
#16400 = CARTESIAN_POINT ( 'NONE',  ( -23.00534385650551528, -8.801233750844183135, 48.81488406609782515 ) ) ;
#16401 = VERTEX_POINT ( 'NONE', #35814 ) ;
#16402 = CARTESIAN_POINT ( 'NONE',  ( -14.77786946956392278, -21.77340987454994092, 61.83589227476007721 ) ) ;
#16403 = CARTESIAN_POINT ( 'NONE',  ( -12.15470796376391682, -20.07677110164151557, 61.51023378490003068 ) ) ;
#16404 = AXIS2_PLACEMENT_3D ( 'NONE', #11180, #3788, #3042 ) ;
#16405 = CARTESIAN_POINT ( 'NONE',  ( -12.48641670427285355, -19.77161270282481098, 65.15058277296205347 ) ) ;
#16406 = VECTOR ( 'NONE', #15903, 1000.000000000000000 ) ;
#16407 = VERTEX_POINT ( 'NONE', #2340 ) ;
#16408 = CARTESIAN_POINT ( 'NONE',  ( -20.78034385541293716, -9.360768649639700456, 51.01397948905896840 ) ) ;
#16409 = AXIS2_PLACEMENT_3D ( 'NONE', #38171, #15510, #42131 ) ;
#16410 = CARTESIAN_POINT ( 'NONE',  ( -22.89702288877819214, -9.753446293288515534, 73.66816357947271854 ) ) ;
#16411 = CARTESIAN_POINT ( 'NONE',  ( -50.42409385541304800, -15.80920654474410725, 74.99999999999998579 ) ) ;
#16412 = ADVANCED_FACE ( 'NONE', ( #20814 ), #2584, .F. ) ;
#16413 = ADVANCED_FACE ( 'NONE', ( #10466 ), #28204, .T. ) ;
#16414 = CARTESIAN_POINT ( 'NONE',  ( -12.20316607747752613, -9.493609027659992705, 57.27590782196710251 ) ) ;
#16415 = VERTEX_POINT ( 'NONE', #6031 ) ;
#16416 = AXIS2_PLACEMENT_3D ( 'NONE', #47800, #2737, #40645 ) ;
#16417 = CARTESIAN_POINT ( 'NONE',  ( -22.91699352949043700, -19.14904340809635741, 59.16794112173154474 ) ) ;
#16418 = DIRECTION ( 'NONE',  ( -0.8665025800563552760, 0.2217504876109172018, -0.4472135954999578722 ) ) ;
#16419 = VERTEX_POINT ( 'NONE', #21776 ) ;
#16420 = CARTESIAN_POINT ( 'NONE',  ( -10.01424894596331505, -14.03598936870067782, 61.17467227907766869 ) ) ;
#16421 = ORIENTED_EDGE ( 'NONE', *, *, #5511, .T. ) ;
#16422 = CARTESIAN_POINT ( 'NONE',  ( -18.72681101482837818, -7.880611649715417499, 70.37068030201731972 ) ) ;
#16423 = EDGE_CURVE ( 'NONE', #42703, #45668, #37226, .T. ) ;
#16424 = EDGE_CURVE ( 'NONE', #38066, #36768, #39763, .T. ) ;
#16425 = CARTESIAN_POINT ( 'NONE',  ( -14.62647943160224528, -7.904425104641775945, 60.41972663192098025 ) ) ;
#16426 = VERTEX_POINT ( 'NONE', #29169 ) ;
#16427 = CARTESIAN_POINT ( 'NONE',  ( -17.42409385541299471, -14.80920654474435594, 52.02966884056656482 ) ) ;
#16428 = CARTESIAN_POINT ( 'NONE',  ( -10.67632725396948956, -12.73975884439864359, 57.48424594490033002 ) ) ;
#16429 = DIRECTION ( 'NONE',  ( -0.9729319276368275649, -0.2310918955413239495, 6.827553174175006206E-08 ) ) ;
#16430 = CARTESIAN_POINT ( 'NONE',  ( -45.92409385541306932, -16.70920654474410938, 70.87000000000000455 ) ) ;
#16431 = ORIENTED_EDGE ( 'NONE', *, *, #46385, .F. ) ;
#16432 = CYLINDRICAL_SURFACE ( 'NONE', #15804, 0.1499999999999971079 ) ;
#16433 = CARTESIAN_POINT ( 'NONE',  ( -20.50876352152089765, -19.05741946913900620, 49.52966884056656482 ) ) ;
#16434 = CARTESIAN_POINT ( 'NONE',  ( -10.08080428754885105, -16.06609343925254763, 68.23413777636764621 ) ) ;
#16435 = ORIENTED_EDGE ( 'NONE', *, *, #12216, .F. ) ;
#16436 = CARTESIAN_POINT ( 'NONE',  ( -17.42409385541299471, -14.80920654474435771, 49.52966884056655772 ) ) ;
#16437 = CARTESIAN_POINT ( 'NONE',  ( -15.56465948913147557, -7.543361525925789124, 47.99999999999994316 ) ) ;
#16438 = ADVANCED_FACE ( 'NONE', ( #6282 ), #13879, .F. ) ;
#16439 = ORIENTED_EDGE ( 'NONE', *, *, #37788, .T. ) ;
#16440 = ORIENTED_EDGE ( 'NONE', *, *, #43855, .T. ) ;
#16441 = CARTESIAN_POINT ( 'NONE',  ( -23.89460186926044472, -11.99007647016461320, 63.09651074612323640 ) ) ;
#16442 = CARTESIAN_POINT ( 'NONE',  ( -12.95699726224880699, -8.846094125884357950, 64.02291131566488502 ) ) ;
#16444 = CARTESIAN_POINT ( 'NONE',  ( -21.33159362617910659, -4.962723823544877177, 53.49999999999995026 ) ) ;
#16443 = AXIS2_PLACEMENT_3D ( 'NONE', #20274, #14905, #1553 ) ;
#16445 = CARTESIAN_POINT ( 'NONE',  ( -19.88034385650552238, -6.424090610841174609, 49.80797279389977916 ) ) ;
#16446 = DIRECTION ( 'NONE',  ( -0.1240347345892086062, 1.145860353393066553E-16, -0.9922778767136676281 ) ) ;
#16447 = CARTESIAN_POINT ( 'NONE',  ( -23.80941655268207668, -18.64734661885979961, 72.80722282987319716 ) ) ;
#16448 = FACE_OUTER_BOUND ( 'NONE', #45108, .T. ) ;
#16449 = AXIS2_PLACEMENT_3D ( 'NONE', #14236, #21179, #40593 ) ;
#16450 = CIRCLE ( 'NONE', #21981, 2.000000000000001776 ) ;
#16451 = CARTESIAN_POINT ( 'NONE',  ( -10.82867469351122836, -11.34449526142513598, 67.73369307302053244 ) ) ;
#16452 = ORIENTED_EDGE ( 'NONE', *, *, #26631, .T. ) ;
#16453 = EDGE_LOOP ( 'NONE', ( #29588, #6058, #20342, #14875 ) ) ;
#16454 = B_SPLINE_CURVE_WITH_KNOTS ( 'NONE', 3,
 ( #37836, #38070, #14659, #19365, #26275, #34373, #661, #15661, #42026, #30716 ),
 .UNSPECIFIED., .F., .F.,
 ( 4, 2, 2, 2, 4 ),
 ( 0.000000000000000000, 0.2500000000000000000, 0.5000000000000000000, 0.7500000000000000000, 1.000000000000000000 ),
 .UNSPECIFIED. ) ;
#16455 = CARTESIAN_POINT ( 'NONE',  ( -10.99586753834015695, -11.04334891231907534, 60.86381058728009208 ) ) ;
#16456 = CARTESIAN_POINT ( 'NONE',  ( -22.01346526549441407, -20.09489739794641849, 58.99116211847115920 ) ) ;
#16457 = CARTESIAN_POINT ( 'NONE',  ( -22.45398798615017455, -19.67764645536353996, 72.94400540998888971 ) ) ;
#16458 = DIRECTION ( 'NONE',  ( 2.723496474639940985E-06, 1.584719855340916648E-07, 0.9999999999962787545 ) ) ;
#16459 = ORIENTED_EDGE ( 'NONE', *, *, #26182, .T. ) ;
#16460 = DIRECTION ( 'NONE',  ( 1.224646799147353207E-16, 1.000000000000000000, -1.912410701131276611E-32 ) ) ;
#16461 = CARTESIAN_POINT ( 'NONE',  ( -22.06352460594304787, -8.980016202103444201, 63.37649054182217867 ) ) ;
#16462 =( BOUNDED_CURVE ( )  B_SPLINE_CURVE ( 3, ( #19357, #41046, #34364, #45244 ),
 .UNSPECIFIED., .F., .F. ) 
 B_SPLINE_CURVE_WITH_KNOTS ( ( 4, 4 ),
 ( 0.4074455897393636783, 0.5000000000000000000 ),
 .UNSPECIFIED. ) 
 CURVE ( )  GEOMETRIC_REPRESENTATION_ITEM ( )  RATIONAL_B_SPLINE_CURVE ( ( 0.6983129098260917322, 0.7760317562606919850, 0.8765941196519932976, 0.9999999999999918954 ) ) 
 REPRESENTATION_ITEM ( '' )  );
#16463 = VERTEX_POINT ( 'NONE', #47411 ) ;
#16464 = CARTESIAN_POINT ( 'NONE',  ( -13.02585106727260822, -13.15662797718154309, 49.52966884056655772 ) ) ;
#16465 = CARTESIAN_POINT ( 'NONE',  ( -24.72409385541305582, -14.80920654474418896, 65.94705882352940307 ) ) ;
#16466 = EDGE_CURVE ( 'NONE', #22481, #2842, #11747, .T. ) ;
#16467 = VERTEX_POINT ( 'NONE', #40262 ) ;
#16468 = AXIS2_PLACEMENT_3D ( 'NONE', #39446, #9415, #13078 ) ;
#16469 = CARTESIAN_POINT ( 'NONE',  ( -22.68646480449111635, -20.08284195570847430, 69.35913425646373298 ) ) ;
#16470 = CARTESIAN_POINT ( 'NONE',  ( -13.85393748347032528, -8.270264590973253505, 74.38449983516251507 ) ) ;
#16471 =( BOUNDED_CURVE ( )  B_SPLINE_CURVE ( 3, ( #34176, #22626, #34414, #45056 ),
 .UNSPECIFIED., .F., .F. ) 
 B_SPLINE_CURVE_WITH_KNOTS ( ( 4, 4 ),
 ( 0.5000000000000000000, 0.9074455897393638448 ),
 .UNSPECIFIED. ) 
 CURVE ( )  GEOMETRIC_REPRESENTATION_ITEM ( )  RATIONAL_B_SPLINE_CURVE ( ( 0.9999999999999754641, 0.4567392136813280268, 0.3561768502900458655, 0.6983129098261023904 ) ) 
 REPRESENTATION_ITEM ( '' )  );
#16472 = ORIENTED_EDGE ( 'NONE', *, *, #27278, .F. ) ;
#16473 =( BOUNDED_CURVE ( )  B_SPLINE_CURVE ( 3, ( #4424, #34454, #24119, #35184 ),
 .UNSPECIFIED., .F., .F. ) 
 B_SPLINE_CURVE_WITH_KNOTS ( ( 4, 4 ),
 ( 0.9074455897393645110, 1.000000000000000000 ),
 .UNSPECIFIED. ) 
 CURVE ( )  GEOMETRIC_REPRESENTATION_ITEM ( )  RATIONAL_B_SPLINE_CURVE ( ( 0.6983129098260982826, 0.7760317562607027542, 0.8765941196520032896, 1.000000000000000000 ) ) 
 REPRESENTATION_ITEM ( '' )  );
#16474 = CARTESIAN_POINT ( 'NONE',  ( -10.49080411414803926, -13.84192971499166269, 57.46441715484542812 ) ) ;
#16475 = VECTOR ( 'NONE', #28265, 999.9999999999998863 ) ;
#16476 = VERTEX_POINT ( 'NONE', #17347 ) ;
#16477 = ADVANCED_FACE ( 'NONE', ( #6764 ), #11685, .T. ) ;
#16478 = CARTESIAN_POINT ( 'NONE',  ( -16.87409385759798752, -6.859212275519751323, 50.50378509014259265 ) ) ;
#16479 = B_SPLINE_CURVE_WITH_KNOTS ( 'NONE', 1,
 ( #31338, #42186 ),
 .UNSPECIFIED., .F., .F.,
 ( 2, 2 ),
 ( 0.000000000000000000, 1.000000000000000000 ),
 .UNSPECIFIED. ) ;
#16480 = CARTESIAN_POINT ( 'NONE',  ( -18.67529344402863956, -22.15414776727839907, 72.39855560065855400 ) ) ;
#16481 = ORIENTED_EDGE ( 'NONE', *, *, #41189, .F. ) ;
#16482 = CARTESIAN_POINT ( 'NONE',  ( -14.27319502748954783, -8.558459675072437989, 70.72957628730870283 ) ) ;
#16483 = CARTESIAN_POINT ( 'NONE',  ( -13.04244981547684823, -8.783951787904593189, 64.05946526178860267 ) ) ;
#16484 = EDGE_CURVE ( 'NONE', #33892, #16133, #21524, .T. ) ;
#16485 = CARTESIAN_POINT ( 'NONE',  ( -16.59284385650551741, -7.406986770994972602, 48.81910596585309747 ) ) ;
#16486 = EDGE_LOOP ( 'NONE', ( #27549, #3612, #14707, #42929 ) ) ;
#16487 = CARTESIAN_POINT ( 'NONE',  ( -11.93102662126159785, -10.47028825497329585, 70.96893105764984000 ) ) ;
#16488 = AXIS2_PLACEMENT_3D ( 'NONE', #34681, #11802, #45301 ) ;
#16489 = EDGE_CURVE ( 'NONE', #17121, #10137, #48396, .T. ) ;
#16490 = CARTESIAN_POINT ( 'NONE',  ( -24.10114582721934084, -12.70328895263707913, 73.47055430460139291 ) ) ;
#16491 = CARTESIAN_POINT ( 'NONE',  ( -14.80056043599933524, -21.78207186541723317, 61.82095768364339960 ) ) ;
#16492 = EDGE_LOOP ( 'NONE', ( #32620, #12773 ) ) ;
#16493 = CARTESIAN_POINT ( 'NONE',  ( -16.13712438557350737, -7.928469192395482423, 60.27316438348749017 ) ) ;
#16494 =( BOUNDED_CURVE ( )  B_SPLINE_CURVE ( 3, ( #20982, #18729, #25884, #36943 ),
 .UNSPECIFIED., .F., .F. ) 
 B_SPLINE_CURVE_WITH_KNOTS ( ( 4, 4 ),
 ( 4.712388980384690562, 4.921828490624010399 ),
 .UNSPECIFIED. ) 
 CURVE ( )  GEOMETRIC_REPRESENTATION_ITEM ( )  RATIONAL_B_SPLINE_CURVE ( ( 1.000000000000000000, 0.9963479302455154896, 0.9963479302455154896, 1.000000000000000000 ) ) 
 REPRESENTATION_ITEM ( '' )  );
#16495 = FACE_OUTER_BOUND ( 'NONE', #17849, .T. ) ;
#16496 = CARTESIAN_POINT ( 'NONE',  ( -13.17588093101833557, -17.89387621085224467, 52.02966884056656482 ) ) ;
#16497 = FACE_OUTER_BOUND ( 'NONE', #4175, .T. ) ;
#16498 = CARTESIAN_POINT ( 'NONE',  ( -41.42703503188364778, -14.80920654474424225, 70.97647058823527288 ) ) ;
#16499 = VERTEX_POINT ( 'NONE', #11193 ) ;
#16500 = ORIENTED_EDGE ( 'NONE', *, *, #24197, .T. ) ;
#16501 = DIRECTION ( 'NONE',  ( 0.4433615477241707459, -0.8963428685495451465, 2.661652803430218851E-08 ) ) ;
#16502 = CARTESIAN_POINT ( 'NONE',  ( -21.48252188606478086, -21.05763224395268196, 69.16794793541382091 ) ) ;
#16503 = ORIENTED_EDGE ( 'NONE', *, *, #8626, .T. ) ;
#16504 = B_SPLINE_CURVE_WITH_KNOTS ( 'NONE', 3,
 ( #5824, #47181, #24055, #43499, #6048, #43255, #20836, #28702, #25015, #39051 ),
 .UNSPECIFIED., .F., .F.,
 ( 4, 2, 2, 2, 4 ),
 ( 0.000000000000000000, 0.2500000000000000000, 0.5000000000000000000, 0.7500000000000000000, 1.000000000000000000 ),
 .UNSPECIFIED. ) ;
#16505 = CARTESIAN_POINT ( 'NONE',  ( -16.07630405233268434, -7.886179812623181462, 67.55496168274575552 ) ) ;
#16506 = CARTESIAN_POINT ( 'NONE',  ( -21.81985589881223930, -9.292801929985119003, 59.92991148151821079 ) ) ;
#16507 = CARTESIAN_POINT ( 'NONE',  ( -10.29385348138020539, -12.64970417265235803, 64.38340698725603772 ) ) ;
#16508 = CARTESIAN_POINT ( 'NONE',  ( -13.07753640729841571, -8.758436312614517050, 64.03229666249436036 ) ) ;
#16509 = CARTESIAN_POINT ( 'NONE',  ( 18.57590614458706924, 1.890747609047612077, 50.53028072113853142 ) ) ;
#16510 = CARTESIAN_POINT ( 'NONE',  ( -12.22244147144377280, -10.12480163234519281, 60.63206217599131520 ) ) ;
#16511 = ORIENTED_EDGE ( 'NONE', *, *, #4427, .F. ) ;
#16512 = CARTESIAN_POINT ( 'NONE',  ( -22.73618463404748624, -20.03370227938794912, 69.28762739622011679 ) ) ;
#16513 = FACE_OUTER_BOUND ( 'NONE', #18247, .T. ) ;
#16514 = CARTESIAN_POINT ( 'NONE',  ( -10.45859239952313224, -15.89938452881993847, 64.79299464097340433 ) ) ;
#16515 = AXIS2_PLACEMENT_3D ( 'NONE', #48584, #14817, #8697 ) ;
#16516 = CARTESIAN_POINT ( 'NONE',  ( -20.92409385541305511, -10.10920654474410618, 81.49999999999998579 ) ) ;
#16517 = LINE ( 'NONE', #31551, #160 ) ;
#16518 = VERTEX_POINT ( 'NONE', #33561 ) ;
#16519 = ORIENTED_EDGE ( 'NONE', *, *, #7099, .F. ) ;
#16520 = ORIENTED_EDGE ( 'NONE', *, *, #43911, .F. ) ;
#16521 = CARTESIAN_POINT ( 'NONE',  ( -17.56877512014188625, -7.360533253644350182, 63.59411120999686062 ) ) ;
#16522 = DIRECTION ( 'NONE',  ( -5.731567514496413899E-31, -1.020425574103664789E-16, -1.000000000000000000 ) ) ;
#16523 = VECTOR ( 'NONE', #24722, 1000.000000000000114 ) ;
#16524 = EDGE_CURVE ( 'NONE', #10223, #36492, #43532, .T. ) ;
#16525 = ORIENTED_EDGE ( 'NONE', *, *, #9153, .F. ) ;
#16526 = CARTESIAN_POINT ( 'NONE',  ( -21.89953879547803695, -8.853196296446007807, 66.70504049802050872 ) ) ;
#16527 = CARTESIAN_POINT ( 'NONE',  ( -10.37795889460693033, -14.56696403379599225, 68.14328054657653411 ) ) ;
#16528 = ORIENTED_EDGE ( 'NONE', *, *, #27553, .T. ) ;
#16529 = CARTESIAN_POINT ( 'NONE',  ( -10.63768371389235767, -17.88312332652141023, 71.68905463271586598 ) ) ;
#16530 = CARTESIAN_POINT ( 'NONE',  ( -19.30861700655685098, -22.01699669475148724, 58.78153328179137560 ) ) ;
#16531 = EDGE_LOOP ( 'NONE', ( #21461, #11898, #29779, #47292 ) ) ;
#16532 = LINE ( 'NONE', #12610, #17848 ) ;
#16533 = CARTESIAN_POINT ( 'NONE',  ( -10.13784000599894597, -13.25541019000276499, 74.79322239981686948 ) ) ;
#16534 = ORIENTED_EDGE ( 'NONE', *, *, #10495, .F. ) ;
#16535 = CARTESIAN_POINT ( 'NONE',  ( -13.40763370604777371, -17.22402126197653160, 49.52966884056655772 ) ) ;
#16536 = CARTESIAN_POINT ( 'NONE',  ( -22.47873160378920687, -20.28232442305464645, 65.82704820931039080 ) ) ;
#16537 = CARTESIAN_POINT ( 'NONE',  ( -21.03862266567373851, -20.86632007393060917, 62.32291251243861296 ) ) ;
#16538 = ORIENTED_EDGE ( 'NONE', *, *, #9009, .T. ) ;
#16539 = CARTESIAN_POINT ( 'NONE',  ( -24.23941684483994408, -17.81830337043964718, 62.58086817458297446 ) ) ;
#16540 = CARTESIAN_POINT ( 'NONE',  ( -24.72409385541305582, -14.80920654474426357, 72.08823529411763786 ) ) ;
#16541 = EDGE_CURVE ( 'NONE', #7654, #31760, #43813, .T. ) ;
#16542 = CARTESIAN_POINT ( 'NONE',  ( -19.11145557798581152, -7.964112677450091660, 63.73089235102099792 ) ) ;
#16543 = ADVANCED_FACE ( 'NONE', ( #22770 ), #25712, .T. ) ;
#16544 = CARTESIAN_POINT ( 'NONE',  ( -14.72744631621160494, -8.295007313424175521, 60.60524229057013201 ) ) ;
#16545 = CARTESIAN_POINT ( 'NONE',  ( -22.23733836534369601, -19.96043719841513564, 65.85421731380807842 ) ) ;
#16546 = CARTESIAN_POINT ( 'NONE',  ( -20.57444639489040483, -21.06071912686655168, 58.92858597573613366 ) ) ;
#16547 = ORIENTED_EDGE ( 'NONE', *, *, #47622, .F. ) ;
#16548 = VECTOR ( 'NONE', #41063, 1000.000000000000000 ) ;
#16549 = DIRECTION ( 'NONE',  ( -0.9687793358424819923, 0.2479245821708680464, 0.000000000000000000 ) ) ;
#16550 = CARTESIAN_POINT ( 'NONE',  ( -16.58751243259469277, -21.80939447449397051, 65.37564390318223673 ) ) ;
#16551 = CARTESIAN_POINT ( 'NONE',  ( -24.86479638606408571, -14.43697995806947176, 66.38303926562055324 ) ) ;
#16552 = CARTESIAN_POINT ( 'NONE',  ( -16.39155882215229099, -21.78318466615559146, 61.90568132352964881 ) ) ;
#16553 = EDGE_CURVE ( 'NONE', #36936, #16629, #30006, .T. ) ;
#16554 = DIRECTION ( 'NONE',  ( 1.000000000000000000, -4.164305804376849172E-17, 1.614929280266638808E-16 ) ) ;
#16555 = CARTESIAN_POINT ( 'NONE',  ( -17.85534385650552025, -7.417179338643134834, 52.18511593390279302 ) ) ;
#16556 = ORIENTED_EDGE ( 'NONE', *, *, #40359, .F. ) ;
#16557 = CARTESIAN_POINT ( 'NONE',  ( -13.99679447977218061, -20.97040113148658591, 71.94079819673058296 ) ) ;
#16558 = DIRECTION ( 'NONE',  ( 2.168404344971008375E-16, 0.000000000000000000, -1.000000000000000000 ) ) ;
#16559 = EDGE_LOOP ( 'NONE', ( #32147, #46280, #10871, #32288, #48414 ) ) ;
#16560 = CARTESIAN_POINT ( 'NONE',  ( -23.36391615787244191, -18.61340847718015823, 66.03209153377542862 ) ) ;
#16561 = CARTESIAN_POINT ( 'NONE',  ( -14.47983125967835960, -7.965589368325148634, 63.90483512601500848 ) ) ;
#16562 = AXIS2_PLACEMENT_3D ( 'NONE', #13954, #36607, #44517 ) ;
#16563 = CARTESIAN_POINT ( 'NONE',  ( -12.74083618280373642, -20.01189185905951007, 68.35159915988243995 ) ) ;
#16564 = CARTESIAN_POINT ( 'NONE',  ( 22.62590614458706639, 1.876874565721113663, 52.48023137145496264 ) ) ;
#16565 = EDGE_CURVE ( 'NONE', #48128, #44170, #19638, .T. ) ;
#16566 = ORIENTED_EDGE ( 'NONE', *, *, #42600, .F. ) ;
#16567 = FACE_OUTER_BOUND ( 'NONE', #32219, .T. ) ;
#16568 = CARTESIAN_POINT ( 'NONE',  ( -13.65684165595416921, -8.849801312179289781, 56.98439896120441261 ) ) ;
#16569 = CARTESIAN_POINT ( 'NONE',  ( -10.51729459156483237, -16.22293329152201480, 71.59750383216309899 ) ) ;
#16570 = ORIENTED_EDGE ( 'NONE', *, *, #40792, .T. ) ;
#16571 = CIRCLE ( 'NONE', #40166, 4.686499999999997890 ) ;
#16572 = FACE_OUTER_BOUND ( 'NONE', #21363, .T. ) ;
#16573 =( BOUNDED_CURVE ( )  B_SPLINE_CURVE ( 3, ( #4387, #14454, #29513, #18415 ),
 .UNSPECIFIED., .F., .F. ) 
 B_SPLINE_CURVE_WITH_KNOTS ( ( 4, 4 ),
 ( 0.9074455897393657322, 1.000000000000000000 ),
 .UNSPECIFIED. ) 
 CURVE ( )  GEOMETRIC_REPRESENTATION_ITEM ( )  RATIONAL_B_SPLINE_CURVE ( ( 0.6983129098260912881, 0.7760317562606967590, 0.8765941196519996259, 1.000000000000000000 ) ) 
 REPRESENTATION_ITEM ( '' )  );
#16574 = CARTESIAN_POINT ( 'NONE',  ( -13.22164718542227035, -8.657617455897696601, 60.63961484927665424 ) ) ;
#16575 = CARTESIAN_POINT ( 'NONE',  ( -17.96636798352247055, -9.322503134287590143, 53.69233794759168887 ) ) ;
#16576 = PLANE ( 'NONE',  #26773 ) ;
#16577 = CARTESIAN_POINT ( 'NONE',  ( -23.08261055559088248, -18.93003034027461950, 62.65406880913197796 ) ) ;
#16578 = EDGE_LOOP ( 'NONE', ( #22325, #47911, #13909, #46855 ) ) ;
#16579 = ORIENTED_EDGE ( 'NONE', *, *, #36329, .F. ) ;
#16580 = CARTESIAN_POINT ( 'NONE',  ( -21.51159385541304303, -8.990409506049200417, 49.61344411288074951 ) ) ;
#16581 = VECTOR ( 'NONE', #2115, 1000.000000000000000 ) ;
#16582 = CARTESIAN_POINT ( 'NONE',  ( -22.97166404482257107, -9.836574275791852173, 70.21189719861501999 ) ) ;
#16583 = AXIS2_PLACEMENT_3D ( 'NONE', #36354, #29225, #21113 ) ;
#16584 = DIRECTION ( 'NONE',  ( -3.071710424422018668E-17, 6.404604876783312462E-16, 1.000000000000000000 ) ) ;
#16585 = ADVANCED_FACE ( 'NONE', ( #48356 ), #7507, .T. ) ;
#16586 = CIRCLE ( 'NONE', #26027, 0.4000000000000011879 ) ;
#16587 = B_SPLINE_CURVE_WITH_KNOTS ( 'NONE', 3,
 ( #8217, #41699, #7985, #4272, #38221, #38473, #16295, #34788, #4505, #20253 ),
 .UNSPECIFIED., .F., .F.,
 ( 4, 2, 2, 2, 4 ),
 ( 0.000000000000000000, 0.2500000000000000000, 0.5000000000000000000, 0.7500000000000000000, 1.000000000000000000 ),
 .UNSPECIFIED. ) ;
#16588 = CARTESIAN_POINT ( 'NONE',  ( -24.72409385541305582, -14.90920654474423124, 69.07058823529411029 ) ) ;
#16589 = CARTESIAN_POINT ( 'NONE',  ( -24.72409385541305582, -14.80920654474416764, 63.93529411764704662 ) ) ;
#16590 = ORIENTED_EDGE ( 'NONE', *, *, #38911, .F. ) ;
#16591 = DIRECTION ( 'NONE',  ( -0.4408917724886824430, -0.07492959997082740409, 0.8944271909999157444 ) ) ;
#16592 = B_SPLINE_CURVE_WITH_KNOTS ( 'NONE', 1,
 ( #47243, #21391 ),
 .UNSPECIFIED., .F., .F.,
 ( 2, 2 ),
 ( 0.000000000000000000, 1.000000000000000000 ),
 .UNSPECIFIED. ) ;
#16593 = CARTESIAN_POINT ( 'NONE',  ( -18.19389323530821301, -22.21941482433020809, 65.53027461949925225 ) ) ;
#16594 = ORIENTED_EDGE ( 'NONE', *, *, #18084, .F. ) ;
#16595 = CARTESIAN_POINT ( 'NONE',  ( -24.14992870231961319, -18.01341063617936911, 59.11883102335588802 ) ) ;
#16596 = EDGE_CURVE ( 'NONE', #45882, #30416, #100, .T. ) ;
#16597 = CARTESIAN_POINT ( 'NONE',  ( -46.33910710821349710, -14.20920654474410760, 70.13000000000000966 ) ) ;
#16598 = ORIENTED_EDGE ( 'NONE', *, *, #15869, .T. ) ;
#16599 = CARTESIAN_POINT ( 'NONE',  ( -6.424093855413058662, -6.859206544744110623, 52.99999999999998579 ) ) ;
#16600 = CARTESIAN_POINT ( 'NONE',  ( -27.42409385541305511, -25.10920654474410441, 78.99999999999998579 ) ) ;
#16601 = ORIENTED_EDGE ( 'NONE', *, *, #20772, .T. ) ;
#16602 = CARTESIAN_POINT ( 'NONE',  ( -17.77920954038207668, -22.25082405446125122, 58.59048702730397196 ) ) ;
#16603 = VECTOR ( 'NONE', #48399, 1000.000000000000000 ) ;
#16604 = EDGE_CURVE ( 'NONE', #46504, #7981, #22265, .T. ) ;
#16605 = CARTESIAN_POINT ( 'NONE',  ( -19.74284385759798965, -7.587656875400192291, 49.25157356644813689 ) ) ;
#16606 = CARTESIAN_POINT ( 'NONE',  ( -20.10190376251898670, -8.341580098330338089, 70.53635029990871885 ) ) ;
#16607 = CARTESIAN_POINT ( 'NONE',  ( -24.70870331492811900, -13.24806755967459537, 59.46293686089323671 ) ) ;
#16608 = ORIENTED_EDGE ( 'NONE', *, *, #6116, .T. ) ;
#16609 = CARTESIAN_POINT ( 'NONE',  ( -18.46649413407774887, -22.18667672369172550, 72.47166315949273496 ) ) ;
#16610 = CARTESIAN_POINT ( 'NONE',  ( -22.24652905638778577, -19.95594847178128362, 62.11950460074248781 ) ) ;
#16611 = CARTESIAN_POINT ( 'NONE',  ( -23.10667289873031649, -18.98809891091294233, 66.12389717179522108 ) ) ;
#16612 = CARTESIAN_POINT ( 'NONE',  ( -10.00761947527410634, -15.51609109068450465, 57.75288224187332276 ) ) ;
#16613 = EDGE_CURVE ( 'NONE', #34949, #28014, #20239, .T. ) ;
#16614 = CARTESIAN_POINT ( 'NONE',  ( -22.09029313690021112, -20.02728107436852767, 62.53439146813792604 ) ) ;
#16615 = FACE_OUTER_BOUND ( 'NONE', #33978, .T. ) ;
#16616 = AXIS2_PLACEMENT_3D ( 'NONE', #40605, #44101, #33446 ) ;
#16617 = CARTESIAN_POINT ( 'NONE',  ( -24.50530043060364349, -7.885727737951715888, 53.49999999999995026 ) ) ;
#16618 = ORIENTED_EDGE ( 'NONE', *, *, #5457, .T. ) ;
#16619 = CARTESIAN_POINT ( 'NONE',  ( -15.47038549838128674, -21.58309193914155344, 72.19575460769013375 ) ) ;
#16620 = EDGE_CURVE ( 'NONE', #10403, #20439, #40820, .T. ) ;
#16621 = ORIENTED_EDGE ( 'NONE', *, *, #14290, .F. ) ;
#16622 = CARTESIAN_POINT ( 'NONE',  ( -11.41497442304007670, -19.21309820834011362, 71.80190602235010999 ) ) ;
#16623 = CARTESIAN_POINT ( 'NONE',  ( -20.81921389985186721, -21.44071754855728784, 58.75979745677555854 ) ) ;
#16624 =( BOUNDED_SURFACE ( )  B_SPLINE_SURFACE ( 3, 1, ( 
 ( #44156, #3985 ),
 ( #22702, #40908 ),
 ( #10873, #25414 ),
 ( #21957, #22205 ),
 ( #36953, #48535 ),
 ( #18245, #17999 ),
 ( #48058, #33254 ) ),
 .UNSPECIFIED., .T., .F., .F. ) 
 B_SPLINE_SURFACE_WITH_KNOTS ( ( 4, 3, 4 ),
 ( 2, 2 ),
 ( 0.000000000000000000, 0.5000000000000000000, 1.000000000000000000 ),
 ( 0.000000000000000000, 1.000000000000000000 ),
 .UNSPECIFIED. ) 
 GEOMETRIC_REPRESENTATION_ITEM ( )  RATIONAL_B_SPLINE_SURFACE ( (
 ( 1.000000000000000000, 1.000000000000000000),
 ( 0.3333333333333335369, 0.3333333333333330373),
 ( 0.3333333333333335369, 0.3333333333333330373),
 ( 1.000000000000000000, 1.000000000000000000),
 ( 0.3333333333333333703, 0.3333333333333333703),
 ( 0.3333333333333333703, 0.3333333333333333703),
 ( 1.000000000000000000, 1.000000000000000000) ) ) 
 REPRESENTATION_ITEM ( '' )  SURFACE ( )  );
#16625 = ORIENTED_EDGE ( 'NONE', *, *, #10435, .F. ) ;
#16626 = LINE ( 'NONE', #36060, #44458 ) ;
#16627 = FACE_BOUND ( 'NONE', #36276, .T. ) ;
#16628 = ORIENTED_EDGE ( 'NONE', *, *, #20874, .F. ) ;
#16629 = VERTEX_POINT ( 'NONE', #27414 ) ;
#16630 = VERTEX_POINT ( 'NONE', #12393 ) ;
#16631 = CARTESIAN_POINT ( 'NONE',  ( -12.85169559483840374, -15.89028456787280952, 52.02966884056656482 ) ) ;
#16632 = VECTOR ( 'NONE', #32109, 1000.000000000000114 ) ;
#16633 = LINE ( 'NONE', #31180, #6691 ) ;
#16634 = DIRECTION ( 'NONE',  ( -3.071710424422018668E-17, 6.404604876783312462E-16, 1.000000000000000000 ) ) ;
#16635 = EDGE_CURVE ( 'NONE', #23522, #44556, #6418, .T. ) ;
#16636 = CARTESIAN_POINT ( 'NONE',  ( -11.97490362423377164, -10.33561459433851404, 67.78424783647008667 ) ) ;
#16637 =( BOUNDED_SURFACE ( )  B_SPLINE_SURFACE ( 3, 1, ( 
 ( #10269, #1224 ),
 ( #31040, #42364 ),
 ( #46054, #25284 ),
 ( #27335, #8637 ),
 ( #27580, #23660 ),
 ( #34956, #16229 ),
 ( #31271, #12558 ) ),
 .UNSPECIFIED., .T., .F., .F. ) 
 B_SPLINE_SURFACE_WITH_KNOTS ( ( 4, 3, 4 ),
 ( 2, 2 ),
 ( 0.000000000000000000, 0.5000000000000000000, 1.000000000000000000 ),
 ( 0.000000000000000000, 1.000000000000000000 ),
 .UNSPECIFIED. ) 
 GEOMETRIC_REPRESENTATION_ITEM ( )  RATIONAL_B_SPLINE_SURFACE ( (
 ( 1.000000000000000000, 1.000000000000000000),
 ( 0.3333333333333335369, 0.3333333333333330373),
 ( 0.3333333333333335369, 0.3333333333333330373),
 ( 1.000000000000000000, 1.000000000000000000),
 ( 0.3333333333333333703, 0.3333333333333333703),
 ( 0.3333333333333333703, 0.3333333333333333703),
 ( 1.000000000000000000, 1.000000000000000000) ) ) 
 REPRESENTATION_ITEM ( '' )  SURFACE ( )  );
#16638 = EDGE_CURVE ( 'NONE', #32429, #15048, #6113, .T. ) ;
#16639 = ORIENTED_EDGE ( 'NONE', *, *, #33306, .T. ) ;
#16640 = EDGE_LOOP ( 'NONE', ( #20738, #8058, #26763, #13072 ) ) ;
#16641 = CARTESIAN_POINT ( 'NONE',  ( -20.30534385650551243, -8.801233750844183135, 48.81488406609782515 ) ) ;
#16642 = ADVANCED_FACE ( 'NONE', ( #4521 ), #30886, .F. ) ;
#16643 = AXIS2_PLACEMENT_3D ( 'NONE', #14824, #18795, #25462 ) ;
#16644 = CARTESIAN_POINT ( 'NONE',  ( -17.42409385541299471, -14.80920654474435594, 52.02966884056656482 ) ) ;
#16645 = DIRECTION ( 'NONE',  ( -0.7700094066334558507, -0.6380325334150235284, 0.000000000000000000 ) ) ;
#16646 = CYLINDRICAL_SURFACE ( 'NONE', #43353, 0.1500000000000063227 ) ;
#16647 = CARTESIAN_POINT ( 'NONE',  ( -21.65534385650552096, -7.417179338643134834, 52.18511593390279302 ) ) ;
#16648 = ORIENTED_EDGE ( 'NONE', *, *, #39002, .T. ) ;
#16649 = AXIS2_PLACEMENT_3D ( 'NONE', #11513, #41304, #29259 ) ;
#16650 = CARTESIAN_POINT ( 'NONE',  ( -23.00381842360518547, -10.58230771189866104, 59.90203429537245228 ) ) ;
#16651 = CARTESIAN_POINT ( 'NONE',  ( -17.42409385541300892, -14.80920654474439324, 53.49899999999994549 ) ) ;
#16652 = VECTOR ( 'NONE', #35230, 1000.000000000000114 ) ;
#16653 = CARTESIAN_POINT ( 'NONE',  ( -24.48565114283276500, -17.18359061586099301, 73.07610194155731165 ) ) ;
#16654 = B_SPLINE_CURVE_WITH_KNOTS ( 'NONE', 3,
 ( #5192, #8648, #42379, #46794, #42860, #35211, #1483, #23671, #38672, #20695 ),
 .UNSPECIFIED., .F., .F.,
 ( 4, 2, 2, 2, 4 ),
 ( 0.6272669072782514066, 0.7522669073001546636, 0.8772669073220578095, 1.002266907343960956, 1.127266907365864324 ),
 .UNSPECIFIED. ) ;
#16655 = VERTEX_POINT ( 'NONE', #45898 ) ;
#16656 = CARTESIAN_POINT ( 'NONE',  ( -17.33262245845742910, -7.759502110702281463, 67.30567542699309058 ) ) ;
#16657 = CARTESIAN_POINT ( 'NONE',  ( -10.98115068093432356, -12.07269720428386961, 74.74943597065113465 ) ) ;
#16658 = FACE_OUTER_BOUND ( 'NONE', #15475, .T. ) ;
#16659 = EDGE_LOOP ( 'NONE', ( #38553, #42660, #24733, #25175, #26859 ) ) ;
#16660 = CARTESIAN_POINT ( 'NONE',  ( -10.57990114081760957, -13.11695186304740979, 71.22300718686658172 ) ) ;
#16661 = CARTESIAN_POINT ( 'NONE',  ( -17.33262245845742910, -7.759502110702281463, 67.30567542699309058 ) ) ;
#16662 = CARTESIAN_POINT ( 'NONE',  ( -11.42760935163198965, -18.42145026959589060, 61.29327518568021560 ) ) ;
#16663 = VERTEX_POINT ( 'NONE', #31604 ) ;
#16664 = CARTESIAN_POINT ( 'NONE',  ( -10.41531639268335496, -14.04517892474411589, 60.93293405735092705 ) ) ;
#16665 = EDGE_LOOP ( 'NONE', ( #36508, #13031 ) ) ;
#16666 = CARTESIAN_POINT ( 'NONE',  ( -40.92409385541305511, -14.80920654474410725, 74.99999999999998579 ) ) ;
#16667 = CARTESIAN_POINT ( 'NONE',  ( -14.59772110827021763, -7.916021557401901276, 60.49713200689404857 ) ) ;
#16669 = EDGE_CURVE ( 'NONE', #18791, #37218, #33120, .T. ) ;
#16668 = ORIENTED_EDGE ( 'NONE', *, *, #34090, .T. ) ;
#16670 = CARTESIAN_POINT ( 'NONE',  ( 18.87590614458706995, 1.904620652374673151, 48.58033007082241994 ) ) ;
#16671 = CARTESIAN_POINT ( 'NONE',  ( -10.40127108354264429, -12.32249413655887871, 57.51352655450988749 ) ) ;
#16672 = CYLINDRICAL_SURFACE ( 'NONE', #48660, 5.000000000000001776 ) ;
#16673 = EDGE_LOOP ( 'NONE', ( #2080, #16150, #869, #36424, #25478 ) ) ;
#16674 = CARTESIAN_POINT ( 'NONE',  ( -10.76763519559319882, -17.13171766695033327, 61.15743118826002700 ) ) ;
#16675 = CARTESIAN_POINT ( 'NONE',  ( -21.24651499925844078, -18.40803921647045982, 50.77966884056655772 ) ) ;
#16676 = CARTESIAN_POINT ( 'NONE',  ( -23.88415217903648724, -17.63235132829416685, 62.77360984996716553 ) ) ;
#16677 = VERTEX_POINT ( 'NONE', #38489 ) ;
#16678 = CARTESIAN_POINT ( 'NONE',  ( -10.39215600595210631, -14.30487551902977827, 64.38803863383273551 ) ) ;
#16679 = CARTESIAN_POINT ( 'NONE',  ( -14.25548580596218429, -11.33998781794830712, 49.52966884056655772 ) ) ;
#16680 = ORIENTED_EDGE ( 'NONE', *, *, #1716, .T. ) ;
#16681 = EDGE_LOOP ( 'NONE', ( #27054, #24149, #21646, #3667 ) ) ;
#16682 = CARTESIAN_POINT ( 'NONE',  ( -14.11063322135152909, -21.03236308526469855, 72.21135587486895702 ) ) ;
#16683 = CARTESIAN_POINT ( 'NONE',  ( -50.42609385541305755, -14.80920654474414810, 61.92352941176469727 ) ) ;
#16684 = LINE ( 'NONE', #43043, #19413 ) ;
#16685 = CARTESIAN_POINT ( 'NONE',  ( -18.64284385650551812, -8.811426318492348031, 52.18089403414751359 ) ) ;
#16686 = CARTESIAN_POINT ( 'NONE',  ( -18.72681101482837818, -7.880611649715417499, 70.37068030201731972 ) ) ;
#16687 = CARTESIAN_POINT ( 'NONE',  ( -17.81160558974999830, -14.71003671187606088, 52.02966884056655061 ) ) ;
#16688 = CARTESIAN_POINT ( 'NONE',  ( -10.40127070788197017, -12.32249518151173895, 57.51352764219546998 ) ) ;
#16689 = ADVANCED_FACE ( 'NONE', ( #589 ), #42694, .T. ) ;
#16690 = CARTESIAN_POINT ( 'NONE',  ( -23.34288328645119037, -19.33377384263253873, 59.06905932422779415 ) ) ;
#16691 = ORIENTED_EDGE ( 'NONE', *, *, #1216, .F. ) ;
#16692 = ORIENTED_EDGE ( 'NONE', *, *, #26456, .T. ) ;
#16693 = CARTESIAN_POINT ( 'NONE',  ( -23.03538909537400770, -9.907469116741831172, 70.19833813022523827 ) ) ;
#16694 = EDGE_CURVE ( 'NONE', #2787, #34596, #40068, .T. ) ;
#16695 = EDGE_CURVE ( 'NONE', #17028, #42512, #46383, .T. ) ;
#16696 = CARTESIAN_POINT ( 'NONE',  ( 0.000000000000000000, 0.000000000000000000, 0.000000000000000000 ) ) ;
#16697 = DIRECTION ( 'NONE',  ( 1.000000000000000000, -4.164305804376849172E-17, 1.614929280266638808E-16 ) ) ;
#16698 = CARTESIAN_POINT ( 'NONE',  ( -19.29727288544221864, -21.61407024248036635, 65.60919142207177401 ) ) ;
#16699 = DIRECTION ( 'NONE',  ( 0.000000000000000000, 0.000000000000000000, 1.000000000000000000 ) ) ;
#16700 = CARTESIAN_POINT ( 'NONE',  ( -41.30129973776600139, -14.90920654474425433, 71.98235294117645822 ) ) ;
#16701 = B_SPLINE_CURVE_WITH_KNOTS ( 'NONE', 3,
 ( #22172, #17720, #47774, #10595, #14013, #6425, #10365, #25604, #21449, #40616 ),
 .UNSPECIFIED., .F., .F.,
 ( 4, 2, 2, 2, 4 ),
 ( 0.000000000000000000, 0.2500000000000000000, 0.5000000000000000000, 0.7500000000000000000, 1.000000000000000000 ),
 .UNSPECIFIED. ) ;
#16702 = ORIENTED_EDGE ( 'NONE', *, *, #47095, .F. ) ;
#16703 = CARTESIAN_POINT ( 'NONE',  ( -22.93812568863854295, -10.41619827269718890, 63.07186016945863827 ) ) ;
#16704 = FILL_AREA_STYLE ('',( #28772 ) ) ;
#16705 = CARTESIAN_POINT ( 'NONE',  ( -22.10219206297270489, -9.524287713326932803, 63.33586711951718229 ) ) ;
#16706 = CARTESIAN_POINT ( 'NONE',  ( -11.05958060454627656, -18.68192940480324182, 61.41677500004188062 ) ) ;
#16707 = VERTEX_POINT ( 'NONE', #5023 ) ;
#16708 = CARTESIAN_POINT ( 'NONE',  ( -22.53655473247544805, -20.22829521909097394, 65.88917159596024931 ) ) ;
#16709 = CARTESIAN_POINT ( 'NONE',  ( -24.39763799706551950, -15.84669482609578317, 69.54779622430707775 ) ) ;
#16710 = ADVANCED_FACE ( 'NONE', ( #1072 ), #13589, .T. ) ;
#16711 = CARTESIAN_POINT ( 'NONE',  ( -10.12326218194131044, -13.32541594658350448, 74.86312942357149325 ) ) ;
#16712 = CARTESIAN_POINT ( 'NONE',  ( -12.83007281553047108, -20.09077549419061626, 71.80653676829817300 ) ) ;
#16713 = CARTESIAN_POINT ( 'NONE',  ( -24.24305685102723018, -16.39138408180526696, 59.42332478927817618 ) ) ;
#16714 = EDGE_LOOP ( 'NONE', ( #32731, #5583, #8523, #5229 ) ) ;
#16715 = CARTESIAN_POINT ( 'NONE',  ( -20.30329177529516116, -7.937872566059631652, 70.41133733428102914 ) ) ;
#16716 = ORIENTED_EDGE ( 'NONE', *, *, #26663, .F. ) ;
#16717 = CARTESIAN_POINT ( 'NONE',  ( -19.24869282864567310, -7.585968669060765279, 63.60902014247216130 ) ) ;
#16718 = CARTESIAN_POINT ( 'NONE',  ( -11.93102524044397938, -10.47028995287008257, 71.26893105764186487 ) ) ;
#16719 = EDGE_LOOP ( 'NONE', ( #44324, #143 ) ) ;
#16720 = CARTESIAN_POINT ( 'NONE',  ( -18.25923033419348940, -22.21300364388852344, 69.00170051292239748 ) ) ;
#16721 = CARTESIAN_POINT ( 'NONE',  ( -18.16784385650552025, -6.428312510596451368, 51.20221977374900035 ) ) ;
#16722 = VERTEX_POINT ( 'NONE', #25183 ) ;
#16723 = CARTESIAN_POINT ( 'NONE',  ( -17.93803645886973541, -7.826487636815978810, 60.19133818497105182 ) ) ;
#16724 = CARTESIAN_POINT ( 'NONE',  ( -14.86477050248655551, -7.812526586475418533, 57.10645908473438226 ) ) ;
#16725 = DIRECTION ( 'NONE',  ( 4.115385489419834812E-17, 0.9999954153791273948, 0.003028072113822188795 ) ) ;
#16726 = VERTEX_POINT ( 'NONE', #28865 ) ;
#16727 = DIRECTION ( 'NONE',  ( -0.7300417127692488961, -0.6834025882427879894, -6.612978995310452690E-09 ) ) ;
#16728 = DIRECTION ( 'NONE',  ( 0.9687793358424817702, -0.2479245821708688791, 0.000000000000000000 ) ) ;
#16729 = LINE ( 'NONE', #43352, #22733 ) ;
#16730 = B_SPLINE_CURVE_WITH_KNOTS ( 'NONE', 3,
 ( #34754, #8188, #27368, #23204, #26401, #22717, #34990, #19983, #31306, #16026 ),
 .UNSPECIFIED., .F., .F.,
 ( 4, 2, 2, 2, 4 ),
 ( 0.000000000000000000, 0.2500000000000000000, 0.5000000000000000000, 0.7500000000000000000, 1.000000000000000000 ),
 .UNSPECIFIED. ) ;
#16731 = DIRECTION ( 'NONE',  ( 0.2573866790907599622, 0.9663084897829604669, 6.714855467380901661E-08 ) ) ;
#16732 = VECTOR ( 'NONE', #23456, 1000.000000000000227 ) ;
#16733 = ORIENTED_EDGE ( 'NONE', *, *, #9103, .T. ) ;
#16734 = ORIENTED_EDGE ( 'NONE', *, *, #38791, .F. ) ;
#16735 = CYLINDRICAL_SURFACE ( 'NONE', #14883, 0.1500000000000045464 ) ;
#16736 = CYLINDRICAL_SURFACE ( 'NONE', #36755, 0.1500000000000002165 ) ;
#16737 = VERTEX_POINT ( 'NONE', #32085 ) ;
#16738 = CARTESIAN_POINT ( 'NONE',  ( -15.75283698213507755, -7.548994588147243334, 67.32502552484606895 ) ) ;
#16739 = PLANE ( 'NONE',  #27120 ) ;
#16740 = CARTESIAN_POINT ( 'NONE',  ( -19.85534385759799036, -8.623186033802570094, 49.24843789510466507 ) ) ;
#16741 = CARTESIAN_POINT ( 'NONE',  ( -13.07136655094769750, -8.762923122256669473, 64.02451139116674028 ) ) ;
#16742 = DIRECTION ( 'NONE',  ( -0.9956360040033418457, 0.09332174201255234725, 0.000000000000000000 ) ) ;
#16743 = DIRECTION ( 'NONE',  ( 0.2573866790907599622, 0.9663084897829604669, 6.714855467380901661E-08 ) ) ;
#16744 = EDGE_LOOP ( 'NONE', ( #27875, #27550 ) ) ;
#16745 = CARTESIAN_POINT ( 'NONE',  ( -46.92409385541305511, -15.80920654474410725, 61.49999999999999289 ) ) ;
#16746 = EDGE_CURVE ( 'NONE', #32101, #35582, #36581, .T. ) ;
#16747 = CARTESIAN_POINT ( 'NONE',  ( -18.91168463870544869, -7.914867951563272719, 63.31600393140114136 ) ) ;
#16748 = CARTESIAN_POINT ( 'NONE',  ( 18.51825960693461681, 0.6486925162843356629, 50.69417723405735643 ) ) ;
#16749 = DIRECTION ( 'NONE',  ( 0.9687793358424821033, -0.2479245821708677133, 0.000000000000000000 ) ) ;
#16750 = CARTESIAN_POINT ( 'NONE',  ( -13.46392434612064015, -20.58285101795483030, 61.58816697997369261 ) ) ;
#16751 =( BOUNDED_CURVE ( )  B_SPLINE_CURVE ( 3, ( #38749, #45909, #46142, #46871 ),
 .UNSPECIFIED., .F., .F. ) 
 B_SPLINE_CURVE_WITH_KNOTS ( ( 4, 4 ),
 ( 0.4074455897393658432, 0.5000000000000000000 ),
 .UNSPECIFIED. ) 
 CURVE ( )  GEOMETRIC_REPRESENTATION_ITEM ( )  RATIONAL_B_SPLINE_CURVE ( ( 0.6983129098260896228, 0.7760317562606886543, 0.8765941196519900780, 0.9999999999999894529 ) ) 
 REPRESENTATION_ITEM ( '' )  );
#16752 = ORIENTED_EDGE ( 'NONE', *, *, #31105, .F. ) ;
#16753 = ORIENTED_EDGE ( 'NONE', *, *, #45488, .T. ) ;
#16754 = EDGE_CURVE ( 'NONE', #42423, #42114, #29789, .T. ) ;
#16755 = EDGE_CURVE ( 'NONE', #3147, #35561, #38765, .T. ) ;
#16756 = ORIENTED_EDGE ( 'NONE', *, *, #30482, .F. ) ;
#16757 = CARTESIAN_POINT ( 'NONE',  ( -13.92409385541305511, -10.10920654474410618, 81.99999999999998579 ) ) ;
#16758 =( NAMED_UNIT ( * ) PLANE_ANGLE_UNIT ( ) SI_UNIT ( $, .RADIAN. ) );
#16759 = ADVANCED_FACE ( 'NONE', ( #13104 ), #23701, .T. ) ;
#16760 = CARTESIAN_POINT ( 'NONE',  ( -21.77717176493317552, -9.327196854410527038, 63.49153729606454988 ) ) ;
#16761 = ADVANCED_FACE ( 'NONE', ( #21249 ), #2039, .T. ) ;
#16762 =( BOUNDED_CURVE ( )  B_SPLINE_CURVE ( 3, ( #12432, #16104, #46175, #35323 ),
 .UNSPECIFIED., .F., .F. ) 
 B_SPLINE_CURVE_WITH_KNOTS ( ( 4, 4 ),
 ( 0.4074455897393719495, 0.5000000000000000000 ),
 .UNSPECIFIED. ) 
 CURVE ( )  GEOMETRIC_REPRESENTATION_ITEM ( )  RATIONAL_B_SPLINE_CURVE ( ( 0.6983129098261073864, 0.7760317562607119690, 0.8765941196520098400, 1.000000000000002220 ) ) 
 REPRESENTATION_ITEM ( '' )  );
#16763 = VERTEX_POINT ( 'NONE', #13345 ) ;
#16764 =( BOUNDED_CURVE ( )  B_SPLINE_CURVE ( 3, ( #22927, #7663, #33467, #48267 ),
 .UNSPECIFIED., .F., .F. ) 
 B_SPLINE_CURVE_WITH_KNOTS ( ( 4, 4 ),
 ( 0.5000000000000000000, 0.9074455897393621795 ),
 .UNSPECIFIED. ) 
 CURVE ( )  GEOMETRIC_REPRESENTATION_ITEM ( )  RATIONAL_B_SPLINE_CURVE ( ( 0.9999999999999985567, 0.4567392136813397396, 0.3561768502900340971, 0.6983129098260800749 ) ) 
 REPRESENTATION_ITEM ( '' )  );
#16765 = CARTESIAN_POINT ( 'NONE',  ( -21.95395705827280963, -8.894478678276469097, 66.91795930326043162 ) ) ;
#16766 = CARTESIAN_POINT ( 'NONE',  ( -10.00747521095153303, -15.51449648374953050, 57.61146884931378054 ) ) ;
#16767 = EDGE_CURVE ( 'NONE', #24011, #1356, #33412, .T. ) ;
#16768 = AXIS2_PLACEMENT_3D ( 'NONE', #3589, #36817, #6804 ) ;
#16769 = EDGE_LOOP ( 'NONE', ( #41693, #26030, #36175, #3975, #23226 ) ) ;
#16770 = DIRECTION ( 'NONE',  ( -3.071710424422018668E-17, 6.404604876783312462E-16, 1.000000000000000000 ) ) ;
#16771 = CARTESIAN_POINT ( 'NONE',  ( -23.08280660609100110, -10.60377317445056811, 59.61675562601556067 ) ) ;
#16772 = ORIENTED_EDGE ( 'NONE', *, *, #25612, .T. ) ;
#16773 = CARTESIAN_POINT ( 'NONE',  ( -16.78411710364782650, -21.83009890335197767, 68.99560651669348488 ) ) ;
#16774 = VERTEX_POINT ( 'NONE', #32560 ) ;
#16775 = DIRECTION ( 'NONE',  ( -0.3964226963016464489, -0.9180681052388938168, 0.000000000000000000 ) ) ;
#16776 =( BOUNDED_CURVE ( )  B_SPLINE_CURVE ( 3, ( #42559, #4630, #42060, #12255 ),
 .UNSPECIFIED., .F., .F. ) 
 B_SPLINE_CURVE_WITH_KNOTS ( ( 4, 4 ),
 ( 0.4074455897393595705, 0.5000000000000000000 ),
 .UNSPECIFIED. ) 
 CURVE ( )  GEOMETRIC_REPRESENTATION_ITEM ( )  RATIONAL_B_SPLINE_CURVE ( ( 0.6983129098260714152, 0.7760317562606651176, 0.8765941196519704270, 0.9999999999999770184 ) ) 
 REPRESENTATION_ITEM ( '' )  );
#16777 = EDGE_LOOP ( 'NONE', ( #16628, #23982, #20269, #20501 ) ) ;
#16778 = CARTESIAN_POINT ( 'NONE',  ( -16.39815193125092208, -7.826197509823805909, 63.81444203941759952 ) ) ;
#16779 = CARTESIAN_POINT ( 'NONE',  ( -23.30963478160716562, -18.69084381296369557, 69.30844128244088154 ) ) ;
#16780 = DIRECTION ( 'NONE',  ( 0.000000000000000000, 0.000000000000000000, 1.000000000000000000 ) ) ;
#16781 = ORIENTED_EDGE ( 'NONE', *, *, #43383, .T. ) ;
#16782 = DIRECTION ( 'NONE',  ( 1.000000000000000000, -0.000000000000000000, 2.081668171172170091E-15 ) ) ;
#16783 = CARTESIAN_POINT ( 'NONE',  ( -20.92409385759799179, -9.359200813967568422, 50.49621490985803263 ) ) ;
#16784 = CARTESIAN_POINT ( 'NONE',  ( -22.22496508270376481, -20.50616197626463233, 58.80796965402809917 ) ) ;
#16785 = CARTESIAN_POINT ( 'NONE',  ( -19.28939690137687535, -8.062307696266060475, 59.96092997387292201 ) ) ;
#16786 = DIRECTION ( 'NONE',  ( 0.000000000000000000, 0.000000000000000000, -1.000000000000000000 ) ) ;
#16787 = CARTESIAN_POINT ( 'NONE',  ( -10.39404051354841485, -17.27517550453656625, 61.25719493627910595 ) ) ;
#16788 = ORIENTED_EDGE ( 'NONE', *, *, #28481, .T. ) ;
#16789 = CARTESIAN_POINT ( 'NONE',  ( -24.40914445986810577, -13.82741747260119958, 73.12271364670142759 ) ) ;
#16790 = DIRECTION ( 'NONE',  ( 1.000000000000000000, -4.164305804376849172E-17, 1.614929280266638808E-16 ) ) ;
#16791 = CARTESIAN_POINT ( 'NONE',  ( -17.42409385541300892, -14.80920654474439679, 56.49999999999994316 ) ) ;
#16792 = CARTESIAN_POINT ( 'NONE',  ( -15.20917060265737675, -21.92251279605420322, 68.73626286540100239 ) ) ;
#16793 = B_SPLINE_CURVE_WITH_KNOTS ( 'NONE', 1,
 ( #29531, #25836 ),
 .UNSPECIFIED., .F., .F.,
 ( 2, 2 ),
 ( 0.000000000000000000, 1.000000000000000000 ),
 .UNSPECIFIED. ) ;
#16794 = CARTESIAN_POINT ( 'NONE',  ( -22.10677449762105340, -15.19398901379252820, 49.52966884056655772 ) ) ;
#16795 = CARTESIAN_POINT ( 'NONE',  ( -16.05534385650551599, -7.417179338643134834, 52.18511593390279302 ) ) ;
#16796 = VERTEX_POINT ( 'NONE', #2529 ) ;
#16797 = CARTESIAN_POINT ( 'NONE',  ( -24.46809763383182101, -15.25302497427750303, 73.15870697135122214 ) ) ;
#16798 = ORIENTED_EDGE ( 'NONE', *, *, #31717, .T. ) ;
#16799 = CARTESIAN_POINT ( 'NONE',  ( -10.37599212182869124, -14.63324797960940771, 71.34254748307667171 ) ) ;
#16800 = CARTESIAN_POINT ( 'NONE',  ( -16.78865592400587659, -21.78030535593112305, 68.99560651886281448 ) ) ;
#16801 = CARTESIAN_POINT ( 'NONE',  ( -14.55629311593335373, -8.423554203384631123, 63.80481326471479520 ) ) ;
#16802 = CARTESIAN_POINT ( 'NONE',  ( -19.51114651407244338, -7.656733154341000436, 60.14748342315007790 ) ) ;
#16803 = FACE_OUTER_BOUND ( 'NONE', #12212, .T. ) ;
#16804 = ADVANCED_FACE ( 'NONE', ( #20998 ), #48542, .T. ) ;
#16805 = ORIENTED_EDGE ( 'NONE', *, *, #33351, .T. ) ;
#16806 = CARTESIAN_POINT ( 'NONE',  ( -4.424093855413056886, -25.10920654474410441, 79.99999999999998579 ) ) ;
#16807 = CARTESIAN_POINT ( 'NONE',  ( -17.33887285826562774, -7.751749031259347333, 74.10451155337131013 ) ) ;
#16808 = CARTESIAN_POINT ( 'NONE',  ( -12.00862336911722927, -9.692924116444773475, 60.81563991731260188 ) ) ;
#16809 = ADVANCED_FACE ( 'NONE', ( #33022 ), #3484, .T. ) ;
#16810 = VERTEX_POINT ( 'NONE', #33758 ) ;
#16811 = AXIS2_PLACEMENT_3D ( 'NONE', #23964, #12860, #27885 ) ;
#16812 = CARTESIAN_POINT ( 'NONE',  ( -17.42409385541299471, -14.80920654474435771, 49.52966884056655772 ) ) ;
#16813 = DIRECTION ( 'NONE',  ( 3.413470714839332458E-33, -1.190614954331866791E-16, 1.000000000000000000 ) ) ;
#16814 = CARTESIAN_POINT ( 'NONE',  ( -42.29394679658953038, -14.80920654474410547, 64.04117647058822627 ) ) ;
#16815 = CARTESIAN_POINT ( 'NONE',  ( -16.39156059917436181, -21.78318494029796781, 62.05568132351888266 ) ) ;
#16816 = ORIENTED_EDGE ( 'NONE', *, *, #42418, .F. ) ;
#16817 = EDGE_LOOP ( 'NONE', ( #17816, #14498, #18071, #25573, #31370 ) ) ;
#16818 = CARTESIAN_POINT ( 'NONE',  ( -17.79909385541304445, -8.105421454601382081, 49.25000573077640098 ) ) ;
#16819 = CARTESIAN_POINT ( 'NONE',  ( -13.30711168077662521, -9.147894172712071281, 64.20946529582356277 ) ) ;
#16820 = EDGE_CURVE ( 'NONE', #24042, #15944, #41656, .T. ) ;
#16821 = EDGE_CURVE ( 'NONE', #30534, #44919, #18328, .T. ) ;
#16822 = CARTESIAN_POINT ( 'NONE',  ( -24.60655895611017741, -12.83064783748087301, 66.45246738850991619 ) ) ;
#16823 = EDGE_CURVE ( 'NONE', #16518, #31075, #16124, .T. ) ;
#16824 = CARTESIAN_POINT ( 'NONE',  ( -10.78978130820344994, -12.42417047965500743, 57.62857332104950814 ) ) ;
#16825 = CARTESIAN_POINT ( 'NONE',  ( -24.34502428176253019, -17.56683243011407924, 66.12852677468319484 ) ) ;
#16826 = ORIENTED_EDGE ( 'NONE', *, *, #6275, .T. ) ;
#16827 = CARTESIAN_POINT ( 'NONE',  ( -28.42409385541305511, -6.859206544744110623, 54.99999999999996447 ) ) ;
#16828 = CARTESIAN_POINT ( 'NONE',  ( -24.36966136476852540, -17.50601128794927774, 69.59995046513768102 ) ) ;
#16829 = EDGE_CURVE ( 'NONE', #20668, #23498, #30812, .T. ) ;
#16830 = ORIENTED_EDGE ( 'NONE', *, *, #5321, .T. ) ;
#16831 = CARTESIAN_POINT ( 'NONE',  ( -21.28537490900993134, -20.64804638814173288, 72.82446480614137840 ) ) ;
#16832 = CARTESIAN_POINT ( 'NONE',  ( -12.96069338448818087, -9.414713290161156323, 74.42996161600342475 ) ) ;
#16833 = CIRCLE ( 'NONE', #48302, 0.5560000000000009379 ) ;
#16834 = EDGE_LOOP ( 'NONE', ( #21556, #1098, #18072, #43368 ) ) ;
#16835 = CARTESIAN_POINT ( 'NONE',  ( -11.39216336840796373, -18.45920852072106300, 61.29182966166492719 ) ) ;
#16836 = CARTESIAN_POINT ( 'NONE',  ( -12.24245772170515956, -19.51581775654790718, 58.22682380653618139 ) ) ;
#16837 = VERTEX_POINT ( 'NONE', #2998 ) ;
#16838 = CARTESIAN_POINT ( 'NONE',  ( -17.63792724537347212, -22.25688666393347859, 58.59208636575791473 ) ) ;
#16839 = PRODUCT_DEFINITION ( 'UNKNOWN', '', #18811, #20389 ) ;
#16840 = AXIS2_PLACEMENT_3D ( 'NONE', #11355, #8165, #30332 ) ;
#16841 = CARTESIAN_POINT ( 'NONE',  ( -10.00889297783421128, -15.53016721190119753, 57.70646298183843470 ) ) ;
#16842 = CARTESIAN_POINT ( 'NONE',  ( -26.42409385541305511, -8.109206544744111511, 50.50000000000000000 ) ) ;
#16843 = DIRECTION ( 'NONE',  ( -0.8858372764600287441, -0.4639960340712824260, 4.734734194490170989E-17 ) ) ;
#16844 = EDGE_LOOP ( 'NONE', ( #20543, #45537, #37870, #44540 ) ) ;
#16845 = B_SPLINE_CURVE_WITH_KNOTS ( 'NONE', 3,
 ( #12697, #42747, #39035, #42016, #648, #26758, #41777, #30941, #45952, #8062 ),
 .UNSPECIFIED., .F., .F.,
 ( 4, 2, 2, 2, 4 ),
 ( 0.000000000000000000, 0.2500000000000000000, 0.5000000000000000000, 0.7500000000000000000, 1.000000000000000000 ),
 .UNSPECIFIED. ) ;
#16846 = CARTESIAN_POINT ( 'NONE',  ( -10.31252162633752079, -12.58677457285831913, 60.91198276946202128 ) ) ;
#16847 = LINE ( 'NONE', #31886, #23460 ) ;
#16848 = CARTESIAN_POINT ( 'NONE',  ( -13.42364920204782841, -9.064338107659910548, 49.69363550579117117 ) ) ;
#16849 = CARTESIAN_POINT ( 'NONE',  ( -11.86614749421525339, -19.77135288044581429, 58.11337654531251218 ) ) ;
#16850 = DIRECTION ( 'NONE',  ( -3.071710424422018668E-17, 6.404604876783312462E-16, 1.000000000000000000 ) ) ;
#16851 = CARTESIAN_POINT ( 'NONE',  ( -17.29025345054776963, -7.359659516233258536, 67.13384346071842401 ) ) ;
#16852 = CARTESIAN_POINT ( 'NONE',  ( -10.50893933415051507, -13.43540278197273885, 74.96345540680638919 ) ) ;
#16853 = VERTEX_POINT ( 'NONE', #18251 ) ;
#16854 = DIRECTION ( 'NONE',  ( -0.2075053346947394739, 0.3961584734335801827, 0.8944271909999157444 ) ) ;
#16855 =( BOUNDED_CURVE ( )  B_SPLINE_CURVE ( 3, ( #48642, #44246, #163, #19097 ),
 .UNSPECIFIED., .F., .F. ) 
 B_SPLINE_CURVE_WITH_KNOTS ( ( 4, 4 ),
 ( 0.9074455897393670645, 1.000000000000000000 ),
 .UNSPECIFIED. ) 
 CURVE ( )  GEOMETRIC_REPRESENTATION_ITEM ( )  RATIONAL_B_SPLINE_CURVE ( ( 0.6983129098260884016, 0.7760317562606942055, 0.8765941196519980716, 1.000000000000000000 ) ) 
 REPRESENTATION_ITEM ( '' )  );
#16856 = CARTESIAN_POINT ( 'NONE',  ( -18.50932031946840439, -21.77517977232111690, 72.43510940650374152 ) ) ;
#16857 = CARTESIAN_POINT ( 'NONE',  ( -45.92409385541306222, -14.20920654474410760, 70.50000000000000000 ) ) ;
#16858 = EDGE_CURVE ( 'NONE', #21561, #20725, #22599, .T. ) ;
#16859 = EDGE_LOOP ( 'NONE', ( #9296, #23649, #48029, #36342 ) ) ;
#16860 = CARTESIAN_POINT ( 'NONE',  ( -17.42409385541299471, -14.80920654474435771, 49.52966884056655772 ) ) ;
#16861 = ORIENTED_EDGE ( 'NONE', *, *, #23169, .T. ) ;
#16862 = ORIENTED_EDGE ( 'NONE', *, *, #8009, .T. ) ;
#16863 = ORIENTED_EDGE ( 'NONE', *, *, #34258, .T. ) ;
#16864 = CARTESIAN_POINT ( 'NONE',  ( -19.04853579327176760, -7.948602568230340282, 63.71617106789811658 ) ) ;
#16865 = CARTESIAN_POINT ( 'NONE',  ( -23.91439695282944200, -17.43141281116713515, 66.24357239631997629 ) ) ;
#16866 = CARTESIAN_POINT ( 'NONE',  ( -22.66727051383977809, -10.09628829486277546, 70.31178520457007153 ) ) ;
#16867 = CARTESIAN_POINT ( 'NONE',  ( -22.48430581236326731, -20.27711595259535571, 65.81926302645771898 ) ) ;
#16868 = CARTESIAN_POINT ( 'NONE',  ( -16.36080021583335409, -22.18299097935824093, 61.94842262253246901 ) ) ;
#16869 = VERTEX_POINT ( 'NONE', #45122 ) ;
#16870 = ORIENTED_EDGE ( 'NONE', *, *, #7685, .F. ) ;
#16871 = CIRCLE ( 'NONE', #33377, 1.500000000000008216 ) ;
#16872 = CARTESIAN_POINT ( 'NONE',  ( -20.24909385650551386, -8.104110260919579645, 48.81699501597546487 ) ) ;
#16873 = ADVANCED_FACE ( 'NONE', ( #40915 ), #47119, .F. ) ;
#16874 = CARTESIAN_POINT ( 'NONE',  ( -21.17484060445739757, -20.78220707328100403, 72.93935319279944451 ) ) ;
#16875 = CARTESIAN_POINT ( 'NONE',  ( -20.70759918696101920, -21.04805149802216846, 58.93915383139984954 ) ) ;
#16876 = FACE_OUTER_BOUND ( 'NONE', #43155, .T. ) ;
#16877 = EDGE_CURVE ( 'NONE', #40684, #32966, #28703, .T. ) ;
#16878 = CARTESIAN_POINT ( 'NONE',  ( -21.14909385650551599, -8.104110260919577868, 48.81699501597546487 ) ) ;
#16879 = EDGE_LOOP ( 'NONE', ( #7364, #37036, #1396, #42993, #16327 ) ) ;
#16880 = EDGE_CURVE ( 'NONE', #27231, #45924, #26708, .T. ) ;
#16881 = CARTESIAN_POINT ( 'NONE',  ( -14.72055112114360753, -21.75152931705752479, 61.79746922803622766 ) ) ;
#16882 = DIRECTION ( 'NONE',  ( -0.9687793358424821033, 0.2479245821708679076, 0.000000000000000000 ) ) ;
#16883 = CARTESIAN_POINT ( 'NONE',  ( -12.54253407177667512, -19.82621502378690082, 65.16674886820000268 ) ) ;
#16884 = EDGE_CURVE ( 'NONE', #23498, #16178, #6727, .T. ) ;
#16885 = VERTEX_POINT ( 'NONE', #42389 ) ;
#16886 = CARTESIAN_POINT ( 'NONE',  ( -10.81230840161673967, -17.25685697075765646, 64.64211442681141762 ) ) ;
#16887 = CARTESIAN_POINT ( 'NONE',  ( -10.40174226954351866, -17.29724918936392442, 61.34238429002267878 ) ) ;
#16888 = CARTESIAN_POINT ( 'NONE',  ( -16.35448746628295424, -21.72700549332279607, 58.39471472850929956 ) ) ;
#16889 = CARTESIAN_POINT ( 'NONE',  ( -14.40132536252195194, -7.999811592943899541, 63.92832360672956327 ) ) ;
#16890 = ORIENTED_EDGE ( 'NONE', *, *, #14764, .T. ) ;
#16891 = DIRECTION ( 'NONE',  ( 0.000000000000000000, 0.000000000000000000, 1.000000000000000000 ) ) ;
#16892 =( BOUNDED_SURFACE ( )  B_SPLINE_SURFACE ( 3, 1, ( 
 ( #24817, #9319 ),
 ( #32447, #39348 ),
 ( #12764, #47224 ),
 ( #28268, #20148 ),
 ( #16441, #32208 ),
 ( #35404, #20643 ),
 ( #5636, #13218 ) ),
 .UNSPECIFIED., .T., .F., .F. ) 
 B_SPLINE_SURFACE_WITH_KNOTS ( ( 4, 3, 4 ),
 ( 2, 2 ),
 ( 0.000000000000000000, 0.5000000000000000000, 1.000000000000000000 ),
 ( 0.000000000000000000, 1.000000000000000000 ),
 .UNSPECIFIED. ) 
 GEOMETRIC_REPRESENTATION_ITEM ( )  RATIONAL_B_SPLINE_SURFACE ( (
 ( 1.000000000000000000, 1.000000000000000000),
 ( 0.3333333333333335369, 0.3333333333333330373),
 ( 0.3333333333333335369, 0.3333333333333330373),
 ( 1.000000000000000000, 1.000000000000000000),
 ( 0.3333333333333333703, 0.3333333333333333703),
 ( 0.3333333333333333703, 0.3333333333333333703),
 ( 1.000000000000000000, 1.000000000000000000) ) ) 
 REPRESENTATION_ITEM ( '' )  SURFACE ( )  );
#16893 = ADVANCED_FACE ( 'NONE', ( #4715 ), #19736, .T. ) ;
#16894 = CARTESIAN_POINT ( 'NONE',  ( -22.85827772906650424, -10.39656997657325910, 63.07185958088085442 ) ) ;
#16895 = CARTESIAN_POINT ( 'NONE',  ( -18.03604899883812607, -21.78284559735032033, 65.62915604077223009 ) ) ;
#16896 = EDGE_LOOP ( 'NONE', ( #13920, #25271, #2326, #17951, #40905 ) ) ;
#16897 = FACE_OUTER_BOUND ( 'NONE', #27219, .T. ) ;
#16898 = EDGE_CURVE ( 'NONE', #26785, #7468, #3250, .T. ) ;
#16899 = ORIENTED_EDGE ( 'NONE', *, *, #37152, .F. ) ;
#16900 = AXIS2_PLACEMENT_3D ( 'NONE', #30950, #11745, #42270 ) ;
#16901 = CARTESIAN_POINT ( 'NONE',  ( -14.92957465851463006, -21.82926012297162899, 65.22101360901100975 ) ) ;
#16902 = CARTESIAN_POINT ( 'NONE',  ( -16.32142960126235209, -21.72225670208395343, 62.03951630124149119 ) ) ;
#16903 = ORIENTED_EDGE ( 'NONE', *, *, #17450, .T. ) ;
#16904 = ADVANCED_FACE ( 'NONE', ( #30588 ), #35309, .T. ) ;
#16905 = CARTESIAN_POINT ( 'NONE',  ( -10.60402983012795808, -16.62626367578652520, 57.83193508283319773 ) ) ;
#16906 = CARTESIAN_POINT ( 'NONE',  ( -21.79520159808653190, -20.27875113210311753, 58.87516014074775228 ) ) ;
#16907 = AXIS2_PLACEMENT_3D ( 'NONE', #24765, #39766, #27955 ) ;
#16908 = CARTESIAN_POINT ( 'NONE',  ( -13.18494979104506015, -8.682762004662409439, 60.48304321394137162 ) ) ;
#16909 = PLANE ( 'NONE',  #32930 ) ;
#16910 = ORIENTED_EDGE ( 'NONE', *, *, #38312, .T. ) ;
#16911 = DIRECTION ( 'NONE',  ( -3.071710424422018668E-17, 6.404604876783312462E-16, 1.000000000000000000 ) ) ;
#16912 = ADVANCED_FACE ( 'NONE', ( #16572 ), #31361, .T. ) ;
#16913 = CARTESIAN_POINT ( 'NONE',  ( -12.74698474939898318, -12.42443183621509917, 52.02966884056656482 ) ) ;
#16914 = CARTESIAN_POINT ( 'NONE',  ( -10.09291371782238045, -16.13494220690481384, 68.16263107114907882 ) ) ;
#16915 = EDGE_LOOP ( 'NONE', ( #9437, #48384 ) ) ;
#16916 = CARTESIAN_POINT ( 'NONE',  ( -11.42622260759249464, -18.51434353338492400, 61.57710833179551457 ) ) ;
#16917 =( BOUNDED_SURFACE ( )  B_SPLINE_SURFACE ( 3, 1, ( 
 ( #40002, #39517 ),
 ( #2576, #24519 ),
 ( #12919, #32610 ),
 ( #13867, #13636 ),
 ( #36293, #5304 ),
 ( #24266, #20320 ),
 ( #31888, #43709 ) ),
 .UNSPECIFIED., .T., .F., .F. ) 
 B_SPLINE_SURFACE_WITH_KNOTS ( ( 4, 3, 4 ),
 ( 2, 2 ),
 ( 0.000000000000000000, 0.5000000000000000000, 1.000000000000000000 ),
 ( 0.000000000000000000, 1.000000000000000000 ),
 .UNSPECIFIED. ) 
 GEOMETRIC_REPRESENTATION_ITEM ( )  RATIONAL_B_SPLINE_SURFACE ( (
 ( 1.000000000000000000, 1.000000000000000000),
 ( 0.3333333333333335369, 0.3333333333333330373),
 ( 0.3333333333333335369, 0.3333333333333330373),
 ( 1.000000000000000000, 1.000000000000000000),
 ( 0.3333333333333333703, 0.3333333333333333703),
 ( 0.3333333333333333703, 0.3333333333333333703),
 ( 1.000000000000000000, 1.000000000000000000) ) ) 
 REPRESENTATION_ITEM ( '' )  SURFACE ( )  );
#16918 = CARTESIAN_POINT ( 'NONE',  ( -11.06712688165958269, -18.69414528815109477, 61.39215548186584215 ) ) ;
#16919 = ORIENTED_EDGE ( 'NONE', *, *, #41499, .F. ) ;
#16920 = ORIENTED_EDGE ( 'NONE', *, *, #4670, .T. ) ;
#16921 = DIRECTION ( 'NONE',  ( 0.000000000000000000, 0.000000000000000000, 1.000000000000000000 ) ) ;
#16922 = DIRECTION ( 'NONE',  ( -0.9345716196833626643, 0.3557750520798445559, 2.412542607589989711E-09 ) ) ;
#16923 = CARTESIAN_POINT ( 'NONE',  ( -10.37462438995674319, -14.89569194323783030, 74.79778901495059529 ) ) ;
#16924 = CARTESIAN_POINT ( 'NONE',  ( -18.92409385650551812, -6.426201560718813433, 50.50509628382439331 ) ) ;
#16925 = CARTESIAN_POINT ( 'NONE',  ( -11.53247254227971474, -18.68106628708273931, 65.04707076447483871 ) ) ;
#16926 = CARTESIAN_POINT ( 'NONE',  ( -22.98865756656685022, -9.855479763439479512, 70.12683098403445570 ) ) ;
#16927 = CARTESIAN_POINT ( 'NONE',  ( -10.82793724842355765, -11.34591556451386651, 67.87510537416113721 ) ) ;
#16928 = EDGE_LOOP ( 'NONE', ( #44196, #30386, #45079, #1327, #31088 ) ) ;
#16929 = VERTEX_POINT ( 'NONE', #42208 ) ;
#16930 = CARTESIAN_POINT ( 'NONE',  ( -12.34220853212439550, -20.25709170942694115, 68.47624048511032413 ) ) ;
#16931 = DIRECTION ( 'NONE',  ( -3.071710424422018668E-17, 6.404604876783312462E-16, 1.000000000000000000 ) ) ;
#16932 = CARTESIAN_POINT ( 'NONE',  ( -20.66696756681432490, -21.06910030335248152, 58.64475164910062688 ) ) ;
#16933 = FACE_OUTER_BOUND ( 'NONE', #3984, .T. ) ;
#16934 = CARTESIAN_POINT ( 'NONE',  ( -17.42409385541299471, -14.80920654474434883, 62.02966884056656482 ) ) ;
#16935 = ORIENTED_EDGE ( 'NONE', *, *, #43855, .F. ) ;
#16936 = EDGE_CURVE ( 'NONE', #34178, #7173, #15170, .T. ) ;
#16937 = CARTESIAN_POINT ( 'NONE',  ( -14.92764441971231726, -21.34891144748960201, 61.93600440564248544 ) ) ;
#16938 = CARTESIAN_POINT ( 'NONE',  ( -24.02655296236175175, -11.35792967378293916, 66.53719098615387395 ) ) ;
#16939 = EDGE_CURVE ( 'NONE', #2617, #3562, #4847, .T. ) ;
#16940 = CARTESIAN_POINT ( 'NONE',  ( -14.95356710262008626, -21.83765618392649444, 65.30607879145217964 ) ) ;
#16941 = CARTESIAN_POINT ( 'NONE',  ( -24.46557908765160860, -17.24254831546467415, 73.13981945087590475 ) ) ;
#16942 = VERTEX_POINT ( 'NONE', #5269 ) ;
#16943 = CARTESIAN_POINT ( 'NONE',  ( -10.13939525383658236, -13.24794156168132275, 74.80100763153892274 ) ) ;
#16944 = CARTESIAN_POINT ( 'NONE',  ( -23.00382044653182945, -10.58231046269237829, 59.60203429539187425 ) ) ;
#16945 = DIRECTION ( 'NONE',  ( -1.000000000000000000, 4.164305804376849172E-17, -1.614929280266638808E-16 ) ) ;
#16946 = FILL_AREA_STYLE ('',( #41595 ) ) ;
#16947 = CYLINDRICAL_SURFACE ( 'NONE', #6861, 2.000000000000001776 ) ;
#16948 = CARTESIAN_POINT ( 'NONE',  ( -23.47974657088402850, -11.29780683472819724, 70.17745371881790106 ) ) ;
#16949 = ORIENTED_EDGE ( 'NONE', *, *, #8390, .F. ) ;
#16950 = CARTESIAN_POINT ( 'NONE',  ( -20.30349787717712573, -7.937960560238677132, 70.38953857791403834 ) ) ;
#16951 = EDGE_CURVE ( 'NONE', #13117, #1942, #35295, .T. ) ;
#16952 = ORIENTED_EDGE ( 'NONE', *, *, #9089, .T. ) ;
#16953 = CARTESIAN_POINT ( 'NONE',  ( -11.28948497894591263, -19.03661189358662043, 68.33972770741397085 ) ) ;
#16954 = CARTESIAN_POINT ( 'NONE',  ( -21.56016804333223646, -8.612711131324969571, 73.64482796973915413 ) ) ;
#16955 = EDGE_LOOP ( 'NONE', ( #30996, #23494 ) ) ;
#16956 = EDGE_CURVE ( 'NONE', #2636, #24853, #16751, .T. ) ;
#16957 = EDGE_CURVE ( 'NONE', #20590, #1538, #13666, .T. ) ;
#16958 = EDGE_CURVE ( 'NONE', #27154, #32100, #42704, .T. ) ;
#16959 = CARTESIAN_POINT ( 'NONE',  ( -14.54749350918766204, -8.372447261038935551, 64.07506791522041567 ) ) ;
#16960 = CARTESIAN_POINT ( 'NONE',  ( -15.41159385650551705, -6.922745924619793101, 51.69366785382590024 ) ) ;
#16961 = VERTEX_POINT ( 'NONE', #16320 ) ;
#16962 = DIRECTION ( 'NONE',  ( 9.588441152175118139E-09, 2.115493544230230216E-07, 0.9999999999999775735 ) ) ;
#16963 = CARTESIAN_POINT ( 'NONE',  ( -19.94917705995926482, -8.226604131702123013, 74.00624557436877637 ) ) ;
#16964 = CARTESIAN_POINT ( 'NONE',  ( -10.93142192406588720, -17.42570591193873497, 64.85412782098468654 ) ) ;
#16965 = ORIENTED_EDGE ( 'NONE', *, *, #45905, .F. ) ;
#16966 = CARTESIAN_POINT ( 'NONE',  ( -16.19404102203350249, -7.918066801900436325, 60.21530862784245386 ) ) ;
#16967 = CARTESIAN_POINT ( 'NONE',  ( -11.57126885336172073, -10.86466612894600381, 74.59451641100736197 ) ) ;
#16968 = AXIS2_PLACEMENT_3D ( 'NONE', #31011, #37649, #46032 ) ;
#16969 = CYLINDRICAL_SURFACE ( 'NONE', #35331, 4.686499999999997002 ) ;
#16970 = LINE ( 'NONE', #47029, #18385 ) ;
#16971 = ORIENTED_EDGE ( 'NONE', *, *, #43012, .T. ) ;
#16972 = ORIENTED_EDGE ( 'NONE', *, *, #14781, .F. ) ;
#16973 = ORIENTED_EDGE ( 'NONE', *, *, #27684, .T. ) ;
#16974 = FACE_OUTER_BOUND ( 'NONE', #37745, .T. ) ;
#16975 = CARTESIAN_POINT ( 'NONE',  ( -21.99178464560338497, -9.439038884874848989, 59.87171213140518944 ) ) ;
#16976 = CARTESIAN_POINT ( 'NONE',  ( -19.91159385759799250, -8.990409506049200417, 49.61344411288074951 ) ) ;
#16977 = CARTESIAN_POINT ( 'NONE',  ( -10.42592298192601241, -14.97187847733016142, 75.08313515325615128 ) ) ;
#16978 = DIRECTION ( 'NONE',  ( -0.9294853595766571219, -0.3688590060343552857, 0.000000000000000000 ) ) ;
#16979 = CARTESIAN_POINT ( 'NONE',  ( -11.31272926253210542, -18.32407376160489676, 57.80714615569726078 ) ) ;
#16980 = ORIENTED_EDGE ( 'NONE', *, *, #7584, .F. ) ;
#16981 = CARTESIAN_POINT ( 'NONE',  ( -16.38321341446914658, -21.78497919871296062, 65.64053219190310529 ) ) ;
#16982 = EDGE_CURVE ( 'NONE', #44055, #33140, #47263, .T. ) ;
#16983 = CARTESIAN_POINT ( 'NONE',  ( -8.424093855413094190, -25.10920654474410441, 64.00000000000002842 ) ) ;
#16984 = CARTESIAN_POINT ( 'NONE',  ( -22.79444606840252874, -10.23710104419528122, 62.95697184964878090 ) ) ;
#16985 = CARTESIAN_POINT ( 'NONE',  ( -24.87417209744295477, -14.81009202510037959, 59.28654333241698993 ) ) ;
#16986 = CARTESIAN_POINT ( 'NONE',  ( -10.79220851498797096, -11.41472892741485623, 67.79581491584505670 ) ) ;
#16987 = EDGE_LOOP ( 'NONE', ( #37519, #43735 ) ) ;
#16988 = ORIENTED_EDGE ( 'NONE', *, *, #45968, .F. ) ;
#16989 = ORIENTED_EDGE ( 'NONE', *, *, #38880, .F. ) ;
#16990 = CARTESIAN_POINT ( 'NONE',  ( -10.88210961209655636, -12.31514285474667503, 57.40027529950947383 ) ) ;
#16991 = LINE ( 'NONE', #32292, #47284 ) ;
#16992 = ADVANCED_FACE ( 'NONE', ( #8730 ), #21792, .T. ) ;
#16993 = DIRECTION ( 'NONE',  ( -0.3478314405900341799, -0.9375570856950852239, 0.000000000000000000 ) ) ;
#16994 = ORIENTED_EDGE ( 'NONE', *, *, #1289, .F. ) ;
#16995 = FACE_OUTER_BOUND ( 'NONE', #48392, .T. ) ;
#16996 = CIRCLE ( 'NONE', #13067, 5.000000000000000000 ) ;
#16997 = B_SPLINE_CURVE_WITH_KNOTS ( 'NONE', 3,
 ( #38746, #38243, #5264, #5028, #23497, #23753, #42206, #27421, #35043, #8239 ),
 .UNSPECIFIED., .F., .F.,
 ( 4, 2, 2, 2, 4 ),
 ( 0.6272669072978649396, 0.7522669073148475771, 0.8772669073318302146, 1.002266907348812852, 1.127266907365795490 ),
 .UNSPECIFIED. ) ;
#16998 = PLANE ( 'NONE',  #35117 ) ;
#16999 = ORIENTED_EDGE ( 'NONE', *, *, #786, .T. ) ;
#17000 = CARTESIAN_POINT ( 'NONE',  ( -11.27120819164457899, -11.36022928427317957, 67.71044750680073321 ) ) ;
#17001 = CARTESIAN_POINT ( 'NONE',  ( -19.07667242297576138, -10.41096375660395168, 49.52966884056655772 ) ) ;
#17002 = EDGE_LOOP ( 'NONE', ( #4577, #7727 ) ) ;
#17003 = CARTESIAN_POINT ( 'NONE',  ( -15.84614975837744133, -7.989249925961589227, 67.14007226002782147 ) ) ;
#17004 = VERTEX_POINT ( 'NONE', #41969 ) ;
#17005 = CARTESIAN_POINT ( 'NONE',  ( -23.67245686711442687, -11.53637809225759625, 69.98390920472554910 ) ) ;
#17006 = ORIENTED_EDGE ( 'NONE', *, *, #4444, .T. ) ;
#17007 = CARTESIAN_POINT ( 'NONE',  ( -17.42409385541300182, -14.80920654474440745, 52.02966884056655061 ) ) ;
#17008 = CARTESIAN_POINT ( 'NONE',  ( -18.50534385759798894, -7.595227055684746986, 51.75156210489594599 ) ) ;
#17009 = CARTESIAN_POINT ( 'NONE',  ( -18.18338144371267617, -21.81849904615365432, 65.63060065626805795 ) ) ;
#17010 = EDGE_LOOP ( 'NONE', ( #9079, #18466 ) ) ;
#17011 = DIRECTION ( 'NONE',  ( 2.866981220435666553E-17, -1.000000000000000000, -1.190614954331866791E-16 ) ) ;
#17012 = ADVANCED_FACE ( 'NONE', ( #846 ), #38245, .T. ) ;
#17013 = EDGE_CURVE ( 'NONE', #43190, #45590, #5132, .T. ) ;
#17014 = DIRECTION ( 'NONE',  ( 1.000000000000000000, 2.866981220435666553E-17, 0.000000000000000000 ) ) ;
#17015 = DIRECTION ( 'NONE',  ( -2.866981220435666553E-17, 1.000000000000000000, 1.190614954331866791E-16 ) ) ;
#17016 = CARTESIAN_POINT ( 'NONE',  ( -20.01838156832885574, -21.36851401455050237, 68.93482423123572289 ) ) ;
#17017 = CARTESIAN_POINT ( 'NONE',  ( -13.84085632603101956, -17.84827948783496865, 52.02966884056656482 ) ) ;
#17018 = DIRECTION ( 'NONE',  ( -0.7700094066334558507, -0.6380325334150236394, 0.000000000000000000 ) ) ;
#17019 = EDGE_LOOP ( 'NONE', ( #47698, #12812 ) ) ;
#17020 = DIRECTION ( 'NONE',  ( 0.3047757271037812576, 0.9524197806957001022, 0.002884009000665203448 ) ) ;
#17021 = CARTESIAN_POINT ( 'NONE',  ( -24.65023647254185590, -12.99629722456026393, 63.01759562046499497 ) ) ;
#17022 = CARTESIAN_POINT ( 'NONE',  ( -16.22363853529886057, -7.456506500845998531, 60.30754342289255732 ) ) ;
#17023 = ADVANCED_FACE ( 'NONE', ( #10173 ), #17543, .F. ) ;
#17024 = EDGE_CURVE ( 'NONE', #28884, #35750, #28237, .T. ) ;
#17025 = CARTESIAN_POINT ( 'NONE',  ( -23.35262004249965528, -18.62986191134476499, 65.70900547832829375 ) ) ;
#17026 = CARTESIAN_POINT ( 'NONE',  ( -10.98557796499954087, -17.68114198556070704, 71.86718193507100239 ) ) ;
#17027 = CARTESIAN_POINT ( 'NONE',  ( -16.28034385650551741, -6.424090610841176385, 49.80797279389978627 ) ) ;
#17029 = EDGE_CURVE ( 'NONE', #33357, #26197, #39720, .T. ) ;
#17028 = VERTEX_POINT ( 'NONE', #39483 ) ;
#17030 = CARTESIAN_POINT ( 'NONE',  ( -13.49145512112739631, -18.65424914341562612, 54.07175714974879099 ) ) ;
#17031 = CARTESIAN_POINT ( 'NONE',  ( -24.36252951794159571, -13.53973495479416478, 59.45448211580517750 ) ) ;
#17032 = ORIENTED_EDGE ( 'NONE', *, *, #11881, .T. ) ;
#17033 = DIRECTION ( 'NONE',  ( 0.000000000000000000, 0.9999954153791273948, 0.003028072113819836077 ) ) ;
#17034 = CARTESIAN_POINT ( 'NONE',  ( -10.13258914451759019, -16.33817228489381179, 71.63245656337019796 ) ) ;
#17035 = CARTESIAN_POINT ( 'NONE',  ( -14.50327952430959044, -8.447626442811719372, 64.01652269559008346 ) ) ;
#17036 = DIRECTION ( 'NONE',  ( 0.000000000000000000, 0.000000000000000000, 1.000000000000000000 ) ) ;
#17037 =( BOUNDED_SURFACE ( )  B_SPLINE_SURFACE ( 3, 1, ( 
 ( #27607, #34985 ),
 ( #20708, #16512 ),
 ( #23926, #46809 ),
 ( #46332, #4972 ),
 ( #2226, #12826 ),
 ( #31302, #38929 ),
 ( #39420, #47048 ) ),
 .UNSPECIFIED., .T., .F., .F. ) 
 B_SPLINE_SURFACE_WITH_KNOTS ( ( 4, 3, 4 ),
 ( 2, 2 ),
 ( 0.000000000000000000, 0.5000000000000000000, 1.000000000000000000 ),
 ( 0.000000000000000000, 1.000000000000000000 ),
 .UNSPECIFIED. ) 
 GEOMETRIC_REPRESENTATION_ITEM ( )  RATIONAL_B_SPLINE_SURFACE ( (
 ( 1.000000000000000000, 1.000000000000000000),
 ( 0.3333333333333335369, 0.3333333333333330373),
 ( 0.3333333333333335369, 0.3333333333333330373),
 ( 1.000000000000000000, 1.000000000000000000),
 ( 0.3333333333333333703, 0.3333333333333333703),
 ( 0.3333333333333333703, 0.3333333333333333703),
 ( 1.000000000000000000, 1.000000000000000000) ) ) 
 REPRESENTATION_ITEM ( '' )  SURFACE ( )  );
#17038 = EDGE_LOOP ( 'NONE', ( #40934, #13365, #9749, #46187, #47748 ) ) ;
#17039 = CARTESIAN_POINT ( 'NONE',  ( -24.72409385541305582, -14.80920654474424225, 70.07647058823528141 ) ) ;
#17040 = VECTOR ( 'NONE', #43873, 1000.000000000000227 ) ;
#17041 = CARTESIAN_POINT ( 'NONE',  ( -20.86206331040166262, -20.96415858629787721, 62.41471384001169298 ) ) ;
#17042 = AXIS2_PLACEMENT_3D ( 'NONE', #22798, #30429, #38027 ) ;
#17043 = CARTESIAN_POINT ( 'NONE',  ( -12.58002213166789041, -9.148928514680237711, 74.43427606957253317 ) ) ;
#17044 = EDGE_CURVE ( 'NONE', #2461, #5461, #11442, .T. ) ;
#17045 = ORIENTED_EDGE ( 'NONE', *, *, #12180, .T. ) ;
#17046 = CARTESIAN_POINT ( 'NONE',  ( -21.57946453887431204, -8.565578233975859490, 53.49999999999994316 ) ) ;
#17047 = SURFACE_SIDE_STYLE ('',( #31179 ) ) ;
#17048 = B_SPLINE_CURVE_WITH_KNOTS ( 'NONE', 3,
 ( #48359, #14592, #43971, #2587 ),
 .UNSPECIFIED., .F., .F.,
 ( 4, 4 ),
 ( 0.8266992229644638535, 1.000000000000000000 ),
 .UNSPECIFIED. ) ;
#17049 = VECTOR ( 'NONE', #3214, 1000.000000000000000 ) ;
#17050 = CARTESIAN_POINT ( 'NONE',  ( -13.41535341985785301, -9.069179271060303194, 63.98116896315330848 ) ) ;
#17051 = CARTESIAN_POINT ( 'NONE',  ( -20.86114118487399338, -21.41899753141851548, 58.84463944793498058 ) ) ;
#17052 = FACE_OUTER_BOUND ( 'NONE', #34918, .T. ) ;
#17053 =( BOUNDED_CURVE ( )  B_SPLINE_CURVE ( 3, ( #18293, #10455, #33545, #44204 ),
 .UNSPECIFIED., .F., .F. ) 
 B_SPLINE_CURVE_WITH_KNOTS ( ( 4, 4 ),
 ( 0.000000000000000000, 0.4074455897393645665 ),
 .UNSPECIFIED. ) 
 CURVE ( )  GEOMETRIC_REPRESENTATION_ITEM ( )  RATIONAL_B_SPLINE_CURVE ( ( 1.000000000000000000, 0.4567392136813290260, 0.3561768502900292122, 0.6983129098261006140 ) ) 
 REPRESENTATION_ITEM ( '' )  );
#17054 = CARTESIAN_POINT ( 'NONE',  ( -10.72615791900921423, -12.77470505732934747, 64.56836133915385290 ) ) ;
#17055 =( BOUNDED_SURFACE ( )  B_SPLINE_SURFACE ( 3, 1, ( 
 ( #23083, #910 ),
 ( #35103, #42272 ),
 ( #9029, #8536 ),
 ( #4849, #38561 ),
 ( #19868, #1134 ),
 ( #31182, #1370 ),
 ( #27485, #42520 ) ),
 .UNSPECIFIED., .T., .F., .F. ) 
 B_SPLINE_SURFACE_WITH_KNOTS ( ( 4, 3, 4 ),
 ( 2, 2 ),
 ( 0.000000000000000000, 0.5000000000000000000, 1.000000000000000000 ),
 ( 0.000000000000000000, 1.000000000000000000 ),
 .UNSPECIFIED. ) 
 GEOMETRIC_REPRESENTATION_ITEM ( )  RATIONAL_B_SPLINE_SURFACE ( (
 ( 1.000000000000000000, 1.000000000000000000),
 ( 0.3333333333333335369, 0.3333333333333330373),
 ( 0.3333333333333335369, 0.3333333333333330373),
 ( 1.000000000000000000, 1.000000000000000000),
 ( 0.3333333333333333703, 0.3333333333333333703),
 ( 0.3333333333333333703, 0.3333333333333333703),
 ( 1.000000000000000000, 1.000000000000000000) ) ) 
 REPRESENTATION_ITEM ( '' )  SURFACE ( )  );
#17056 = VERTEX_POINT ( 'NONE', #14068 ) ;
#17057 = ORIENTED_EDGE ( 'NONE', *, *, #25160, .F. ) ;
#17058 = CARTESIAN_POINT ( 'NONE',  ( -17.34909385541304161, -8.112991634885936776, 51.74999426922421719 ) ) ;
#17059 = LINE ( 'NONE', #24956, #9938 ) ;
#17060 = CARTESIAN_POINT ( 'NONE',  ( -14.07986447567954436, -8.151974645673341513, 70.92968827753317385 ) ) ;
#17061 =( BOUNDED_SURFACE ( )  B_SPLINE_SURFACE ( 3, 1, ( 
 ( #48448, #45038 ),
 ( #33922, #215 ),
 ( #15195, #41564 ),
 ( #8814, #34649 ),
 ( #16160, #4873 ),
 ( #42292, #19641 ),
 ( #42544, #30736 ) ),
 .UNSPECIFIED., .T., .F., .F. ) 
 B_SPLINE_SURFACE_WITH_KNOTS ( ( 4, 3, 4 ),
 ( 2, 2 ),
 ( 0.000000000000000000, 0.5000000000000000000, 1.000000000000000000 ),
 ( 0.000000000000000000, 1.000000000000000000 ),
 .UNSPECIFIED. ) 
 GEOMETRIC_REPRESENTATION_ITEM ( )  RATIONAL_B_SPLINE_SURFACE ( (
 ( 1.000000000000000000, 1.000000000000000000),
 ( 0.3333333333333335369, 0.3333333333333330373),
 ( 0.3333333333333335369, 0.3333333333333330373),
 ( 1.000000000000000000, 1.000000000000000000),
 ( 0.3333333333333333703, 0.3333333333333333703),
 ( 0.3333333333333333703, 0.3333333333333333703),
 ( 1.000000000000000000, 1.000000000000000000) ) ) 
 REPRESENTATION_ITEM ( '' )  SURFACE ( )  );
#17062 = CARTESIAN_POINT ( 'NONE',  ( -22.95693723218890980, -10.52102731622098375, 59.61705815066174097 ) ) ;
#17063 = DIRECTION ( 'NONE',  ( -9.637352644315596475E-17, 0.000000000000000000, -1.000000000000000000 ) ) ;
#17064 = EDGE_LOOP ( 'NONE', ( #22260, #40446, #38793, #28463, #31079 ) ) ;
#17065 = CARTESIAN_POINT ( 'NONE',  ( -21.11440761173729186, -20.75744868006576027, 65.77557061749909906 ) ) ;
#17066 = CARTESIAN_POINT ( 'NONE',  ( -24.72409385541305582, -14.90920654474410512, 56.99999999999998579 ) ) ;
#17067 = EDGE_LOOP ( 'NONE', ( #13158, #28009 ) ) ;
#17068 = DIRECTION ( 'NONE',  ( -3.071710424422018668E-17, 6.404604876783312462E-16, 1.000000000000000000 ) ) ;
#17069 = CARTESIAN_POINT ( 'NONE',  ( -11.98246295270348405, -15.60836430055780433, 54.07175714974878389 ) ) ;
#17070 = AXIS2_PLACEMENT_3D ( 'NONE', #47701, #13939, #10287 ) ;
#17071 = ORIENTED_EDGE ( 'NONE', *, *, #35262, .T. ) ;
#17072 = CARTESIAN_POINT ( 'NONE',  ( -24.11881394502254849, -17.01995806294775448, 73.16863963025599560 ) ) ;
#17073 = DIRECTION ( 'NONE',  ( 5.625773296287788022E-06, 7.100530152274343103E-06, 0.9999999999589664901 ) ) ;
#17074 = ORIENTED_EDGE ( 'NONE', *, *, #28511, .F. ) ;
#17075 = DIRECTION ( 'NONE',  ( -1.000000000000000000, -1.669677910507523057E-21, -6.493791346278465266E-22 ) ) ;
#17076 = EDGE_CURVE ( 'NONE', #5475, #34665, #36611, .T. ) ;
#17077 = DIRECTION ( 'NONE',  ( -0.06306825763707681054, 0.9980092158285027715, 2.415158932891090531E-08 ) ) ;
#17078 = AXIS2_PLACEMENT_3D ( 'NONE', #8502, #1842, #39018 ) ;
#17079 = DIRECTION ( 'NONE',  ( 1.027096116490394736E-05, 2.598167872976484874E-06, 0.9999999999438784481 ) ) ;
#17080 = CARTESIAN_POINT ( 'NONE',  ( -11.03124120290388532, -17.66077365132053956, 71.86718193465377169 ) ) ;
#17081 = ORIENTED_EDGE ( 'NONE', *, *, #46969, .F. ) ;
#17082 = CARTESIAN_POINT ( 'NONE',  ( -14.31269513454703102, -8.538704322430856308, 67.45078350274380341 ) ) ;
#17083 = CARTESIAN_POINT ( 'NONE',  ( -22.38400238879419391, -20.36826089713532895, 62.41934470639706944 ) ) ;
#17084 = CARTESIAN_POINT ( 'NONE',  ( -11.06818430912604256, -11.75871762752125349, 71.38860862825016795 ) ) ;
#17085 = DIRECTION ( 'NONE',  ( 0.7670373483544791204, 0.6416024518573233415, -2.496223344567303931E-08 ) ) ;
#17086 = ADVANCED_FACE ( 'NONE', ( #21259 ), #32571, .T. ) ;
#17087 = B_SPLINE_CURVE_WITH_KNOTS ( 'NONE', 3,
 ( #37934, #45107, #26369, #19721, #37685, #1003, #16000, #22945, #41384, #11848 ),
 .UNSPECIFIED., .F., .F.,
 ( 4, 2, 2, 2, 4 ),
 ( 0.1272669073658400374, 0.2522669073463247313, 0.3772669073268094531, 0.5022669073072940638, 0.6272669072877787855 ),
 .UNSPECIFIED. ) ;
#17088 = CARTESIAN_POINT ( 'NONE',  ( -19.94917705995926482, -8.226604131702123013, 74.00624557436877637 ) ) ;
#17089 = CARTESIAN_POINT ( 'NONE',  ( -17.33262245845742910, -7.759502110702281463, 67.30567542699309058 ) ) ;
#17090 = ADVANCED_FACE ( 'NONE', ( #43920 ), #2542, .T. ) ;
#17091 = CARTESIAN_POINT ( 'NONE',  ( -16.16063142123006813, -7.467037929575190525, 60.38523757159160965 ) ) ;
#17092 = DIRECTION ( 'NONE',  ( -0.4683180279402421875, 0.8835599723313412035, -4.589753180866139968E-08 ) ) ;
#17093 = VERTEX_POINT ( 'NONE', #40441 ) ;
#17094 = CARTESIAN_POINT ( 'NONE',  ( -24.34764189302621062, -17.56035350371566750, 66.06544510718885022 ) ) ;
#17095 = ADVANCED_FACE ( 'NONE', ( #36714 ), #5984, .F. ) ;
#17096 = DIRECTION ( 'NONE',  ( -1.000000000000000000, 0.000000000000000000, 0.000000000000000000 ) ) ;
#17097 = CARTESIAN_POINT ( 'NONE',  ( -9.999882549351870153, -15.43057416212389832, 57.70759442341619661 ) ) ;
#17098 = ORIENTED_EDGE ( 'NONE', *, *, #19502, .T. ) ;
#17099 = DIRECTION ( 'NONE',  ( 0.9687793358424821033, -0.2479245821708680464, 0.000000000000000000 ) ) ;
#17100 = VERTEX_POINT ( 'NONE', #17046 ) ;
#17101 = VERTEX_POINT ( 'NONE', #13358 ) ;
#17102 = VERTEX_POINT ( 'NONE', #21009 ) ;
#17103 = CARTESIAN_POINT ( 'NONE',  ( -19.11145865927416310, -7.964113456900453691, 63.43089235103783352 ) ) ;
#17104 = AXIS2_PLACEMENT_3D ( 'NONE', #24792, #17383, #46715 ) ;
#17105 = CARTESIAN_POINT ( 'NONE',  ( -17.42409385541299471, -14.80920654474435594, 52.02966884056656482 ) ) ;
#17106 = DIRECTION ( 'NONE',  ( 6.816999858124113439E-06, 9.113320815582587851E-06, 0.9999999999352379154 ) ) ;
#17107 = CARTESIAN_POINT ( 'NONE',  ( -15.29909385759798823, -8.105421454601382081, 49.25000573077640098 ) ) ;
#17108 = CARTESIAN_POINT ( 'NONE',  ( -23.47355814803600893, -18.42978312378849637, 73.05808415355102170 ) ) ;
#17109 = CIRCLE ( 'NONE', #35987, 4.686499999999998778 ) ;
#17110 = ORIENTED_EDGE ( 'NONE', *, *, #27684, .F. ) ;
#17111 = ORIENTED_EDGE ( 'NONE', *, *, #23270, .F. ) ;
#17112 = CARTESIAN_POINT ( 'NONE',  ( -19.23659385650551457, -6.915538690918075382, 49.31353937987644542 ) ) ;
#17113 = CARTESIAN_POINT ( 'NONE',  ( -21.00520398765801744, -21.34214743040633167, 62.37117330845665464 ) ) ;
#17114 = CARTESIAN_POINT ( 'NONE',  ( -14.37682202087475680, -19.38786730597467667, 53.49999999999995026 ) ) ;
#17115 = CARTESIAN_POINT ( 'NONE',  ( -20.81159385650551386, -6.922745924619793101, 51.69366785382590024 ) ) ;
#17116 = CIRCLE ( 'NONE', #47011, 1.949999999999999734 ) ;
#17117 = ORIENTED_EDGE ( 'NONE', *, *, #25568, .F. ) ;
#17118 = CARTESIAN_POINT ( 'NONE',  ( -24.35706328060247827, -15.77560928887050373, 69.53307488759497801 ) ) ;
#17119 = CARTESIAN_POINT ( 'NONE',  ( -24.81734138798520561, -15.73308575106217511, 69.64652101300646336 ) ) ;
#17120 = EDGE_CURVE ( 'NONE', #40267, #23016, #6481, .T. ) ;
#17121 = VERTEX_POINT ( 'NONE', #43431 ) ;
#17122 = CARTESIAN_POINT ( 'NONE',  ( 18.46573386768564973, 1.637040139411225059, 51.75426295951076838 ) ) ;
#17123 = DIRECTION ( 'NONE',  ( 0.000000000000000000, 0.000000000000000000, -1.000000000000000000 ) ) ;
#17124 = DIRECTION ( 'NONE',  ( 0.000000000000000000, 0.000000000000000000, 1.000000000000000000 ) ) ;
#17125 = ORIENTED_EDGE ( 'NONE', *, *, #10775, .T. ) ;
#17126 = AXIS2_PLACEMENT_3D ( 'NONE', #5796, #6269, #36045 ) ;
#17127 = DIRECTION ( 'NONE',  ( 3.549360974554993999E-17, -6.371834667797928663E-18, -1.000000000000000000 ) ) ;
#17128 = AXIS2_PLACEMENT_3D ( 'NONE', #29908, #44940, #44444 ) ;
#17129 = CARTESIAN_POINT ( 'NONE',  ( -16.44703096029287437, -9.650926977002853846, 52.02966884056656482 ) ) ;
#17130 = DIRECTION ( 'NONE',  ( 4.115385489419834196E-17, 0.9999954153791273948, 0.003028072113822188795 ) ) ;
#17131 = VERTEX_POINT ( 'NONE', #28643 ) ;
#17132 = CARTESIAN_POINT ( 'NONE',  ( -20.64396844604977233, -21.02470390210128670, 58.64475165022597025 ) ) ;
#17133 = AXIS2_PLACEMENT_3D ( 'NONE', #41574, #41321, #33417 ) ;
#17134 = CIRCLE ( 'NONE', #12452, 5.249999999999998224 ) ;
#17135 = ORIENTED_EDGE ( 'NONE', *, *, #6617, .T. ) ;
#17136 = CARTESIAN_POINT ( 'NONE',  ( -41.66527032600129132, -14.80920654474423159, 69.07058823529411029 ) ) ;
#17137 = CARTESIAN_POINT ( 'NONE',  ( -15.65212752116712558, -9.867280269464723474, 50.77966884056655772 ) ) ;
#17138 = VERTEX_POINT ( 'NONE', #43675 ) ;
#17139 = CARTESIAN_POINT ( 'NONE',  ( -20.89788161767221197, -20.94431024770144489, 62.39999296070408974 ) ) ;
#17140 = DIRECTION ( 'NONE',  ( -0.9375570856950864451, 0.3478314405900309603, -3.549360974553816870E-17 ) ) ;
#17141 = CARTESIAN_POINT ( 'NONE',  ( -24.22092292145011072, -12.93687797069018153, 66.60246741374322710 ) ) ;
#17142 = ADVANCED_FACE ( 'NONE', ( #9928, #25429 ), #36011, .F. ) ;
#17143 = CARTESIAN_POINT ( 'NONE',  ( -21.17741856139999612, -21.24480563955526691, 65.70737070468148033 ) ) ;
#17144 = VERTEX_POINT ( 'NONE', #32801 ) ;
#17145 = CARTESIAN_POINT ( 'NONE',  ( -21.95938932932862642, -9.477124872050278981, 60.02171213236835712 ) ) ;
#17146 = AXIS2_PLACEMENT_3D ( 'NONE', #33876, #3860, #6576 ) ;
#17147 = EDGE_CURVE ( 'NONE', #23374, #38177, #34516, .T. ) ;
#17148 = CARTESIAN_POINT ( 'NONE',  ( -42.41968209070717677, -14.80920654474416764, 63.03529411764704804 ) ) ;
#17149 = CYLINDRICAL_SURFACE ( 'NONE', #10937, 4.686499999999997002 ) ;
#17150 = ORIENTED_EDGE ( 'NONE', *, *, #1008, .T. ) ;
#17151 = CARTESIAN_POINT ( 'NONE',  ( -10.16422381746084014, -13.13610325312378713, 71.34682038963120476 ) ) ;
#17152 = ADVANCED_FACE ( 'NONE', ( #2765 ), #17773, .T. ) ;
#17153 = FACE_OUTER_BOUND ( 'NONE', #23525, .T. ) ;
#17154 = ORIENTED_EDGE ( 'NONE', *, *, #38869, .F. ) ;
#17155 = ORIENTED_EDGE ( 'NONE', *, *, #17808, .T. ) ;
#17156 = CARTESIAN_POINT ( 'NONE',  ( -14.07539681412750809, -8.605278097683306981, 74.49954655214880006 ) ) ;
#17157 = DIRECTION ( 'NONE',  ( -3.071710424422018668E-17, 6.404604876783312462E-16, 1.000000000000000000 ) ) ;
#17158 = CARTESIAN_POINT ( 'NONE',  ( -11.46044050272623416, -11.04924139602722200, 57.20903212151936401 ) ) ;
#17159 = CARTESIAN_POINT ( 'NONE',  ( -17.23659385650551812, -6.915538690918074494, 49.31353937987644542 ) ) ;
#17160 = LINE ( 'NONE', #20152, #10102 ) ;
#17162 = EDGE_CURVE ( 'NONE', #14223, #24550, #14269, .T. ) ;
#17161 = CARTESIAN_POINT ( 'NONE',  ( -19.38219705895271261, -7.621082839763254846, 60.15367139372862937 ) ) ;
#17163 = CARTESIAN_POINT ( 'NONE',  ( -23.27571566865760033, -18.75553318983527262, 72.90801392080540211 ) ) ;
#17164 = FACE_OUTER_BOUND ( 'NONE', #15365, .T. ) ;
#17165 = ADVANCED_FACE ( 'NONE', ( #25910 ), #19010, .T. ) ;
#17166 = LINE ( 'NONE', #28758, #25317 ) ;
#17167 = EDGE_LOOP ( 'NONE', ( #4746, #46928, #13331, #33627, #17074 ) ) ;
#17168 = ORIENTED_EDGE ( 'NONE', *, *, #23614, .T. ) ;
#17169 = CARTESIAN_POINT ( 'NONE',  ( -22.89456339367424675, -10.36189766663814638, 63.36626189060206826 ) ) ;
#17170 = SHAPE_REPRESENTATION_RELATIONSHIP ( 'NONE' , 'NONE' ,  #5940, #28519 ) ;
#17171 = CARTESIAN_POINT ( 'NONE',  ( -23.64864599473625262, -11.60591425853287539, 66.43831147808981541 ) ) ;
#17172 = VECTOR ( 'NONE', #39456, 1000.000000000000000 ) ;
#17173 = CARTESIAN_POINT ( 'NONE',  ( -6.424093855413058662, -6.859206544744110623, 54.99999999999999289 ) ) ;
#17174 = DIRECTION ( 'NONE',  ( 0.9687793358424821033, -0.2479245821708677133, 0.000000000000000000 ) ) ;
#17175 = CARTESIAN_POINT ( 'NONE',  ( -20.82063550681992226, -21.43998110257799539, 58.90121085131534784 ) ) ;
#17176 = CIRCLE ( 'NONE', #13997, 0.5560000000000009379 ) ;
#17177 = CARTESIAN_POINT ( 'NONE',  ( -21.34284385650552096, -8.811426318492348031, 52.18089403414751359 ) ) ;
#17178 = AXIS2_PLACEMENT_3D ( 'NONE', #46619, #39460, #38726 ) ;
#17179 = ORIENTED_EDGE ( 'NONE', *, *, #46106, .F. ) ;
#17180 = CARTESIAN_POINT ( 'NONE',  ( -20.81696448553514855, -20.93198605141084201, 62.41471400679856885 ) ) ;
#17181 = CARTESIAN_POINT ( 'NONE',  ( -46.47622156840087371, -14.20920654474410760, 70.87000000000000455 ) ) ;
#17182 = FACE_OUTER_BOUND ( 'NONE', #11563, .T. ) ;
#17183 = CARTESIAN_POINT ( 'NONE',  ( -18.20148605613024628, -22.21866286466902451, 65.52249049189786945 ) ) ;
#17184 = VECTOR ( 'NONE', #15630, 1000.000000000000000 ) ;
#17185 =( BOUNDED_SURFACE ( )  B_SPLINE_SURFACE ( 3, 1, ( 
 ( #25918, #22719 ),
 ( #26650, #10896 ),
 ( #14793, #7466 ),
 ( #19016, #40933 ),
 ( #22467, #29610 ),
 ( #15294, #11875 ),
 ( #23207, #4247 ) ),
 .UNSPECIFIED., .T., .F., .F. ) 
 B_SPLINE_SURFACE_WITH_KNOTS ( ( 4, 3, 4 ),
 ( 2, 2 ),
 ( 0.000000000000000000, 0.5000000000000000000, 1.000000000000000000 ),
 ( 0.000000000000000000, 1.000000000000000000 ),
 .UNSPECIFIED. ) 
 GEOMETRIC_REPRESENTATION_ITEM ( )  RATIONAL_B_SPLINE_SURFACE ( (
 ( 1.000000000000000000, 1.000000000000000000),
 ( 0.3333333333333335369, 0.3333333333333330373),
 ( 0.3333333333333335369, 0.3333333333333330373),
 ( 1.000000000000000000, 1.000000000000000000),
 ( 0.3333333333333333703, 0.3333333333333333703),
 ( 0.3333333333333333703, 0.3333333333333333703),
 ( 1.000000000000000000, 1.000000000000000000) ) ) 
 REPRESENTATION_ITEM ( '' )  SURFACE ( )  );
#17186 = ADVANCED_FACE ( 'NONE', ( #21972 ), #3494, .T. ) ;
#17187 = ORIENTED_EDGE ( 'NONE', *, *, #37401, .T. ) ;
#17188 = CARTESIAN_POINT ( 'NONE',  ( -24.40217295060720204, -14.25566147773195524, 69.95275273531336779 ) ) ;
#17189 = FACE_OUTER_BOUND ( 'NONE', #6788, .T. ) ;
#17190 = CARTESIAN_POINT ( 'NONE',  ( 18.62590614458706995, 1.902842057076367777, 48.83032374393989272 ) ) ;
#17191 = B_SPLINE_CURVE_WITH_KNOTS ( 'NONE', 1,
 ( #18318, #8015 ),
 .UNSPECIFIED., .F., .F.,
 ( 2, 2 ),
 ( 0.000000000000000000, 1.000000000000000000 ),
 .UNSPECIFIED. ) ;
#17192 = CARTESIAN_POINT ( 'NONE',  ( -10.45378225047720200, -13.70027870591744446, 74.83384660681542755 ) ) ;
#17193 = CARTESIAN_POINT ( 'NONE',  ( -15.51435322605840739, -21.59577299045269427, 72.34015665073278001 ) ) ;
#17194 = CARTESIAN_POINT ( 'NONE',  ( -23.49746296483011321, -11.32841565874639222, 70.19210718165021490 ) ) ;
#17195 = FACE_OUTER_BOUND ( 'NONE', #22180, .T. ) ;
#17196 = EDGE_LOOP ( 'NONE', ( #32873, #42572, #26582, #6626 ) ) ;
#17197 = EDGE_CURVE ( 'NONE', #11545, #4554, #20771, .T. ) ;
#17198 = DIRECTION ( 'NONE',  ( 3.071710424422018668E-17, -6.404604876783312462E-16, -1.000000000000000000 ) ) ;
#17199 =( BOUNDED_CURVE ( )  B_SPLINE_CURVE ( 3, ( #45182, #19057, #41713, #7754 ),
 .UNSPECIFIED., .F., .F. ) 
 B_SPLINE_CURVE_WITH_KNOTS ( ( 4, 4 ),
 ( 0.000000000000000000, 0.4074455897393635673 ),
 .UNSPECIFIED. ) 
 CURVE ( )  GEOMETRIC_REPRESENTATION_ITEM ( )  RATIONAL_B_SPLINE_CURVE ( ( 1.000000000000000000, 0.4567392136813370196, 0.3561768502900321542, 0.6983129098260854040 ) ) 
 REPRESENTATION_ITEM ( '' )  );
#17200 = ORIENTED_EDGE ( 'NONE', *, *, #20219, .F. ) ;
#17201 = DIRECTION ( 'NONE',  ( 1.261798975490001659E-05, -2.391811517362266964E-06, 0.9999999999175328558 ) ) ;
#17202 = CARTESIAN_POINT ( 'NONE',  ( -19.25563148410905612, -7.587679091002938137, 63.59235773869015418 ) ) ;
#17203 = ORIENTED_EDGE ( 'NONE', *, *, #44963, .T. ) ;
#17204 = CARTESIAN_POINT ( 'NONE',  ( -30.42409385541305156, -25.10920654474410441, 52.99999999999997158 ) ) ;
#17205 = CARTESIAN_POINT ( 'NONE',  ( -14.17409385650551457, -9.792211528768504536, 50.49490371617623197 ) ) ;
#17206 = CIRCLE ( 'NONE', #48685, 0.2499999999999976408 ) ;
#17207 = ORIENTED_EDGE ( 'NONE', *, *, #26850, .F. ) ;
#17208 = CARTESIAN_POINT ( 'NONE',  ( -15.60243201887541709, -21.62804181911354817, 68.73160055118694345 ) ) ;
#17209 = CARTESIAN_POINT ( 'NONE',  ( -20.72574062298286535, -8.580111251864035893, 59.84125250080548142 ) ) ;
#17210 = CARTESIAN_POINT ( 'NONE',  ( 8.575906144586951996, 11.88994474481043184, 50.81056029612154390 ) ) ;
#17211 = ORIENTED_EDGE ( 'NONE', *, *, #9696, .F. ) ;
#17212 = CARTESIAN_POINT ( 'NONE',  ( -23.85493189207092257, -17.57435386044600278, 62.77360986608242399 ) ) ;
#17213 = AXIS2_PLACEMENT_3D ( 'NONE', #28854, #36948, #36468 ) ;
#17214 = VECTOR ( 'NONE', #25242, 1000.000000000000000 ) ;
#17215 = CARTESIAN_POINT ( 'NONE',  ( -27.42409385541305511, -6.359206544744109735, 63.99999999999998579 ) ) ;
#17216 = B_SPLINE_CURVE_WITH_KNOTS ( 'NONE', 1,
 ( #33525, #30608 ),
 .UNSPECIFIED., .F., .F.,
 ( 2, 2 ),
 ( 0.000000000000000000, 1.000000000000000000 ),
 .UNSPECIFIED. ) ;
#17217 = EDGE_CURVE ( 'NONE', #43000, #23813, #44888, .T. ) ;
#17218 = CARTESIAN_POINT ( 'NONE',  ( -11.96893353090061929, -10.42262660427394039, 67.72570221455328010 ) ) ;
#17219 = DIRECTION ( 'NONE',  ( -3.071710424422018668E-17, 6.404604876783312462E-16, 1.000000000000000000 ) ) ;
#17220 = ORIENTED_EDGE ( 'NONE', *, *, #32645, .T. ) ;
#17221 = ORIENTED_EDGE ( 'NONE', *, *, #42356, .T. ) ;
#17222 = EDGE_CURVE ( 'NONE', #27479, #5194, #8298, .T. ) ;
#17223 = DIRECTION ( 'NONE',  ( 3.913797943140854342E-06, 1.965591624649253694E-06, 0.9999999999904093384 ) ) ;
#17224 = CARTESIAN_POINT ( 'NONE',  ( -18.78767905735283605, -20.13749289187802916, 53.49999999999995026 ) ) ;
#17225 = ORIENTED_EDGE ( 'NONE', *, *, #28979, .F. ) ;
#17226 = CARTESIAN_POINT ( 'NONE',  ( -17.65334680565586112, -7.812901805943546663, 60.15348847797940124 ) ) ;
#17227 = CARTESIAN_POINT ( 'NONE',  ( -17.42409385541299471, -14.80920654474435771, 49.52966884056655772 ) ) ;
#17228 = VECTOR ( 'NONE', #19596, 1000.000000000000000 ) ;
#17229 = EDGE_CURVE ( 'NONE', #36010, #41418, #14862, .T. ) ;
#17230 = CARTESIAN_POINT ( 'NONE',  ( -18.67409385759799179, -6.859212275519751323, 50.50378509014259265 ) ) ;
#17231 = CARTESIAN_POINT ( 'NONE',  ( -24.41470909780205290, -15.75055545595021478, 66.06324634287898334 ) ) ;
#17232 = CARTESIAN_POINT ( 'NONE',  ( -24.30048669258562200, -16.36410883687464946, 59.42332431756337741 ) ) ;
#17233 = CARTESIAN_POINT ( 'NONE',  ( -12.34063872187652855, -9.996720073711612642, 60.85918082403506446 ) ) ;
#17234 = ORIENTED_EDGE ( 'NONE', *, *, #1107, .F. ) ;
#17235 = CARTESIAN_POINT ( 'NONE',  ( -43.17409385541305511, -15.80920654474410725, 56.99999999999999289 ) ) ;
#17236 = DIRECTION ( 'NONE',  ( -1.669677910507523245E-21, 1.000000000000000000, -1.084253996632606407E-42 ) ) ;
#17237 = CARTESIAN_POINT ( 'NONE',  ( -24.72694767484942702, -16.28301260341204326, 62.70833288210281609 ) ) ;
#17238 = CARTESIAN_POINT ( 'NONE',  ( -10.78910781157109433, -11.42070086764308812, 67.77897960319765502 ) ) ;
#17239 = ADVANCED_FACE ( 'NONE', ( #3257 ), #18260, .T. ) ;
#17240 = ADVANCED_FACE ( 'NONE', ( #44392 ), #22220, .T. ) ;
#17241 = VERTEX_POINT ( 'NONE', #15289 ) ;
#17242 = ORIENTED_EDGE ( 'NONE', *, *, #29490, .F. ) ;
#17243 = EDGE_CURVE ( 'NONE', #44898, #7311, #48306, .T. ) ;
#17244 = EDGE_CURVE ( 'NONE', #14076, #1460, #42414, .T. ) ;
#17245 = CARTESIAN_POINT ( 'NONE',  ( -22.63008543824757979, -10.12971389395683097, 70.01178520543939499 ) ) ;
#17246 = AXIS2_PLACEMENT_3D ( 'NONE', #11036, #15867, #3641 ) ;
#17247 = CARTESIAN_POINT ( 'NONE',  ( -23.90351025910924321, -11.13227635073321764, 69.99187118439921562 ) ) ;
#17248 = B_SPLINE_CURVE_WITH_KNOTS ( 'NONE', 3,
 ( #36810, #25749, #33355, #15377, #48398, #10731, #30443, #44481, #45456, #40769 ),
 .UNSPECIFIED., .F., .F.,
 ( 4, 2, 2, 2, 4 ),
 ( 0.6272669072877892216, 0.7522669073072935086, 0.8772669073267977957, 1.002266907346302194, 1.127266907365806370 ),
 .UNSPECIFIED. ) ;
#17249 = VERTEX_POINT ( 'NONE', #32550 ) ;
#17250 = VECTOR ( 'NONE', #45787, 1000.000000000000114 ) ;
#17251 = CARTESIAN_POINT ( 'NONE',  ( -16.22269243185835919, -7.456664632783214230, 60.39366801213454750 ) ) ;
#17252 = B_SPLINE_CURVE_WITH_KNOTS ( 'NONE', 3,
 ( #4308, #34321, #31129, #46153, #8976, #1573, #16582, #19315, #45684, #12410 ),
 .UNSPECIFIED., .F., .F.,
 ( 4, 2, 2, 2, 4 ),
 ( 0.1272669073658274641, 0.2522669073463270628, 0.3772669073268266615, 0.5022669073073262602, 0.6272669072878258589 ),
 .UNSPECIFIED. ) ;
#17253 = CARTESIAN_POINT ( 'NONE',  ( -12.87649578556737318, -13.67667219862661021, 49.52966884056655772 ) ) ;
#17254 = ORIENTED_EDGE ( 'NONE', *, *, #38038, .F. ) ;
#17255 = CARTESIAN_POINT ( 'NONE',  ( -20.31649657898477912, -7.943510300654241796, 70.43595776394847974 ) ) ;
#17256 = CARTESIAN_POINT ( 'NONE',  ( -17.91840021365262814, -21.79173196354552644, 62.17535923606572368 ) ) ;
#17257 = EDGE_LOOP ( 'NONE', ( #5699, #28299, #8019, #2621, #11957 ) ) ;
#17258 = CARTESIAN_POINT ( 'NONE',  ( -15.81136650494192963, -7.997455857626498243, 67.15509653266745715 ) ) ;
#17259 = ORIENTED_EDGE ( 'NONE', *, *, #5099, .T. ) ;
#17260 = CYLINDRICAL_SURFACE ( 'NONE', #11009, 0.1500000000000072387 ) ;
#17261 = ORIENTED_EDGE ( 'NONE', *, *, #47663, .T. ) ;
#17262 = CARTESIAN_POINT ( 'NONE',  ( -11.90387715906214439, -19.81242515194113807, 58.08828870480375173 ) ) ;
#17263 = CARTESIAN_POINT ( 'NONE',  ( -23.33186513658400685, -18.65645323816980294, 69.29372015302412535 ) ) ;
#17264 = DIRECTION ( 'NONE',  ( 0.2843796944294933460, 0.9587117342539337450, 5.205739956168972140E-08 ) ) ;
#17265 = VERTEX_POINT ( 'NONE', #47811 ) ;
#17266 = CARTESIAN_POINT ( 'NONE',  ( -13.41013012084913036, -9.008953577314683159, 56.96967469688792818 ) ) ;
#17267 = EDGE_CURVE ( 'NONE', #8655, #40234, #12564, .T. ) ;
#17268 = CARTESIAN_POINT ( 'NONE',  ( -16.97946104448713101, -21.84517140583366057, 72.46543221429990922 ) ) ;
#17269 = VECTOR ( 'NONE', #23607, 1000.000000000000000 ) ;
#17270 = DIRECTION ( 'NONE',  ( -3.071710424422018668E-17, 6.404604876783312462E-16, 1.000000000000000000 ) ) ;
#17271 = CARTESIAN_POINT ( 'NONE',  ( -23.62594491300536959, -11.45603751788689451, 66.70742424642772050 ) ) ;
#17272 = CARTESIAN_POINT ( 'NONE',  ( -19.21526828202639336, -8.042187119094190706, 60.24627617707014338 ) ) ;
#17273 = ORIENTED_EDGE ( 'NONE', *, *, #201, .F. ) ;
#17274 = CARTESIAN_POINT ( 'NONE',  ( -17.45711534482409988, -7.809224652626227225, 63.62345145953160142 ) ) ;
#17275 = PLANE ( 'NONE',  #4584 ) ;
#17276 = DIRECTION ( 'NONE',  ( 9.941263206242173230E-06, 7.040377906907692017E-06, -0.9999999999258021299 ) ) ;
#17277 = CARTESIAN_POINT ( 'NONE',  ( -13.49409790474204840, -20.66256726344224504, 61.53118467422925164 ) ) ;
#17278 = EDGE_CURVE ( 'NONE', #20100, #6805, #46964, .T. ) ;
#17279 = LINE ( 'NONE', #28135, #28349 ) ;
#17280 = CARTESIAN_POINT ( 'NONE',  ( -14.08659385650551776, -9.302874398569244363, 51.68646062012417985 ) ) ;
#17281 = EDGE_LOOP ( 'NONE', ( #43349, #47082, #24845, #34453 ) ) ;
#17282 = ADVANCED_FACE ( 'NONE', ( #21481 ), #46690, .T. ) ;
#17283 = VECTOR ( 'NONE', #20129, 1000.000000000000000 ) ;
#17284 = LINE ( 'NONE', #43902, #48698 ) ;
#17285 = CARTESIAN_POINT ( 'NONE',  ( -10.48067321144888808, -16.03043919553437036, 68.12767830706636119 ) ) ;
#17286 = EDGE_LOOP ( 'NONE', ( #11751, #9748, #20008, #33191, #21072 ) ) ;
#17287 = CARTESIAN_POINT ( 'NONE',  ( -9.974456290884534226, -14.72748455880875795, 71.51278017970571454 ) ) ;
#17288 = DIRECTION ( 'NONE',  ( 2.866981220435666553E-17, -1.000000000000000000, -1.190614954331866791E-16 ) ) ;
#17289 = AXIS2_PLACEMENT_3D ( 'NONE', #2317, #28184, #24973 ) ;
#17290 = CARTESIAN_POINT ( 'NONE',  ( -11.92202137443377907, -10.38855435516889081, 64.18481546414660954 ) ) ;
#17291 = CARTESIAN_POINT ( 'NONE',  ( -16.98991614605047218, -22.24663000551990777, 72.35038637723081933 ) ) ;
#17292 = ORIENTED_EDGE ( 'NONE', *, *, #32254, .T. ) ;
#17293 = CARTESIAN_POINT ( 'NONE',  ( -24.28579947082789303, -13.18942387424446316, 62.84736316175410309 ) ) ;
#17294 = CARTESIAN_POINT ( 'NONE',  ( -17.42409385541299471, -14.80920654474435771, 49.52966884056655772 ) ) ;
#17295 = CARTESIAN_POINT ( 'NONE',  ( -20.85039448910245241, -8.638677133180788559, 63.45554403117525055 ) ) ;
#17296 = ORIENTED_EDGE ( 'NONE', *, *, #44647, .T. ) ;
#17297 = DIRECTION ( 'NONE',  ( -0.9687793358424822143, 0.2479245821708672415, 0.000000000000000000 ) ) ;
#17298 = CARTESIAN_POINT ( 'NONE',  ( -15.68502974777997494, -7.977065180327442384, 70.90989839958919561 ) ) ;
#17299 = VECTOR ( 'NONE', #1077, 1000.000000000000000 ) ;
#17300 = CARTESIAN_POINT ( 'NONE',  ( -13.25427695047628873, -8.635260007732634691, 60.60096827762414051 ) ) ;
#17301 = CARTESIAN_POINT ( 'NONE',  ( -24.59706363142188934, -12.79617847886399140, 66.48742024426742603 ) ) ;
#17302 = CARTESIAN_POINT ( 'NONE',  ( -20.83700022493356130, -19.12221826660257307, 53.49999999999995026 ) ) ;
#17303 = CARTESIAN_POINT ( 'NONE',  ( -11.57411280416560651, -10.96269712432890131, 57.28073583805487345 ) ) ;
#17305 = ORIENTED_EDGE ( 'NONE', *, *, #14379, .T. ) ;
#17304 = ADVANCED_FACE ( 'NONE', ( #33250 ), #43898, .F. ) ;
#17306 = ORIENTED_EDGE ( 'NONE', *, *, #2242, .T. ) ;
#17307 = CARTESIAN_POINT ( 'NONE',  ( -18.75534385541304516, -8.623186033802570094, 49.24843789510466507 ) ) ;
#17308 = ADVANCED_FACE ( 'NONE', ( #10400 ), #39942, .T. ) ;
#17309 = EDGE_CURVE ( 'NONE', #39506, #46704, #3237, .T. ) ;
#17310 = CARTESIAN_POINT ( 'NONE',  ( -10.37541943412130863, -14.96049300415475614, 75.08306784598362071 ) ) ;
#17311 = CARTESIAN_POINT ( 'NONE',  ( -19.04042132780597996, -7.536568533962904048, 67.01576502235467103 ) ) ;
#17312 = EDGE_CURVE ( 'NONE', #1731, #15392, #43721, .T. ) ;
#17313 = ADVANCED_FACE ( 'NONE', ( #17751 ), #33010, .F. ) ;
#17314 = CARTESIAN_POINT ( 'NONE',  ( -20.18941624216641273, -7.891347737435665977, 73.83601159825586535 ) ) ;
#17315 = CARTESIAN_POINT ( 'NONE',  ( -10.40888626530166405, -14.10966241957602563, 60.91821293886854249 ) ) ;
#17316 = ORIENTED_EDGE ( 'NONE', *, *, #32718, .F. ) ;
#17317 = CARTESIAN_POINT ( 'NONE',  ( -21.05203622307093170, -20.79576407825920725, 65.59956342937501006 ) ) ;
#17318 = DIRECTION ( 'NONE',  ( -0.000000000000000000, -1.000000000000000000, -0.000000000000000000 ) ) ;
#17319 = ORIENTED_EDGE ( 'NONE', *, *, #31986, .F. ) ;
#17320 = FACE_OUTER_BOUND ( 'NONE', #29527, .T. ) ;
#17321 = VECTOR ( 'NONE', #19874, 1000.000000000000227 ) ;
#17322 = CARTESIAN_POINT ( 'NONE',  ( -19.30271816048872324, -8.014114901043837946, 60.26092997144682784 ) ) ;
#17323 = ORIENTED_EDGE ( 'NONE', *, *, #32650, .T. ) ;
#17324 = DIRECTION ( 'NONE',  ( 0.09077643883959131410, -0.9958712959773466933, -4.338678766818132329E-08 ) ) ;
#17325 = CARTESIAN_POINT ( 'NONE',  ( -12.16754809903432211, -19.43427161745671228, 58.03755408627969103 ) ) ;
#17326 = EDGE_LOOP ( 'NONE', ( #4838, #25831 ) ) ;
#17327 = LINE ( 'NONE', #9236, #17553 ) ;
#17328 = ADVANCED_FACE ( 'NONE', ( #14521 ), #21709, .T. ) ;
#17329 = CARTESIAN_POINT ( 'NONE',  ( -12.32278866559117780, -19.67576434477648917, 61.41150688479135766 ) ) ;
#17330 = CIRCLE ( 'NONE', #40927, 1.250000000000001110 ) ;
#17331 =( BOUNDED_CURVE ( )  B_SPLINE_CURVE ( 3, ( #17685, #2908, #2443, #9840 ),
 .UNSPECIFIED., .F., .F. ) 
 B_SPLINE_CURVE_WITH_KNOTS ( ( 4, 4 ),
 ( 0.4074455897393622905, 0.5000000000000000000 ),
 .UNSPECIFIED. ) 
 CURVE ( )  GEOMETRIC_REPRESENTATION_ITEM ( )  RATIONAL_B_SPLINE_CURVE ( ( 0.6983129098260907330, 0.7760317562607114139, 0.8765941196520190548, 1.000000000000024203 ) ) 
 REPRESENTATION_ITEM ( '' )  );
#17332 = DIRECTION ( 'NONE',  ( 1.000000000000000000, 0.000000000000000000, 0.000000000000000000 ) ) ;
#17333 = CARTESIAN_POINT ( 'NONE',  ( -11.08737491380029461, -17.78356865475915427, 71.64006328234201249 ) ) ;
#17334 = ORIENTED_EDGE ( 'NONE', *, *, #4473, .T. ) ;
#17335 = DIRECTION ( 'NONE',  ( 0.8547111024021492032, 0.5191039697695417621, 7.472447835916433805E-08 ) ) ;
#17336 = CARTESIAN_POINT ( 'NONE',  ( -26.92409385541305511, -6.859206544744110623, 52.99999999999997158 ) ) ;
#17337 = CARTESIAN_POINT ( 'NONE',  ( -15.40900924028612451, -21.51335189680180804, 72.06192110245186200 ) ) ;
#17338 = CARTESIAN_POINT ( 'NONE',  ( -11.91343944425293522, -19.82283459374304968, 58.04187056893558605 ) ) ;
#17339 = CARTESIAN_POINT ( 'NONE',  ( -17.42409385541299471, -14.80920654474435771, 49.52966884056655772 ) ) ;
#17340 = DIRECTION ( 'NONE',  ( -0.4501286257827957216, -0.8929637284072022840, 1.500157795982635434E-08 ) ) ;
#17341 = EDGE_CURVE ( 'NONE', #260, #15899, #7266, .T. ) ;
#17342 = VECTOR ( 'NONE', #33292, 1000.000000000000000 ) ;
#17343 = DIRECTION ( 'NONE',  ( -0.6105870317843965500, -0.7919491628991826015, 6.540688078712152548E-08 ) ) ;
#17344 = CARTESIAN_POINT ( 'NONE',  ( -23.42597896001542424, -18.52301023162717897, 65.97956265853692059 ) ) ;
#17345 = EDGE_LOOP ( 'NONE', ( #43035, #2056, #20872, #46228, #11528 ) ) ;
#17346 = CARTESIAN_POINT ( 'NONE',  ( -13.84149883539359749, -8.276978603410436008, 74.33808174404438773 ) ) ;
#17347 = CARTESIAN_POINT ( 'NONE',  ( -22.63183829035100914, -15.47396055967929129, 49.52966884056655772 ) ) ;
#17348 = FACE_OUTER_BOUND ( 'NONE', #803, .T. ) ;
#17349 = VERTEX_POINT ( 'NONE', #4453 ) ;
#17350 =( BOUNDED_CURVE ( )  B_SPLINE_CURVE ( 3, ( #4974, #34989, #8910, #46085 ),
 .UNSPECIFIED., .F., .F. ) 
 B_SPLINE_CURVE_WITH_KNOTS ( ( 4, 4 ),
 ( 0.000000000000000000, 0.4074455897393651771 ),
 .UNSPECIFIED. ) 
 CURVE ( )  GEOMETRIC_REPRESENTATION_ITEM ( )  RATIONAL_B_SPLINE_CURVE ( ( 1.000000000000000000, 0.4567392136813375192, 0.3561768502900323208, 0.6983129098260844048 ) ) 
 REPRESENTATION_ITEM ( '' )  );
#17351 = DIRECTION ( 'NONE',  ( -3.071710424422018668E-17, 6.404604876783312462E-16, 1.000000000000000000 ) ) ;
#17352 = CIRCLE ( 'NONE', #14202, 2.499999999999999556 ) ;
#17353 = ORIENTED_EDGE ( 'NONE', *, *, #34557, .F. ) ;
#17354 = ORIENTED_EDGE ( 'NONE', *, *, #10058, .F. ) ;
#17355 = VERTEX_POINT ( 'NONE', #34735 ) ;
#17357 = CARTESIAN_POINT ( 'NONE',  ( -16.13432406759100601, -21.74052631579560568, 58.30057715624173653 ) ) ;
#17356 = AXIS2_PLACEMENT_3D ( 'NONE', #19338, #34347, #15633 ) ;
#17358 = CARTESIAN_POINT ( 'NONE',  ( -23.15062936622491563, -18.83573383206660168, 66.10772932244093170 ) ) ;
#17359 = CYLINDRICAL_SURFACE ( 'NONE', #43258, 0.1499999999999988565 ) ;
#17360 = CARTESIAN_POINT ( 'NONE',  ( -22.27409385759798965, -6.859212275519751323, 50.50378509014259265 ) ) ;
#17361 = CIRCLE ( 'NONE', #33055, 3.982850737850970990 ) ;
#17362 =( BOUNDED_CURVE ( )  B_SPLINE_CURVE ( 3, ( #9898, #42672, #39925, #17009 ),
 .UNSPECIFIED., .F., .F. ) 
 B_SPLINE_CURVE_WITH_KNOTS ( ( 4, 4 ),
 ( 0.9074455897393701731, 1.000000000000000000 ),
 .UNSPECIFIED. ) 
 CURVE ( )  GEOMETRIC_REPRESENTATION_ITEM ( )  RATIONAL_B_SPLINE_CURVE ( ( 0.6983129098261113832, 0.7760317562607140784, 0.8765941196520102840, 1.000000000000000000 ) ) 
 REPRESENTATION_ITEM ( '' )  );
#17363 = ORIENTED_EDGE ( 'NONE', *, *, #26119, .T. ) ;
#17364 = VERTEX_POINT ( 'NONE', #11853 ) ;
#17365 = CARTESIAN_POINT ( 'NONE',  ( -19.46159385650551599, -9.295667164867525756, 49.30633214617472504 ) ) ;
#17366 = ADVANCED_FACE ( 'NONE', ( #7434 ), #34481, .T. ) ;
#17367 = CARTESIAN_POINT ( 'NONE',  ( -11.47236213698566054, -10.32806074475630886, 74.55389686390628867 ) ) ;
#17368 = AXIS2_PLACEMENT_3D ( 'NONE', #11623, #30358, #48562 ) ;
#17369 = LINE ( 'NONE', #32164, #20546 ) ;
#17370 = CARTESIAN_POINT ( 'NONE',  ( -17.38034385650551528, -6.424090610841176385, 49.80797279389977916 ) ) ;
#17371 = B_SPLINE_CURVE_WITH_KNOTS ( 'NONE', 3,
 ( #29915, #37513, #11203, #3809, #30169, #4528, #42210, #19308, #26951, #38011 ),
 .UNSPECIFIED., .F., .F.,
 ( 4, 2, 2, 2, 4 ),
 ( 0.6272669072978946936, 0.7522669073148660068, 0.8772669073318372090, 1.002266907348808411, 1.127266907365779725 ),
 .UNSPECIFIED. ) ;
#17372 = EDGE_CURVE ( 'NONE', #47972, #41967, #41392, .T. ) ;
#17374 = ORIENTED_EDGE ( 'NONE', *, *, #48321, .F. ) ;
#17373 = ADVANCED_FACE ( 'NONE', ( #522 ), #19725, .T. ) ;
#17375 = CARTESIAN_POINT ( 'NONE',  ( -18.12273401612753077, -22.22646211661374593, 65.46036745194116691 ) ) ;
#17376 = EDGE_CURVE ( 'NONE', #34652, #23071, #37432, .T. ) ;
#17377 = CARTESIAN_POINT ( 'NONE',  ( -24.87384330133638599, -14.87999890626018384, 59.35804801245023299 ) ) ;
#17378 = EDGE_CURVE ( 'NONE', #11979, #11700, #4908, .T. ) ;
#17379 = ORIENTED_EDGE ( 'NONE', *, *, #13481, .T. ) ;
#17380 = CARTESIAN_POINT ( 'NONE',  ( -16.87409385759798752, -6.859212275519751323, 50.50378509014259265 ) ) ;
#17381 = ORIENTED_EDGE ( 'NONE', *, *, #5542, .F. ) ;
#17382 = CARTESIAN_POINT ( 'NONE',  ( -22.49805064719525305, -9.986866608920609067, 73.48161091687566682 ) ) ;
#17383 = DIRECTION ( 'NONE',  ( -3.071710424422018668E-17, 6.404604876783312462E-16, 1.000000000000000000 ) ) ;
#17384 = CARTESIAN_POINT ( 'NONE',  ( -18.90223155190902915, -7.506551502853892721, 67.01416387246997886 ) ) ;
#17385 = ADVANCED_FACE ( 'NONE', ( #23420 ), #19468, .T. ) ;
#17386 = AXIS2_PLACEMENT_3D ( 'NONE', #42796, #20139, #39087 ) ;
#17387 = VERTEX_POINT ( 'NONE', #1009 ) ;
#17388 = DIRECTION ( 'NONE',  ( -0.3964226963016471150, -0.9180681052388935948, 0.000000000000000000 ) ) ;
#17389 = FACE_OUTER_BOUND ( 'NONE', #25770, .T. ) ;
#17390 = FACE_OUTER_BOUND ( 'NONE', #10172, .T. ) ;
#17391 = ORIENTED_EDGE ( 'NONE', *, *, #45151, .T. ) ;
#17392 = CARTESIAN_POINT ( 'NONE',  ( -24.83419172831454347, -15.58085240086919576, 73.14157211650798729 ) ) ;
#17393 = AXIS2_PLACEMENT_3D ( 'NONE', #21341, #47917, #29203 ) ;
#17394 = CARTESIAN_POINT ( 'NONE',  ( -24.85911909788007179, -14.32540520456757172, 69.83930567627945152 ) ) ;
#17395 = EDGE_LOOP ( 'NONE', ( #29145, #27853 ) ) ;
#17396 = B_SPLINE_CURVE_WITH_KNOTS ( 'NONE', 3,
 ( #17594, #32627, #2102, #6039, #19008, #59, #11869, #27119, #22714, #42396 ),
 .UNSPECIFIED., .F., .F.,
 ( 4, 2, 2, 2, 4 ),
 ( 0.6272669072877625762, 0.7522669073072669743, 0.8772669073267712614, 1.002266907346275548, 1.127266907365779947 ),
 .UNSPECIFIED. ) ;
#17397 = CARTESIAN_POINT ( 'NONE',  ( -13.86189509728330904, -11.74550036546146004, 49.52966884056655772 ) ) ;
#17398 = CARTESIAN_POINT ( 'NONE',  ( -50.42609385541305755, -14.90920654474424367, 70.07647058823528141 ) ) ;
#17399 = VERTEX_POINT ( 'NONE', #15764 ) ;
#17400 = DIRECTION ( 'NONE',  ( -0.3478314405900308492, -0.9375570856950864451, 0.000000000000000000 ) ) ;
#17401 = CARTESIAN_POINT ( 'NONE',  ( -24.66730449611544529, -13.06573935865489844, 62.94768786448354092 ) ) ;
#17402 = CARTESIAN_POINT ( 'NONE',  ( -16.93941734680483080, -7.775588144984237005, 74.24546186738449194 ) ) ;
#17403 = CARTESIAN_POINT ( 'NONE',  ( -24.03160975973305824, -17.26750547207224784, 69.56339792588553905 ) ) ;
#17404 = ORIENTED_EDGE ( 'NONE', *, *, #27758, .T. ) ;
#17405 = CARTESIAN_POINT ( 'NONE',  ( -21.98930295831539894, -9.502568441585983905, 59.72171225693869445 ) ) ;
#17406 = PRODUCT_DEFINITION_CONTEXT ( 'detailed design', #39771, 'design' ) ;
#17407 = CARTESIAN_POINT ( 'NONE',  ( -19.04042241193164386, -7.536568769452434147, 67.01576393362593365 ) ) ;
#17408 = CARTESIAN_POINT ( 'NONE',  ( -24.35021929840575439, -16.12578517662164401, 62.88768852640185258 ) ) ;
#17409 = EDGE_LOOP ( 'NONE', ( #13323, #20879, #39319, #45434, #22424 ) ) ;
#17410 = CARTESIAN_POINT ( 'NONE',  ( -10.60570718526854961, -17.81143598018131158, 71.68222757358374508 ) ) ;
#17411 = CARTESIAN_POINT ( 'NONE',  ( -24.72409385541305582, -14.90920654474412643, 59.01176470588234224 ) ) ;
#17413 = ORIENTED_EDGE ( 'NONE', *, *, #46969, .T. ) ;
#17412 = CIRCLE ( 'NONE', #4855, 2.000000000000000000 ) ;
#17414 = ORIENTED_EDGE ( 'NONE', *, *, #13758, .T. ) ;
#17415 = CARTESIAN_POINT ( 'NONE',  ( -46.47622156840087371, -14.20920654474410760, 70.56550563755013172 ) ) ;
#17416 = CARTESIAN_POINT ( 'NONE',  ( -19.94733193681641481, -19.41309290135173526, 52.02966884056656482 ) ) ;
#17417 = CARTESIAN_POINT ( 'NONE',  ( -13.33151401730585306, -20.55006798877650454, 58.06122216312902395 ) ) ;
#17418 = CARTESIAN_POINT ( 'NONE',  ( -18.81159385650551741, -6.922745924619793101, 51.69366785382590024 ) ) ;
#17419 = CARTESIAN_POINT ( 'NONE',  ( -45.92409385541306222, -14.20920654474410760, 70.50000000000000000 ) ) ;
#17420 = CARTESIAN_POINT ( 'NONE',  ( -24.72409385541305582, -14.90920654474415663, 62.02941176470587692 ) ) ;
#17421 = ADVANCED_FACE ( 'NONE', ( #44865 ), #30090, .F. ) ;
#17422 = CARTESIAN_POINT ( 'NONE',  ( -21.25790634982353211, -21.19723378012398030, 65.74487280419876356 ) ) ;
#17423 = CARTESIAN_POINT ( 'NONE',  ( -12.23693665947836529, -20.15673230564203422, 65.06663674221491078 ) ) ;
#17424 = CARTESIAN_POINT ( 'NONE',  ( -18.79049830835916524, -7.892586073225762000, 70.38540174208183942 ) ) ;
#17425 = VERTEX_POINT ( 'NONE', #7930 ) ;
#17426 = ORIENTED_EDGE ( 'NONE', *, *, #5394, .F. ) ;
#17428 = CARTESIAN_POINT ( 'NONE',  ( -20.13360759725221882, -21.74902176548401300, 72.55478737390036770 ) ) ;
#17427 = CIRCLE ( 'NONE', #23752, 3.951441697420975618 ) ;
#17429 = EDGE_CURVE ( 'NONE', #16141, #3147, #37939, .T. ) ;
#17430 = AXIS2_PLACEMENT_3D ( 'NONE', #21488, #43662, #17033 ) ;
#17431 = CYLINDRICAL_SURFACE ( 'NONE', #29927, 2.000000000000000000 ) ;
#17432 = DIRECTION ( 'NONE',  ( 0.9629498065864428025, 0.2696806815386155187, -2.751890642837150366E-17 ) ) ;
#17433 = CARTESIAN_POINT ( 'NONE',  ( -11.03124120290388532, -17.66077365132053956, 71.86718193465377169 ) ) ;
#17434 = CARTESIAN_POINT ( 'NONE',  ( -11.05981229291193024, -11.89443034174749769, 71.19746914266430338 ) ) ;
#17435 = B_SPLINE_CURVE_WITH_KNOTS ( 'NONE', 1,
 ( #38717, #43147 ),
 .UNSPECIFIED., .F., .F.,
 ( 2, 2 ),
 ( 0.000000000000000000, 1.000000000000000000 ),
 .UNSPECIFIED. ) ;
#17436 = CARTESIAN_POINT ( 'NONE',  ( -20.66784385650552380, -6.428312510596450480, 51.20221977374900035 ) ) ;
#17437 = ORIENTED_EDGE ( 'NONE', *, *, #39279, .T. ) ;
#17438 = CARTESIAN_POINT ( 'NONE',  ( -20.04849592361258104, -21.35284569240296548, 72.69006679631316103 ) ) ;
#17439 = SURFACE_SIDE_STYLE ('',( #10060 ) ) ;
#17440 = EDGE_CURVE ( 'NONE', #9885, #5635, #41153, .T. ) ;
#17441 = CARTESIAN_POINT ( 'NONE',  ( -14.67111461712440601, -7.886426496449994161, 60.43500955848998757 ) ) ;
#17442 = CARTESIAN_POINT ( 'NONE',  ( -10.10502314809590274, -16.20379097455708006, 68.09112436593052564 ) ) ;
#17443 = CIRCLE ( 'NONE', #24538, 5.249999999999998224 ) ;
#17444 = EDGE_CURVE ( 'NONE', #30955, #10419, #6244, .T. ) ;
#17445 = ORIENTED_EDGE ( 'NONE', *, *, #12111, .T. ) ;
#17446 = EDGE_CURVE ( 'NONE', #43090, #15096, #8582, .T. ) ;
#17447 = CARTESIAN_POINT ( 'NONE',  ( -10.38078069312423679, -14.50222183502507356, 68.00800126083242958 ) ) ;
#17448 = CARTESIAN_POINT ( 'NONE',  ( -20.13271805750754950, -8.299978134201072777, 70.53628287813307907 ) ) ;
#17449 = LINE ( 'NONE', #47500, #2150 ) ;
#17450 = EDGE_CURVE ( 'NONE', #31116, #8437, #3763, .T. ) ;
#17451 = CARTESIAN_POINT ( 'NONE',  ( -8.424093855413094190, -15.80920654474410725, 64.00000000000002842 ) ) ;
#17452 = VERTEX_POINT ( 'NONE', #31530 ) ;
#17453 = CARTESIAN_POINT ( 'NONE',  ( -22.99017014647701984, -19.05426393579631750, 59.18410607220618402 ) ) ;
#17454 = VERTEX_POINT ( 'NONE', #31049 ) ;
#17455 = CARTESIAN_POINT ( 'NONE',  ( -50.42609385541305755, -14.90920654474417972, 64.94117647058821774 ) ) ;
#17456 = CARTESIAN_POINT ( 'NONE',  ( -11.28576306333344625, -19.03127759451936285, 68.37836181605487695 ) ) ;
#17457 = ORIENTED_EDGE ( 'NONE', *, *, #13647, .F. ) ;
#17458 = CARTESIAN_POINT ( 'NONE',  ( -13.71953088125924225, -21.27299755413469384, 68.63341999928891823 ) ) ;
#17459 = CARTESIAN_POINT ( 'NONE',  ( -15.46784385650551918, -6.428312510596451368, 51.20221977374900035 ) ) ;
#17460 = CIRCLE ( 'NONE', #37099, 4.686499999999999666 ) ;
#17461 = VERTEX_POINT ( 'NONE', #39641 ) ;
#17462 = CARTESIAN_POINT ( 'NONE',  ( -18.86498648104808495, -7.957467358499918042, 70.55995216654250157 ) ) ;
#17463 = FACE_OUTER_BOUND ( 'NONE', #9152, .T. ) ;
#17464 = CARTESIAN_POINT ( 'NONE',  ( -41.15852941833841783, -27.10920654474410796, 54.99999999999997868 ) ) ;
#17465 = VERTEX_POINT ( 'NONE', #9130 ) ;
#17466 = CARTESIAN_POINT ( 'NONE',  ( -19.89081357980290932, -21.83916422767060794, 69.07449100745587600 ) ) ;
#17467 = DIRECTION ( 'NONE',  ( -3.071710424422018668E-17, 6.404604876783312462E-16, 1.000000000000000000 ) ) ;
#17468 = CARTESIAN_POINT ( 'NONE',  ( -11.32638108541902788, -11.37148941047682627, 60.78771700233693309 ) ) ;
#17469 = CARTESIAN_POINT ( 'NONE',  ( -20.19231657184298001, -8.325423463105359190, 70.25100341277899929 ) ) ;
#17470 = VERTEX_POINT ( 'NONE', #1739 ) ;
#17471 = EDGE_LOOP ( 'NONE', ( #45350, #20256 ) ) ;
#17472 = CARTESIAN_POINT ( 'NONE',  ( -23.77312771997254615, -18.70709664074277612, 72.87872845841107505 ) ) ;
#17473 = CARTESIAN_POINT ( 'NONE',  ( -13.22529448846758982, -9.145569705956512863, 64.19474388871357462 ) ) ;
#17474 = VERTEX_POINT ( 'NONE', #9374 ) ;
#17475 = DIRECTION ( 'NONE',  ( -3.071710424422018668E-17, 6.404604876783312462E-16, 1.000000000000000000 ) ) ;
#17476 = CARTESIAN_POINT ( 'NONE',  ( -17.21159385759798965, -8.990409506049200417, 49.61344411288074951 ) ) ;
#17477 = CARTESIAN_POINT ( 'NONE',  ( -23.05195072219661512, -10.55808160950470409, 63.48674805708738234 ) ) ;
#17478 = ADVANCED_FACE ( 'NONE', ( #27591 ), #4956, .T. ) ;
#17479 = CARTESIAN_POINT ( 'NONE',  ( -13.89388974506275787, -21.36980381032900667, 72.11102993026078423 ) ) ;
#17480 = CARTESIAN_POINT ( 'NONE',  ( -19.36683724782897897, -21.58655468785150688, 62.00975759738177118 ) ) ;
#17481 = ORIENTED_EDGE ( 'NONE', *, *, #38261, .F. ) ;
#17482 = CARTESIAN_POINT ( 'NONE',  ( -13.07136655094769750, -8.762923122256669473, 64.02451139116674028 ) ) ;
#17483 = CARTESIAN_POINT ( 'NONE',  ( -24.08907074505709645, -11.48026357735065872, 63.13713704106291402 ) ) ;
#17484 = DIRECTION ( 'NONE',  ( -3.071710424422018668E-17, 6.404604876783312462E-16, 1.000000000000000000 ) ) ;
#17485 =( BOUNDED_CURVE ( )  B_SPLINE_CURVE ( 3, ( #9728, #46900, #2078, #43215 ),
 .UNSPECIFIED., .F., .F. ) 
 B_SPLINE_CURVE_WITH_KNOTS ( ( 4, 4 ),
 ( 0.4074455897393639559, 0.5000000000000000000 ),
 .UNSPECIFIED. ) 
 CURVE ( )  GEOMETRIC_REPRESENTATION_ITEM ( )  RATIONAL_B_SPLINE_CURVE ( ( 0.6983129098260867362, 0.7760317562606950936, 0.8765941196520002920, 1.000000000000003775 ) ) 
 REPRESENTATION_ITEM ( '' )  );
#17486 = ORIENTED_EDGE ( 'NONE', *, *, #35171, .F. ) ;
#17487 = ORIENTED_EDGE ( 'NONE', *, *, #20258, .T. ) ;
#17488 = CARTESIAN_POINT ( 'NONE',  ( -24.46435014771442695, -14.30944682264569856, 62.86863794226144364 ) ) ;
#17489 = EDGE_CURVE ( 'NONE', #18401, #35636, #5520, .T. ) ;
#17490 = DIRECTION ( 'NONE',  ( 2.866981220435666553E-17, -1.000000000000000000, -1.190614954331866791E-16 ) ) ;
#17491 = ORIENTED_EDGE ( 'NONE', *, *, #34327, .T. ) ;
#17492 =( BOUNDED_CURVE ( )  B_SPLINE_CURVE ( 3, ( #35032, #16560, #12157, #41957 ),
 .UNSPECIFIED., .F., .F. ) 
 B_SPLINE_CURVE_WITH_KNOTS ( ( 4, 4 ),
 ( 0.000000000000000000, 0.4074455897393675086 ),
 .UNSPECIFIED. ) 
 CURVE ( )  GEOMETRIC_REPRESENTATION_ITEM ( )  RATIONAL_B_SPLINE_CURVE ( ( 1.000000000000000000, 0.4567392136813269721, 0.3561768502900284350, 0.6983129098261046108 ) ) 
 REPRESENTATION_ITEM ( '' )  );
#17493 = CARTESIAN_POINT ( 'NONE',  ( -42.54541738482483026, -14.90920654474415841, 62.02941176470587692 ) ) ;
#17494 = EDGE_CURVE ( 'NONE', #38652, #44500, #18816, .T. ) ;
#17495 = DIRECTION ( 'NONE',  ( 1.000000000000000000, -4.164305804376849172E-17, 1.614929280266638808E-16 ) ) ;
#17496 = ORIENTED_EDGE ( 'NONE', *, *, #6406, .T. ) ;
#17497 = DIRECTION ( 'NONE',  ( 7.166348388238339064E-06, -1.030346078752312232E-05, -0.9999999999212410007 ) ) ;
#17498 = EDGE_CURVE ( 'NONE', #31661, #29406, #3527, .T. ) ;
#17499 = CARTESIAN_POINT ( 'NONE',  ( -17.87922771257724008, -21.79450505577156960, 61.87535931805457778 ) ) ;
#17500 = CARTESIAN_POINT ( 'NONE',  ( -14.98249323814573941, -9.880861343182303358, 54.07175714974879099 ) ) ;
#17501 = ORIENTED_EDGE ( 'NONE', *, *, #15801, .F. ) ;
#17502 = PLANE ( 'NONE',  #32284 ) ;
#17503 = ORIENTED_EDGE ( 'NONE', *, *, #1268, .T. ) ;
#17504 = CARTESIAN_POINT ( 'NONE',  ( 7.325906144586951996, -6.109215713985405749, 50.50605614422795497 ) ) ;
#17505 = CARTESIAN_POINT ( 'NONE',  ( -10.71495605983455590, -12.81234157828920850, 64.26836111193937029 ) ) ;
#17506 = CARTESIAN_POINT ( 'NONE',  ( -17.42539685990596254, -7.755594512365703963, 70.58215807128591734 ) ) ;
#17507 = ORIENTED_EDGE ( 'NONE', *, *, #24884, .F. ) ;
#17508 = CARTESIAN_POINT ( 'NONE',  ( -24.14695329351509656, -18.01973419914282104, 59.18191163003312028 ) ) ;
#17509 = CARTESIAN_POINT ( 'NONE',  ( -10.25351306168449383, -12.78524163461458762, 64.38180785400611228 ) ) ;
#17510 = VECTOR ( 'NONE', #36500, 1000.000000000000227 ) ;
#17511 = CYLINDRICAL_SURFACE ( 'NONE', #31260, 0.1500000000000000222 ) ;
#17512 = EDGE_CURVE ( 'NONE', #27648, #20725, #16729, .T. ) ;
#17513 = CARTESIAN_POINT ( 'NONE',  ( -24.44757306576362410, -14.11227934896924374, 66.33859978849633876 ) ) ;
#17514 = DIRECTION ( 'NONE',  ( 3.071710424422018668E-17, -6.404604876783312462E-16, -1.000000000000000000 ) ) ;
#17515 = CARTESIAN_POINT ( 'NONE',  ( -10.39891438989669226, -17.28914431743334035, 61.26404815609701870 ) ) ;
#17516 = VERTEX_POINT ( 'NONE', #35454 ) ;
#17517 = CARTESIAN_POINT ( 'NONE',  ( -11.46875891826176819, -18.48806303968299858, 61.27710833525312495 ) ) ;
#17518 = ADVANCED_FACE ( 'NONE', ( #16497 ), #46066, .T. ) ;
#17519 = CARTESIAN_POINT ( 'NONE',  ( -11.73157977884637226, -10.00306985186507269, 67.75542791425031908 ) ) ;
#17520 = CARTESIAN_POINT ( 'NONE',  ( -22.97398039646707701, -9.839151245828711367, 70.11204270335640842 ) ) ;
#17521 = B_SPLINE_CURVE_WITH_KNOTS ( 'NONE', 1,
 ( #21030, #1835 ),
 .UNSPECIFIED., .F., .F.,
 ( 2, 2 ),
 ( 0.000000000000000000, 1.000000000000000000 ),
 .UNSPECIFIED. ) ;
#17522 = FACE_OUTER_BOUND ( 'NONE', #40731, .T. ) ;
#17523 = CARTESIAN_POINT ( 'NONE',  ( -18.67686240032185552, -7.922096350451282909, 70.37067976680781101 ) ) ;
#17524 = EDGE_CURVE ( 'NONE', #15882, #21369, #16654, .T. ) ;
#17525 = LINE ( 'NONE', #10151, #27160 ) ;
#17526 = ORIENTED_EDGE ( 'NONE', *, *, #40542, .T. ) ;
#17527 = VERTEX_POINT ( 'NONE', #13273 ) ;
#17528 = CARTESIAN_POINT ( 'NONE',  ( -21.64853795319383067, -9.164858462540919959, 66.95590184911722531 ) ) ;
#17529 = PLANE ( 'NONE',  #40718 ) ;
#17530 = ORIENTED_EDGE ( 'NONE', *, *, #35060, .F. ) ;
#17531 = CARTESIAN_POINT ( 'NONE',  ( -11.33476804054750531, -19.10151225439055978, 68.40184904730287485 ) ) ;
#17533 = CARTESIAN_POINT ( 'NONE',  ( -11.79792781917550570, -18.97409009807959279, 71.68685885149984927 ) ) ;
#17532 = CARTESIAN_POINT ( 'NONE',  ( -10.62793585389281326, -13.13198463278400041, 67.81120344634712183 ) ) ;
#17534 = DIRECTION ( 'NONE',  ( 0.000000000000000000, 0.000000000000000000, 1.000000000000000000 ) ) ;
#17535 = CARTESIAN_POINT ( 'NONE',  ( -18.92409385541303024, -9.359200813967568422, 50.49621490985794026 ) ) ;
#17536 = CARTESIAN_POINT ( 'NONE',  ( -10.42492065060444872, -12.25670954885047692, 57.58503240040955262 ) ) ;
#17537 = VERTEX_POINT ( 'NONE', #46566 ) ;
#17538 = FACE_BOUND ( 'NONE', #25956, .T. ) ;
#17539 = CARTESIAN_POINT ( 'NONE',  ( -10.79572441526863180, -11.40795732096215254, 67.80359905390240272 ) ) ;
#17540 = PLANE ( 'NONE',  #17675 ) ;
#17541 = CARTESIAN_POINT ( 'NONE',  ( -14.80637861323768334, -7.834189837989483429, 57.04274166530056078 ) ) ;
#17542 = ORIENTED_EDGE ( 'NONE', *, *, #3955, .T. ) ;
#17543 = PLANE ( 'NONE',  #32177 ) ;
#17544 = CARTESIAN_POINT ( 'NONE',  ( -11.50962084936622709, -18.55351502409101272, 61.29213219555924042 ) ) ;
#17545 = CARTESIAN_POINT ( 'NONE',  ( -10.40948780249357597, -12.29963818034608813, 57.52846117370101098 ) ) ;
#17546 = CARTESIAN_POINT ( 'NONE',  ( -22.56207008003183745, -19.63703213565221617, 72.92928497383269359 ) ) ;
#17547 = CARTESIAN_POINT ( 'NONE',  ( -15.39389095703113952, -21.97733419268598709, 72.23070866474378704 ) ) ;
#17548 = DIRECTION ( 'NONE',  ( -0.7364384864160969935, 0.6765045127160409510, 1.031360481960658298E-08 ) ) ;
#17549 = ORIENTED_EDGE ( 'NONE', *, *, #45484, .T. ) ;
#17550 = ORIENTED_EDGE ( 'NONE', *, *, #11132, .F. ) ;
#17551 = CARTESIAN_POINT ( 'NONE',  ( -18.36159385541304090, -7.228003583438117552, 51.38655588711986155 ) ) ;
#17552 = CARTESIAN_POINT ( 'NONE',  ( -10.40174263535760524, -17.29725023780839166, 61.34238537770443855 ) ) ;
#17553 = VECTOR ( 'NONE', #20312, 1000.000000000000000 ) ;
#17554 = CYLINDRICAL_SURFACE ( 'NONE', #24499, 1.249999999999998668 ) ;
#17555 = ADVANCED_FACE ( 'NONE', ( #12806, #35685 ), #24147, .F. ) ;
#17556 = CARTESIAN_POINT ( 'NONE',  ( -13.88631413956031579, -11.73554473314221980, 52.02966884056656482 ) ) ;
#17557 = CARTESIAN_POINT ( 'NONE',  ( -10.37873872693602273, -15.23103030436339544, 74.95345861988057834 ) ) ;
#17558 = EDGE_LOOP ( 'NONE', ( #34739, #6193, #35718, #21761 ) ) ;
#17559 = CARTESIAN_POINT ( 'NONE',  ( -11.32522400900782067, -11.27219014254736074, 60.96413645226084554 ) ) ;
#17560 = CARTESIAN_POINT ( 'NONE',  ( -22.07805708657739885, -20.69058616546009333, 53.49999999999994316 ) ) ;
#17561 = VERTEX_POINT ( 'NONE', #28068 ) ;
#17562 = PLANE ( 'NONE',  #43044 ) ;
#17563 = DIRECTION ( 'NONE',  ( -3.071710424422018668E-17, 6.404604876783312462E-16, 1.000000000000000000 ) ) ;
#17564 = ORIENTED_EDGE ( 'NONE', *, *, #9424, .T. ) ;
#17565 = FACE_OUTER_BOUND ( 'NONE', #46796, .T. ) ;
#17566 = CARTESIAN_POINT ( 'NONE',  ( -18.63483346095911131, -21.70376574273382175, 72.35798910450991173 ) ) ;
#17567 = ORIENTED_EDGE ( 'NONE', *, *, #6881, .T. ) ;
#17568 = DIRECTION ( 'NONE',  ( 4.615129112206533859E-07, -1.699487772732772144E-08, 0.9999999999998934186 ) ) ;
#17569 = CARTESIAN_POINT ( 'NONE',  ( -24.83515292193595769, -14.04764123926324082, 73.23776205861604183 ) ) ;
#17570 =( BOUNDED_SURFACE ( )  B_SPLINE_SURFACE ( 3, 1, ( 
 ( #15168, #14919 ),
 ( #44760, #19611 ),
 ( #4128, #26035 ),
 ( #7335, #33633 ),
 ( #48673, #29976 ),
 ( #34134, #33898 ),
 ( #426, #15406 ) ),
 .UNSPECIFIED., .T., .F., .F. ) 
 B_SPLINE_SURFACE_WITH_KNOTS ( ( 4, 3, 4 ),
 ( 2, 2 ),
 ( 0.000000000000000000, 0.5000000000000000000, 1.000000000000000000 ),
 ( 0.000000000000000000, 1.000000000000000000 ),
 .UNSPECIFIED. ) 
 GEOMETRIC_REPRESENTATION_ITEM ( )  RATIONAL_B_SPLINE_SURFACE ( (
 ( 1.000000000000000000, 1.000000000000000000),
 ( 0.3333333333333335369, 0.3333333333333330373),
 ( 0.3333333333333335369, 0.3333333333333330373),
 ( 1.000000000000000000, 1.000000000000000000),
 ( 0.3333333333333333703, 0.3333333333333333703),
 ( 0.3333333333333333703, 0.3333333333333333703),
 ( 1.000000000000000000, 1.000000000000000000) ) ) 
 REPRESENTATION_ITEM ( '' )  SURFACE ( )  );
#17571 = CARTESIAN_POINT ( 'NONE',  ( -21.73099075187129614, -8.730192115828774746, 70.31627817507801126 ) ) ;
#17572 = CYLINDRICAL_SURFACE ( 'NONE', #26043, 1.999999999999999112 ) ;
#17573 = ORIENTED_EDGE ( 'NONE', *, *, #29317, .F. ) ;
#17574 = DIRECTION ( 'NONE',  ( 3.549360974551883545E-17, -6.371834667872732552E-18, -1.000000000000000000 ) ) ;
#17575 = DIRECTION ( 'NONE',  ( 0.9862050927915948506, 0.1655279884246635136, 7.765682856207885122E-08 ) ) ;
#17576 = EDGE_CURVE ( 'NONE', #17705, #2492, #45454, .T. ) ;
#17577 = CARTESIAN_POINT ( 'NONE',  ( -11.96073139429061527, -19.87431630704028152, 57.97036459255868124 ) ) ;
#17578 = ADVANCED_FACE ( 'NONE', ( #24639 ), #16969, .T. ) ;
#17579 = EDGE_CURVE ( 'NONE', #6698, #8929, #13293, .T. ) ;
#17580 = DIRECTION ( 'NONE',  ( -3.071710424422018668E-17, 6.404604876783312462E-16, 1.000000000000000000 ) ) ;
#17581 = CARTESIAN_POINT ( 'NONE',  ( -21.79284385650551670, -7.406986770994972602, 48.81910596585309747 ) ) ;
#17582 = CIRCLE ( 'NONE', #15189, 7.000000000000000888 ) ;
#17583 = CARTESIAN_POINT ( 'NONE',  ( -21.65914559189701194, -18.31838547852702348, 53.49999999999995026 ) ) ;
#17584 = CARTESIAN_POINT ( 'NONE',  ( -23.27284462870851911, -18.74605969774991010, 66.10917289053097079 ) ) ;
#17585 = ORIENTED_EDGE ( 'NONE', *, *, #36867, .T. ) ;
#17586 = CARTESIAN_POINT ( 'NONE',  ( -23.46260370332431577, -11.17067683354235719, 73.66193301755811262 ) ) ;
#17587 = CARTESIAN_POINT ( 'NONE',  ( -24.16515061560491162, -17.98105989040287866, 59.15378417205010209 ) ) ;
#17588 = CARTESIAN_POINT ( 'NONE',  ( -24.08318141890305597, -17.12462156339858055, 72.88895803463330481 ) ) ;
#17589 = ORIENTED_EDGE ( 'NONE', *, *, #27685, .T. ) ;
#17590 = DIRECTION ( 'NONE',  ( 0.000000000000000000, 1.000000000000000000, 0.000000000000000000 ) ) ;
#17591 = EDGE_LOOP ( 'NONE', ( #33456, #7710 ) ) ;
#17592 = VERTEX_POINT ( 'NONE', #21890 ) ;
#17593 = ORIENTED_EDGE ( 'NONE', *, *, #35262, .F. ) ;
#17594 = CARTESIAN_POINT ( 'NONE',  ( -10.03035368457962662, -15.72374687363213575, 61.22284448286259817 ) ) ;
#17595 = DIRECTION ( 'NONE',  ( 1.224646799147353207E-16, 1.000000000000000000, -1.912410701131276611E-32 ) ) ;
#17596 = DIRECTION ( 'NONE',  ( -3.071710424422018668E-17, 6.404604876783312462E-16, 1.000000000000000000 ) ) ;
#17597 = DIRECTION ( 'NONE',  ( 0.000000000000000000, -1.000000000000000000, 0.000000000000000000 ) ) ;
#17598 = ORIENTED_EDGE ( 'NONE', *, *, #46372, .T. ) ;
#17599 = ORIENTED_EDGE ( 'NONE', *, *, #33455, .F. ) ;
#17600 = CARTESIAN_POINT ( 'NONE',  ( -17.71784385650551741, -9.790100578890868377, 49.79778022625163203 ) ) ;
#17601 = EDGE_CURVE ( 'NONE', #17102, #1741, #17935, .T. ) ;
#17602 = FACE_OUTER_BOUND ( 'NONE', #19121, .T. ) ;
#17603 = DIRECTION ( 'NONE',  ( 0.8547111024021490921, 0.5191039697695417621, 7.472447835916433805E-08 ) ) ;
#17604 = CARTESIAN_POINT ( 'NONE',  ( -20.08034385650552167, -6.424090610841176385, 49.80797279389977916 ) ) ;
#17605 = VECTOR ( 'NONE', #22214, 1000.000000000000000 ) ;
#17606 = EDGE_LOOP ( 'NONE', ( #2016, #38814, #16001, #27538, #33628 ) ) ;
#17607 = B_SPLINE_CURVE_WITH_KNOTS ( 'NONE', 3,
 ( #22450, #10876, #26149, #41160, #33256, #18002, #3734, #18744, #25646, #21716 ),
 .UNSPECIFIED., .F., .F.,
 ( 4, 2, 2, 2, 4 ),
 ( 0.6272669072877946617, 0.7522669073073083856, 0.8772669073268219986, 1.002266907346335723, 1.127266907365849447 ),
 .UNSPECIFIED. ) ;
#17608 = EDGE_CURVE ( 'NONE', #14795, #12703, #30199, .T. ) ;
#17609 = DIRECTION ( 'NONE',  ( 0.9375570856950865561, -0.3478314405900308492, 0.000000000000000000 ) ) ;
#17610 = EDGE_CURVE ( 'NONE', #18615, #28180, #25352, .T. ) ;
#17611 = DIRECTION ( 'NONE',  ( 0.4599824152910792496, 0.8879280250239794947, 2.250728352126283681E-08 ) ) ;
#17612 =( BOUNDED_CURVE ( )  B_SPLINE_CURVE ( 3, ( #22258, #26200, #25701, #29402 ),
 .UNSPECIFIED., .F., .F. ) 
 B_SPLINE_CURVE_WITH_KNOTS ( ( 4, 4 ),
 ( 0.000000000000000000, 0.4074455897393676196 ),
 .UNSPECIFIED. ) 
 CURVE ( )  GEOMETRIC_REPRESENTATION_ITEM ( )  RATIONAL_B_SPLINE_CURVE ( ( 1.000000000000000000, 0.4567392136813364090, 0.3561768502900319322, 0.6983129098260865142 ) ) 
 REPRESENTATION_ITEM ( '' )  );
#17613 = ORIENTED_EDGE ( 'NONE', *, *, #39896, .T. ) ;
#17614 = LINE ( 'NONE', #28715, #36672 ) ;
#17615 = ORIENTED_EDGE ( 'NONE', *, *, #16638, .F. ) ;
#17616 = B_SPLINE_CURVE_WITH_KNOTS ( 'NONE', 3,
 ( #47472, #27778, #42807, #34308, #37767, #30654, #29911, #11199, #3551, #10039 ),
 .UNSPECIFIED., .F., .F.,
 ( 4, 2, 2, 2, 4 ),
 ( 0.000000000000000000, 0.2500000000000000000, 0.5000000000000000000, 0.7500000000000000000, 1.000000000000000000 ),
 .UNSPECIFIED. ) ;
#17617 = CARTESIAN_POINT ( 'NONE',  ( -10.70532053225239544, -12.67267096592666498, 61.08381491717225487 ) ) ;
#17618 = CARTESIAN_POINT ( 'NONE',  ( -23.81024829756716343, -18.64597716098235836, 72.94863620959463901 ) ) ;
#17619 = DIRECTION ( 'NONE',  ( -3.071710424422018668E-17, 6.404604876783312462E-16, 1.000000000000000000 ) ) ;
#17620 = VERTEX_POINT ( 'NONE', #7132 ) ;
#17621 = FACE_OUTER_BOUND ( 'NONE', #36554, .T. ) ;
#17622 = CARTESIAN_POINT ( 'NONE',  ( -17.94839601134439633, -19.47832453368858552, 49.52966884056656482 ) ) ;
#17623 = EDGE_LOOP ( 'NONE', ( #33089, #39926, #9080, #27133 ) ) ;
#17624 = CARTESIAN_POINT ( 'NONE',  ( -24.83263378688676326, -15.59489965655864374, 73.18799144572807336 ) ) ;
#17625 =( BOUNDED_CURVE ( )  B_SPLINE_CURVE ( 3, ( #1492, #16506, #24401, #5920 ),
 .UNSPECIFIED., .F., .F. ) 
 B_SPLINE_CURVE_WITH_KNOTS ( ( 4, 4 ),
 ( 0.000000000000000000, 0.4074455897393596260 ),
 .UNSPECIFIED. ) 
 CURVE ( )  GEOMETRIC_REPRESENTATION_ITEM ( )  RATIONAL_B_SPLINE_CURVE ( ( 1.000000000000000000, 0.4567392136813444026, 0.3561768502900348743, 0.6983129098260714152 ) ) 
 REPRESENTATION_ITEM ( '' )  );
#17626 = CARTESIAN_POINT ( 'NONE',  ( -13.27770465421436796, -9.107456272842561873, 64.20946529204060482 ) ) ;
#17627 = ORIENTED_EDGE ( 'NONE', *, *, #5059, .F. ) ;
#17628 = FACE_OUTER_BOUND ( 'NONE', #48731, .T. ) ;
#17629 = FACE_OUTER_BOUND ( 'NONE', #12867, .T. ) ;
#17630 = VERTEX_POINT ( 'NONE', #44088 ) ;
#17631 = ADVANCED_FACE ( 'NONE', ( #10089 ), #37131, .T. ) ;
#17632 = EDGE_CURVE ( 'NONE', #9114, #22244, #29287, .T. ) ;
#17633 = CARTESIAN_POINT ( 'NONE',  ( -11.02242957576233451, -11.85532881267382166, 74.57312195644870201 ) ) ;
#17634 = CARTESIAN_POINT ( 'NONE',  ( -12.91230480768039790, -16.07689808402359333, 52.02966884056656482 ) ) ;
#17635 = CARTESIAN_POINT ( 'NONE',  ( -24.03161744405940325, -17.27608056677072312, 73.29824685711943744 ) ) ;
#17636 = B_SPLINE_CURVE_WITH_KNOTS ( 'NONE', 3,
 ( #46949, #47202, #17858, #9295, #20853, #39322, #9782, #16895, #40054, #1895 ),
 .UNSPECIFIED., .F., .F.,
 ( 4, 2, 2, 2, 4 ),
 ( 0.000000000000000000, 0.2500000000000000000, 0.5000000000000000000, 0.7500000000000000000, 1.000000000000000000 ),
 .UNSPECIFIED. ) ;
#17637 = LINE ( 'NONE', #6577, #24314 ) ;
#17638 = EDGE_LOOP ( 'NONE', ( #30983, #22540 ) ) ;
#17639 = DIRECTION ( 'NONE',  ( -0.000000000000000000, -0.000000000000000000, 1.000000000000000000 ) ) ;
#17640 = LINE ( 'NONE', #25524, #36061 ) ;
#17641 = CARTESIAN_POINT ( 'NONE',  ( -21.55304606329672623, -8.607909972211214011, 73.72315957790283392 ) ) ;
#17642 = ORIENTED_EDGE ( 'NONE', *, *, #21206, .F. ) ;
#17643 = CARTESIAN_POINT ( 'NONE',  ( -10.39538363539702104, -14.16717768424945412, 68.00232930279112509 ) ) ;
#17644 =( BOUNDED_SURFACE ( )  B_SPLINE_SURFACE ( 3, 1, ( 
 ( #33774, #3262 ),
 ( #23376, #19686 ),
 ( #21978, #33272 ),
 ( #12288, #8610 ),
 ( #27309, #10894 ),
 ( #25917, #10656 ),
 ( #11145, #36974 ) ),
 .UNSPECIFIED., .T., .F., .F. ) 
 B_SPLINE_SURFACE_WITH_KNOTS ( ( 4, 3, 4 ),
 ( 2, 2 ),
 ( 0.000000000000000000, 0.5000000000000000000, 1.000000000000000000 ),
 ( 0.000000000000000000, 1.000000000000000000 ),
 .UNSPECIFIED. ) 
 GEOMETRIC_REPRESENTATION_ITEM ( )  RATIONAL_B_SPLINE_SURFACE ( (
 ( 1.000000000000000000, 1.000000000000000000),
 ( 0.3333333333333335369, 0.3333333333333330373),
 ( 0.3333333333333335369, 0.3333333333333330373),
 ( 1.000000000000000000, 1.000000000000000000),
 ( 0.3333333333333333703, 0.3333333333333333703),
 ( 0.3333333333333333703, 0.3333333333333333703),
 ( 1.000000000000000000, 1.000000000000000000) ) ) 
 REPRESENTATION_ITEM ( '' )  SURFACE ( )  );
#17645 = EDGE_CURVE ( 'NONE', #918, #38805, #6632, .T. ) ;
#17646 = ADVANCED_FACE ( 'NONE', ( #6637 ), #21653, .T. ) ;
#17647 = CARTESIAN_POINT ( 'NONE',  ( -24.22122181710478017, -12.92668648255967234, 62.71775301689540782 ) ) ;
#17648 = CIRCLE ( 'NONE', #45203, 0.5560000000000009379 ) ;
#17649 = EDGE_LOOP ( 'NONE', ( #34463, #711 ) ) ;
#17650 = VERTEX_POINT ( 'NONE', #36643 ) ;
#17651 = EDGE_CURVE ( 'NONE', #45860, #42513, #18845, .T. ) ;
#17652 = CARTESIAN_POINT ( 'NONE',  ( -14.87409385541153917, -6.859212275519794844, 50.50378509015643402 ) ) ;
#17653 = CARTESIAN_POINT ( 'NONE',  ( -13.65948078749761585, -20.77935321253323053, 58.20216925893738846 ) ) ;
#17654 = EDGE_CURVE ( 'NONE', #42072, #20668, #10164, .T. ) ;
#17655 = CARTESIAN_POINT ( 'NONE',  ( -10.56409641782382813, -13.17052685802803680, 75.09306420679733662 ) ) ;
#17656 = CARTESIAN_POINT ( 'NONE',  ( -19.44376929052122449, -7.638105555415076076, 60.07597592072836790 ) ) ;
#17657 = CARTESIAN_POINT ( 'NONE',  ( -14.94536187920032333, -8.261047438867105797, 60.50923257244761544 ) ) ;
#17658 = CARTESIAN_POINT ( 'NONE',  ( -12.40319033546273531, -19.76959921888892424, 68.48090162751329046 ) ) ;
#17659 = FACE_OUTER_BOUND ( 'NONE', #412, .T. ) ;
#17660 = EDGE_LOOP ( 'NONE', ( #9639, #14887, #37465, #32060, #8098 ) ) ;
#17661 = ORIENTED_EDGE ( 'NONE', *, *, #47603, .T. ) ;
#17662 = CARTESIAN_POINT ( 'NONE',  ( -10.43098718212803000, -15.70539730037032911, 61.32316937334011442 ) ) ;
#17663 = EDGE_CURVE ( 'NONE', #39613, #5898, #24966, .T. ) ;
#17664 = DIRECTION ( 'NONE',  ( -0.05957303659011965041, -0.9982239494779875377, 2.515684304538401650E-08 ) ) ;
#17665 = CARTESIAN_POINT ( 'NONE',  ( -14.54176566789882585, -21.67913831930545854, 58.28122448549703449 ) ) ;
#17666 = FACE_OUTER_BOUND ( 'NONE', #42382, .T. ) ;
#17667 = CARTESIAN_POINT ( 'NONE',  ( -45.55409385541305767, -16.70920654474410938, 70.50000000000000000 ) ) ;
#17668 = CARTESIAN_POINT ( 'NONE',  ( -18.92409385650551812, -6.426201560718813433, 50.50509628382439331 ) ) ;
#17669 = ORIENTED_EDGE ( 'NONE', *, *, #25101, .F. ) ;
#17670 = CARTESIAN_POINT ( 'NONE',  ( -14.73375663737576247, -21.75657035701089370, 61.75105113489106401 ) ) ;
#17671 = CARTESIAN_POINT ( 'NONE',  ( -19.94550508065608341, -21.39305643010487756, 72.41038500746213913 ) ) ;
#17672 = CARTESIAN_POINT ( 'NONE',  ( -14.66963140629840190, -7.887024584555132556, 60.57642187187276051 ) ) ;
#17673 = CARTESIAN_POINT ( 'NONE',  ( -10.08052694344373812, -16.06451652471636748, 68.09272548404199199 ) ) ;
#17674 = EDGE_LOOP ( 'NONE', ( #46743, #10199, #6630, #35741 ) ) ;
#17675 = AXIS2_PLACEMENT_3D ( 'NONE', #40435, #21499, #29852 ) ;
#17676 = FACE_OUTER_BOUND ( 'NONE', #32913, .T. ) ;
#17677 = CARTESIAN_POINT ( 'NONE',  ( -12.73449705190429881, -9.612314979486423994, 74.51026123490949260 ) ) ;
#17678 = AXIS2_PLACEMENT_3D ( 'NONE', #7806, #22821, #34116 ) ;
#17679 = CYLINDRICAL_SURFACE ( 'NONE', #8450, 2.000000000000001332 ) ;
#17680 = EDGE_CURVE ( 'NONE', #37170, #5421, #3145, .T. ) ;
#17681 = PLANE ( 'NONE',  #39313 ) ;
#17682 = ORIENTED_EDGE ( 'NONE', *, *, #17076, .F. ) ;
#17683 = CARTESIAN_POINT ( 'NONE',  ( -17.42409385541299471, -14.80920654474435594, 52.02966884056656482 ) ) ;
#17684 = ORIENTED_EDGE ( 'NONE', *, *, #31504, .F. ) ;
#17685 = CARTESIAN_POINT ( 'NONE',  ( -24.37683822056718697, -15.97618770311995640, 66.06324926631656069 ) ) ;
#17686 = CARTESIAN_POINT ( 'NONE',  ( -11.29385027892729987, -19.04286830487734861, 68.33194243210506613 ) ) ;
#17687 = ORIENTED_EDGE ( 'NONE', *, *, #44169, .T. ) ;
#17688 = EDGE_CURVE ( 'NONE', #7043, #43099, #12036, .T. ) ;
#17689 = CARTESIAN_POINT ( 'NONE',  ( -13.69271718318762154, -21.25742183927064488, 68.55601500167955464 ) ) ;
#17690 = CARTESIAN_POINT ( 'NONE',  ( -13.22466687598806523, -9.790356633151166221, 49.88233999786937289 ) ) ;
#17691 = VERTEX_POINT ( 'NONE', #41096 ) ;
#17692 = LINE ( 'NONE', #7619, #21320 ) ;
#17693 = LINE ( 'NONE', #36636, #4707 ) ;
#17694 = CARTESIAN_POINT ( 'NONE',  ( -23.92640620196626600, -11.17277965375445703, 70.14856683682155847 ) ) ;
#17695 = VERTEX_POINT ( 'NONE', #8344 ) ;
#17696 = CARTESIAN_POINT ( 'NONE',  ( -13.46596743574567867, -21.12091133008686938, 65.10912019092907599 ) ) ;
#17697 = CARTESIAN_POINT ( 'NONE',  ( -24.22177629109872399, -13.13842424187848934, 63.13264177643409880 ) ) ;
#17698 = CARTESIAN_POINT ( 'NONE',  ( -11.40127056704611519, -11.24191079892443135, 60.67885781060143557 ) ) ;
#17699 = DIRECTION ( 'NONE',  ( 7.381188785182666071E-06, 5.670466977913946987E-06, 0.9999999999566818731 ) ) ;
#17700 = EDGE_LOOP ( 'NONE', ( #23645, #13269, #42321, #31472 ) ) ;
#17701 = ORIENTED_EDGE ( 'NONE', *, *, #34000, .T. ) ;
#17702 = EDGE_CURVE ( 'NONE', #2342, #6917, #21205, .T. ) ;
#17703 = CARTESIAN_POINT ( 'NONE',  ( -23.38832489838272011, -10.34464890867069542, 59.78016211506488986 ) ) ;
#17704 = CARTESIAN_POINT ( 'NONE',  ( -17.00708550189658652, -7.821638742870105965, 73.96018273346899718 ) ) ;
#17705 = VERTEX_POINT ( 'NONE', #44808 ) ;
#17706 = CARTESIAN_POINT ( 'NONE',  ( -11.43603398054886711, -11.08795246958514547, 57.50343388809581313 ) ) ;
#17707 = CARTESIAN_POINT ( 'NONE',  ( -17.83034385759799179, -6.857644439848013640, 49.98602051094139398 ) ) ;
#17708 = EDGE_CURVE ( 'NONE', #46221, #14849, #40347, .T. ) ;
#17709 = CARTESIAN_POINT ( 'NONE',  ( -13.95528965362524332, -21.40322351219866093, 72.03952346373179694 ) ) ;
#17710 = CARTESIAN_POINT ( 'NONE',  ( -19.21257558972570223, -21.63231285022588679, 62.08683831298252898 ) ) ;
#17711 = CIRCLE ( 'NONE', #36569, 2.000000000000001776 ) ;
#17712 = VERTEX_POINT ( 'NONE', #37884 ) ;
#17713 = DIRECTION ( 'NONE',  ( 0.9968684284758858594, -0.07907803935364897396, 1.831731161803828584E-08 ) ) ;
#17714 =( NAMED_UNIT ( * ) SI_UNIT ( $, .STERADIAN. ) SOLID_ANGLE_UNIT ( ) );
#17715 = PLANE ( 'NONE',  #28767 ) ;
#17716 = DIRECTION ( 'NONE',  ( -3.071710424422018668E-17, 6.404604876783312462E-16, 1.000000000000000000 ) ) ;
#17717 = ADVANCED_FACE ( 'NONE', ( #7379 ), #45540, .F. ) ;
#17718 = EDGE_LOOP ( 'NONE', ( #42381, #40308 ) ) ;
#17719 = ORIENTED_EDGE ( 'NONE', *, *, #36326, .T. ) ;
#17720 = CARTESIAN_POINT ( 'NONE',  ( -20.66572514793045912, -8.604890110293021976, 59.84125219026921627 ) ) ;
#17721 = CARTESIAN_POINT ( 'NONE',  ( -12.34589673948493171, -19.70464915359104907, 64.95854842562067688 ) ) ;
#17722 = CARTESIAN_POINT ( 'NONE',  ( -10.72552571836178181, -12.61109718544098790, 60.79853568372239891 ) ) ;
#17723 = CARTESIAN_POINT ( 'NONE',  ( -15.21159385541304587, -8.990409506049200417, 49.61344411288074951 ) ) ;
#17724 = ORIENTED_EDGE ( 'NONE', *, *, #9077, .F. ) ;
#17725 = B_SPLINE_CURVE_WITH_KNOTS ( 'NONE', 3,
 ( #21458, #21926, #2723, #17729, #13311, #40630, #43390, #36212, #21215, #17971 ),
 .UNSPECIFIED., .F., .F.,
 ( 4, 2, 2, 2, 4 ),
 ( 0.6272669072877782304, 0.7522669073072908441, 0.8772669073268035689, 1.002266907346316183, 1.127266907365828796 ),
 .UNSPECIFIED. ) ;
#17726 = CARTESIAN_POINT ( 'NONE',  ( -24.23259748711979356, -13.18308280478570005, 59.55370993033776728 ) ) ;
#17727 = CARTESIAN_POINT ( 'NONE',  ( -12.56076107774658723, -9.694232635630330108, 74.47489936300191005 ) ) ;
#17728 = ORIENTED_EDGE ( 'NONE', *, *, #3332, .T. ) ;
#17729 = CARTESIAN_POINT ( 'NONE',  ( -12.57238404326915315, -20.46304599113934941, 71.94507178006293202 ) ) ;
#17730 = CARTESIAN_POINT ( 'NONE',  ( -21.96079975839714038, -8.899669644523443779, 66.83962766284624024 ) ) ;
#17731 = EDGE_CURVE ( 'NONE', #30525, #46554, #45394, .T. ) ;
#17732 = ORIENTED_EDGE ( 'NONE', *, *, #28119, .T. ) ;
#17733 = DIRECTION ( 'NONE',  ( 0.3688590060343601706, -0.9294853595766551235, 1.901466464867618399E-17 ) ) ;
#17734 = CIRCLE ( 'NONE', #16968, 4.686499999999998778 ) ;
#17735 = ORIENTED_EDGE ( 'NONE', *, *, #18378, .T. ) ;
#17736 = LINE ( 'NONE', #32765, #25264 ) ;
#17737 = CARTESIAN_POINT ( 'NONE',  ( -22.87929373774275632, -19.88409160966729772, 72.75745300618787326 ) ) ;
#17738 = CARTESIAN_POINT ( 'NONE',  ( -19.35628891158445342, -21.53731772049657067, 58.75180642434932565 ) ) ;
#17739 = ORIENTED_EDGE ( 'NONE', *, *, #42119, .F. ) ;
#17740 = CARTESIAN_POINT ( 'NONE',  ( -24.14391077536845032, -18.02620038539897962, 59.16524916619123786 ) ) ;
#17741 = CARTESIAN_POINT ( 'NONE',  ( -10.76270079184834749, -12.47665168726528506, 64.41269048358307714 ) ) ;
#17742 = CARTESIAN_POINT ( 'NONE',  ( -23.00534385650551172, -8.801233750844183135, 48.81488406609782515 ) ) ;
#17743 = CARTESIAN_POINT ( 'NONE',  ( -10.56816478614453381, -13.15098976910933537, 74.76997804572182815 ) ) ;
#17744 = CARTESIAN_POINT ( 'NONE',  ( -11.89179040387956832, -10.43929601004734486, 70.96893105543333036 ) ) ;
#17745 = FACE_OUTER_BOUND ( 'NONE', #41232, .T. ) ;
#17746 = VERTEX_POINT ( 'NONE', #14705 ) ;
#17747 = CARTESIAN_POINT ( 'NONE',  ( -16.90444465785252959, -22.24122871430926196, 72.32689728778339600 ) ) ;
#17748 = CARTESIAN_POINT ( 'NONE',  ( -11.25989573505624364, -11.38792594226331012, 64.14882039369129529 ) ) ;
#17749 = CARTESIAN_POINT ( 'NONE',  ( -22.64102959707144791, -20.12774700627143076, 69.28143819862634700 ) ) ;
#17750 = CARTESIAN_POINT ( 'NONE',  ( -10.40277079310570052, -15.44444055846370745, 57.71792809063055785 ) ) ;
#17751 = FACE_OUTER_BOUND ( 'NONE', #5106, .T. ) ;
#17752 = CARTESIAN_POINT ( 'NONE',  ( -16.07865109465781117, -7.939724484389961034, 63.97011030347106697 ) ) ;
#17753 = ORIENTED_EDGE ( 'NONE', *, *, #16821, .F. ) ;
#17754 = VERTEX_POINT ( 'NONE', #29776 ) ;
#17755 = EDGE_CURVE ( 'NONE', #34024, #22189, #1672, .T. ) ;
#17756 = CARTESIAN_POINT ( 'NONE',  ( -19.09949158415725634, -8.012660229328147921, 63.43089235425713923 ) ) ;
#17757 = CARTESIAN_POINT ( 'NONE',  ( -19.42896615819153538, -21.56812558881098241, 62.14503644571260565 ) ) ;
#17758 = EDGE_LOOP ( 'NONE', ( #10567, #2074, #40116, #16200, #34489 ) ) ;
#17760 = CARTESIAN_POINT ( 'NONE',  ( -14.37682202087475680, -19.38786730597468022, 54.07175714974878389 ) ) ;
#17759 = DIRECTION ( 'NONE',  ( 3.071710424422018668E-17, -6.404604876783312462E-16, -1.000000000000000000 ) ) ;
#17761 = CARTESIAN_POINT ( 'NONE',  ( -17.42409385541299471, -14.80920654474435771, 49.52966884056655772 ) ) ;
#17762 = CARTESIAN_POINT ( 'NONE',  ( -18.64284385541303735, -7.587656875400188738, 49.25157356644812978 ) ) ;
#17763 = EDGE_CURVE ( 'NONE', #25767, #19668, #6707, .T. ) ;
#17764 = CARTESIAN_POINT ( 'NONE',  ( -22.04114742393716142, -9.481025248639415537, 59.73643293354757589 ) ) ;
#17765 =( BOUNDED_CURVE ( )  B_SPLINE_CURVE ( 2, ( #20798, #27452, #23531, #20570, #4813, #16605, #31145, #42487, #8762 ),
 .UNSPECIFIED., .F., .F. ) 
 B_SPLINE_CURVE_WITH_KNOTS ( ( 3, 2, 2, 2, 3 ),
 ( 0.2500000000000001110, 0.2604166666666667407, 0.2708333333333333703, 0.2812500000000000000, 0.2916666666666666297 ),
 .UNSPECIFIED. ) 
 CURVE ( )  GEOMETRIC_REPRESENTATION_ITEM ( )  RATIONAL_B_SPLINE_CURVE ( ( 0.9999999999999992228, 0.9238795325112875156, 1.000000000000000000, 0.9238795325112867385, 1.000000000000000000, 0.9238795325112867385, 1.000000000000000000, 0.9238795325112871826, 0.9999999999999995559 ) ) 
 REPRESENTATION_ITEM ( '' )  );
#17766 = CARTESIAN_POINT ( 'NONE',  ( -35.32409385541306079, -8.109206544744111511, 49.44999999999998863 ) ) ;
#17767 = FACE_BOUND ( 'NONE', #14596, .T. ) ;
#17768 = CARTESIAN_POINT ( 'NONE',  ( -24.09792875595537964, -17.08130417324981565, 72.88336032035921619 ) ) ;
#17769 = CARTESIAN_POINT ( 'NONE',  ( -24.27033155520888030, -13.12649183948492393, 62.98264177272948672 ) ) ;
#17770 = EDGE_CURVE ( 'NONE', #22085, #12430, #44762, .T. ) ;
#17771 = CARTESIAN_POINT ( 'NONE',  ( -20.75918656682226171, -8.147304802054664563, 63.42626204841099735 ) ) ;
#17772 = ORIENTED_EDGE ( 'NONE', *, *, #45422, .F. ) ;
#17773 = PLANE ( 'NONE',  #32925 ) ;
#17774 = CARTESIAN_POINT ( 'NONE',  ( -10.21805405031902225, -12.91800167290361578, 67.78186406512817541 ) ) ;
#17775 = CARTESIAN_POINT ( 'NONE',  ( -16.89979169948162863, -10.14008855580012636, 49.52966884056655772 ) ) ;
#17776 = CARTESIAN_POINT ( 'NONE',  ( -24.13185811504778755, -12.61356036044664464, 66.45813649863244166 ) ) ;
#17777 = ADVANCED_FACE ( 'NONE', ( #45295 ), #23386, .T. ) ;
#17778 = CARTESIAN_POINT ( 'NONE',  ( -11.10681587527927938, -11.67891925637714401, 71.10332952723315714 ) ) ;
#17779 = CARTESIAN_POINT ( 'NONE',  ( -11.54449430114617137, -11.00967495709500810, 57.22519909113746905 ) ) ;
#17780 =( BOUNDED_CURVE ( )  B_SPLINE_CURVE ( 3, ( #15538, #30598, #26901, #41910 ),
 .UNSPECIFIED., .F., .F. ) 
 B_SPLINE_CURVE_WITH_KNOTS ( ( 4, 4 ),
 ( 0.5000000000000000000, 0.9074455897393627346 ),
 .UNSPECIFIED. ) 
 CURVE ( )  GEOMETRIC_REPRESENTATION_ITEM ( )  RATIONAL_B_SPLINE_CURVE ( ( 1.000000000000048628, 0.4567392136813446801, 0.3561768502900010680, 0.6983129098260700829 ) ) 
 REPRESENTATION_ITEM ( '' )  );
#17781 = EDGE_LOOP ( 'NONE', ( #42215, #25329, #8877, #16386, #28819 ) ) ;
#17782 = AXIS2_PLACEMENT_3D ( 'NONE', #940, #45528, #15938 ) ;
#17783 = ORIENTED_EDGE ( 'NONE', *, *, #35710, .F. ) ;
#17784 = AXIS2_PLACEMENT_3D ( 'NONE', #42601, #20901, #8861 ) ;
#17785 = CARTESIAN_POINT ( 'NONE',  ( -16.84284385541304729, -7.587656875400192291, 49.25157356644813689 ) ) ;
#17786 = ORIENTED_EDGE ( 'NONE', *, *, #30655, .F. ) ;
#17787 = CARTESIAN_POINT ( 'NONE',  ( -16.91855014848012928, -22.24212009645463439, 72.28047803099305213 ) ) ;
#17788 = B_SPLINE_CURVE_WITH_KNOTS ( 'NONE', 3,
 ( #9234, #21035, #5548, #39747, #17325, #47391, #20567, #1839, #16836, #28668 ),
 .UNSPECIFIED., .F., .F.,
 ( 4, 2, 2, 2, 4 ),
 ( 0.000000000000000000, 0.2500000000000000000, 0.5000000000000000000, 0.7500000000000000000, 1.000000000000000000 ),
 .UNSPECIFIED. ) ;
#17789 = CARTESIAN_POINT ( 'NONE',  ( -15.41904748403203484, -7.634001509309876532, 74.19490257054667381 ) ) ;
#17790 = CARTESIAN_POINT ( 'NONE',  ( -16.26195973558533936, -21.76306465430365122, 58.57113428431811997 ) ) ;
#17791 = EDGE_LOOP ( 'NONE', ( #10260, #44693, #22601, #43081, #40415 ) ) ;
#17792 = CARTESIAN_POINT ( 'NONE',  ( -10.99197923738610250, -11.04991372156584006, 60.85602641044604155 ) ) ;
#17793 = CARTESIAN_POINT ( 'NONE',  ( 18.62590614458706995, 1.878653161019418816, 52.23023769833749697 ) ) ;
#17794 = ORIENTED_EDGE ( 'NONE', *, *, #48333, .F. ) ;
#17795 = DIRECTION ( 'NONE',  ( -0.09077643883959130022, 0.9958712959773466933, 4.338678762321648003E-08 ) ) ;
#17796 = ADVANCED_FACE ( 'NONE', ( #27775 ), #1424, .T. ) ;
#17797 = FACE_OUTER_BOUND ( 'NONE', #43376, .T. ) ;
#17798 = ORIENTED_EDGE ( 'NONE', *, *, #5712, .F. ) ;
#17799 = CARTESIAN_POINT ( 'NONE',  ( -17.79929111768229433, -7.368650117109674547, 60.18037143928950172 ) ) ;
#17800 = CARTESIAN_POINT ( 'NONE',  ( -21.23484681875272884, -20.74088929683185611, 69.33978048267414351 ) ) ;
#17801 = CARTESIAN_POINT ( 'NONE',  ( -26.42409385541305511, -6.359206544744109735, 47.99999999999997868 ) ) ;
#17802 = ORIENTED_EDGE ( 'NONE', *, *, #42402, .T. ) ;
#17803 = CARTESIAN_POINT ( 'NONE',  ( -10.70297003644833644, -11.59513240183115279, 71.27356180636090244 ) ) ;
#17804 = CARTESIAN_POINT ( 'NONE',  ( -24.41897112398753933, -17.37347453850100720, 69.59835118672229726 ) ) ;
#17805 = CARTESIAN_POINT ( 'NONE',  ( -17.42409385541305511, -14.80920654474410725, 79.00000000000000000 ) ) ;
#17806 = ORIENTED_EDGE ( 'NONE', *, *, #4444, .F. ) ;
#17807 = DIRECTION ( 'NONE',  ( -0.5589780652556125551, 0.8291824422665291516, -7.938832475108110126E-08 ) ) ;
#17808 = EDGE_CURVE ( 'NONE', #24396, #47392, #5471, .T. ) ;
#17809 = LINE ( 'NONE', #7498, #48264 ) ;
#17810 = CIRCLE ( 'NONE', #24900, 1.250000000000001110 ) ;
#17811 = AXIS2_PLACEMENT_3D ( 'NONE', #26473, #34329, #19572 ) ;
#17812 = CARTESIAN_POINT ( 'NONE',  ( -11.70966707598573819, -10.02926654750783975, 67.64896868923555928 ) ) ;
#17813 = CARTESIAN_POINT ( 'NONE',  ( -22.46784385650551741, -6.428312510596449592, 51.20221977374900035 ) ) ;
#17814 = CARTESIAN_POINT ( 'NONE',  ( -16.64258257546838138, -22.21885596081591174, 68.88215988439684168 ) ) ;
#17815 = DIRECTION ( 'NONE',  ( -3.071710424422018668E-17, 6.404604876783312462E-16, 1.000000000000000000 ) ) ;
#17816 = ORIENTED_EDGE ( 'NONE', *, *, #2791, .F. ) ;
#17817 = CARTESIAN_POINT ( 'NONE',  ( -17.74348949963705024, -22.25235684858374796, 58.55553378380137985 ) ) ;
#17818 = VECTOR ( 'NONE', #37327, 1000.000000000000000 ) ;
#17819 = DIRECTION ( 'NONE',  ( -0.9048399035850771543, -0.4257519804770707461, -1.330923645920820637E-08 ) ) ;
#17820 = DIRECTION ( 'NONE',  ( -3.071710424422018668E-17, 6.404604876783312462E-16, 1.000000000000000000 ) ) ;
#17821 = ORIENTED_EDGE ( 'NONE', *, *, #34271, .F. ) ;
#17822 = DIRECTION ( 'NONE',  ( 0.9562635972186038780, -0.2925062950340272527, 4.666065131241567634E-08 ) ) ;
#17823 = B_SPLINE_CURVE_WITH_KNOTS ( 'NONE', 3,
 ( #37521, #11944, #26223, #44958, #139, #4078, #26716, #607, #41236, #38513 ),
 .UNSPECIFIED., .F., .F.,
 ( 4, 2, 2, 2, 4 ),
 ( 0.000000000000000000, 0.2500000000000000000, 0.5000000000000000000, 0.7500000000000000000, 1.000000000000000000 ),
 .UNSPECIFIED. ) ;
#17824 = EDGE_CURVE ( 'NONE', #12655, #39442, #23615, .T. ) ;
#17825 = VERTEX_POINT ( 'NONE', #1677 ) ;
#17826 = ORIENTED_EDGE ( 'NONE', *, *, #43874, .T. ) ;
#17827 = ORIENTED_EDGE ( 'NONE', *, *, #10316, .T. ) ;
#17828 = EDGE_CURVE ( 'NONE', #31288, #34613, #42575, .T. ) ;
#17829 = CARTESIAN_POINT ( 'NONE',  ( -13.96006829630253776, -20.89348458149306964, 72.15437620276698283 ) ) ;
#17830 = CARTESIAN_POINT ( 'NONE',  ( -22.66727079836811853, -10.09628861529951216, 70.16178520457069112 ) ) ;
#17831 = DIRECTION ( 'NONE',  ( 0.8083598999316397027, 0.5886886037477749856, 6.671815825018552065E-08 ) ) ;
#17832 = ORIENTED_EDGE ( 'NONE', *, *, #24330, .T. ) ;
#17833 = EDGE_LOOP ( 'NONE', ( #17319, #27472, #25798, #5159 ) ) ;
#17834 = CARTESIAN_POINT ( 'NONE',  ( -17.60534385650551670, -8.801233750844183135, 48.81488406609782515 ) ) ;
#17835 = DIRECTION ( 'NONE',  ( -1.000000000000000000, 0.000000000000000000, -1.927470528863119295E-16 ) ) ;
#17836 = DIRECTION ( 'NONE',  ( 0.7506333037770493988, -0.6607190350373991494, 0.000000000000000000 ) ) ;
#17838 = EDGE_CURVE ( 'NONE', #41531, #25220, #12270, .T. ) ;
#17837 = CARTESIAN_POINT ( 'NONE',  ( -20.58659385650551599, -9.302874398569244363, 51.68646062012417985 ) ) ;
#17839 = EDGE_CURVE ( 'NONE', #13744, #18062, #14874, .T. ) ;
#17840 = VECTOR ( 'NONE', #6826, 1000.000000000000000 ) ;
#17841 = ORIENTED_EDGE ( 'NONE', *, *, #40832, .T. ) ;
#17842 = ADVANCED_FACE ( 'NONE', ( #39094 ), #35019, .T. ) ;
#17843 = EDGE_CURVE ( 'NONE', #35459, #41905, #43619, .T. ) ;
#17844 = ADVANCED_FACE ( 'NONE', ( #20640 ), #20397, .T. ) ;
#17845 = DIRECTION ( 'NONE',  ( -3.071710424422018668E-17, 6.404604876783312462E-16, 1.000000000000000000 ) ) ;
#17846 = CARTESIAN_POINT ( 'NONE',  ( -12.55198883488284878, -12.25722835735234639, 53.49899999999994549 ) ) ;
#17847 =( BOUNDED_CURVE ( )  B_SPLINE_CURVE ( 3, ( #24157, #31294, #17231, #27602 ),
 .UNSPECIFIED., .F., .F. ) 
 B_SPLINE_CURVE_WITH_KNOTS ( ( 4, 4 ),
 ( 0.000000000000000000, 0.4074455897393622905 ),
 .UNSPECIFIED. ) 
 CURVE ( )  GEOMETRIC_REPRESENTATION_ITEM ( )  RATIONAL_B_SPLINE_CURVE ( ( 1.000000000000000000, 0.4567392136813342995, 0.3561768502900312106, 0.6983129098260907330 ) ) 
 REPRESENTATION_ITEM ( '' )  );
#17848 = VECTOR ( 'NONE', #5228, 1000.000000000000000 ) ;
#17849 = EDGE_LOOP ( 'NONE', ( #12554, #41617, #18868, #36453 ) ) ;
#17850 = DIRECTION ( 'NONE',  ( -2.168404344971008375E-16, -0.000000000000000000, 1.000000000000000000 ) ) ;
#17851 = ORIENTED_EDGE ( 'NONE', *, *, #16638, .T. ) ;
#17852 = CARTESIAN_POINT ( 'NONE',  ( -14.48548941065489970, -8.400516866317895293, 67.27447142263336843 ) ) ;
#17853 = CARTESIAN_POINT ( 'NONE',  ( -19.52605052145376874, -21.48662438560833365, 65.48102853648620680 ) ) ;
#17854 = CARTESIAN_POINT ( 'NONE',  ( -10.39890676938329150, -12.32907080782536191, 57.45044596432388317 ) ) ;
#17855 = VERTEX_POINT ( 'NONE', #9316 ) ;
#17856 = FACE_OUTER_BOUND ( 'NONE', #32643, .T. ) ;
#17857 = CARTESIAN_POINT ( 'NONE',  ( -16.84284385541304374, -7.587656875400191403, 49.25157356644812978 ) ) ;
#17858 = CARTESIAN_POINT ( 'NONE',  ( -18.03604760049577393, -21.78284572725946333, 65.36148796969293073 ) ) ;
#17859 = ORIENTED_EDGE ( 'NONE', *, *, #1915, .F. ) ;
#17860 = CARTESIAN_POINT ( 'NONE',  ( -24.83347472307691817, -15.58731732267899694, 73.18020620047872171 ) ) ;
#17861 = DIRECTION ( 'NONE',  ( 0.9956360040033426229, -0.09332174201254497814, 0.000000000000000000 ) ) ;
#17862 = DIRECTION ( 'NONE',  ( 0.000000000000000000, 0.000000000000000000, 1.000000000000000000 ) ) ;
#17863 = ORIENTED_EDGE ( 'NONE', *, *, #6547, .T. ) ;
#17864 = CARTESIAN_POINT ( 'NONE',  ( -13.37636250268599092, -20.58507941322447365, 61.93135214938352107 ) ) ;
#17865 = EDGE_LOOP ( 'NONE', ( #15154, #6137, #42023, #7520, #354 ) ) ;
#17866 = CARTESIAN_POINT ( 'NONE',  ( -13.18362795047878144, -8.683667697493742565, 60.62445659250467145 ) ) ;
#17868 = EDGE_CURVE ( 'NONE', #21243, #39081, #1914, .T. ) ;
#17867 = DIRECTION ( 'NONE',  ( -0.06357898915123239014, 0.9979768094191906469, 2.064515410283096215E-19 ) ) ;
#17869 = CARTESIAN_POINT ( 'NONE',  ( -36.42409385541304800, -9.359200813967566646, 50.49621490985803263 ) ) ;
#17870 = ORIENTED_EDGE ( 'NONE', *, *, #44515, .F. ) ;
#17871 = CARTESIAN_POINT ( 'NONE',  ( -22.09234465700630423, -20.09219189623108548, 62.23439162498055310 ) ) ;
#17872 = CARTESIAN_POINT ( 'NONE',  ( -10.92672688430831229, -11.16395088679539249, 64.40527978002718612 ) ) ;
#17873 = FACE_OUTER_BOUND ( 'NONE', #16578, .T. ) ;
#17874 = ORIENTED_EDGE ( 'NONE', *, *, #1916, .T. ) ;
#17875 = CARTESIAN_POINT ( 'NONE',  ( -23.73621606195537481, -11.66110265205040974, 59.69055757226052350 ) ) ;
#17876 = VECTOR ( 'NONE', #22646, 1000.000000000000114 ) ;
#17877 = VECTOR ( 'NONE', #38097, 1000.000000000000000 ) ;
#17878 = CARTESIAN_POINT ( 'NONE',  ( -24.76903642440577258, -16.05600587708614668, 66.16350687787337392 ) ) ;
#17879 = ORIENTED_EDGE ( 'NONE', *, *, #39631, .F. ) ;
#17880 = ORIENTED_EDGE ( 'NONE', *, *, #45811, .T. ) ;
#17881 = DIRECTION ( 'NONE',  ( -3.071710424422018668E-17, 6.404604876783312462E-16, 1.000000000000000000 ) ) ;
#17882 = CARTESIAN_POINT ( 'NONE',  ( -19.41474593944376537, -21.52019035999878938, 61.99503644832097393 ) ) ;
#17883 = VECTOR ( 'NONE', #41833, 1000.000000000000000 ) ;
#17884 = CYLINDRICAL_SURFACE ( 'NONE', #41598, 1.999999999999999112 ) ;
#17885 = CARTESIAN_POINT ( 'NONE',  ( -23.92640620196626600, -11.17277965375445703, 70.14856683682155847 ) ) ;
#17886 = CARTESIAN_POINT ( 'NONE',  ( -12.29927561225700750, -19.57981844400423910, 61.58605613336224849 ) ) ;
#17887 = CARTESIAN_POINT ( 'NONE',  ( -17.42409385541299471, -14.80920654474434883, 62.02966884056656482 ) ) ;
#17888 = DIRECTION ( 'NONE',  ( -3.071710424422018668E-17, 6.404604876783312462E-16, 1.000000000000000000 ) ) ;
#17889 = AXIS2_PLACEMENT_3D ( 'NONE', #20271, #30643, #35275 ) ;
#17890 = ORIENTED_EDGE ( 'NONE', *, *, #31715, .F. ) ;
#17891 = ORIENTED_EDGE ( 'NONE', *, *, #45634, .F. ) ;
#17892 = CARTESIAN_POINT ( 'NONE',  ( -19.42896615819153538, -21.56812558881098241, 62.14503644571260565 ) ) ;
#17893 = PLANE ( 'NONE',  #38563 ) ;
#17894 = CARTESIAN_POINT ( 'NONE',  ( -10.38078070663892660, -14.50222156296673148, 67.85800126083267969 ) ) ;
#17895 = CARTESIAN_POINT ( 'NONE',  ( -19.01896746559008733, -7.531908412828363097, 67.00097544457088361 ) ) ;
#17896 = DIRECTION ( 'NONE',  ( 0.000000000000000000, 0.000000000000000000, 1.000000000000000000 ) ) ;
#17897 = ORIENTED_EDGE ( 'NONE', *, *, #30353, .F. ) ;
#17898 =( BOUNDED_CURVE ( )  B_SPLINE_CURVE ( 3, ( #4015, #7962, #37967, #11884 ),
 .UNSPECIFIED., .F., .F. ) 
 B_SPLINE_CURVE_WITH_KNOTS ( ( 4, 4 ),
 ( 4.712388980384689674, 4.921828490624008623 ),
 .UNSPECIFIED. ) 
 CURVE ( )  GEOMETRIC_REPRESENTATION_ITEM ( )  RATIONAL_B_SPLINE_CURVE ( ( 1.000000000000000000, 0.9963479302455156006, 0.9963479302455156006, 1.000000000000000000 ) ) 
 REPRESENTATION_ITEM ( '' )  );
#17899 = CARTESIAN_POINT ( 'NONE',  ( -18.64284385650551812, -8.811426318492348031, 52.18089403414751359 ) ) ;
#17900 = EDGE_LOOP ( 'NONE', ( #43825, #44999 ) ) ;
#17901 = EDGE_CURVE ( 'NONE', #15165, #26529, #18620, .T. ) ;
#17902 = ADVANCED_FACE ( 'NONE', ( #17153 ), #36588, .T. ) ;
#17903 = CARTESIAN_POINT ( 'NONE',  ( -22.37985696210566999, -19.82347738784875801, 69.32417989525721680 ) ) ;
#17904 = CARTESIAN_POINT ( 'NONE',  ( -11.96181355942711910, -19.87549434724351727, 58.11177690156993947 ) ) ;
#17905 = DIRECTION ( 'NONE',  ( 0.9687793358424822143, -0.2479245821708672415, 0.000000000000000000 ) ) ;
#17906 = CARTESIAN_POINT ( 'NONE',  ( -10.09263637371726041, -16.13336529236863015, 68.02121877882343881 ) ) ;
#17907 = CIRCLE ( 'NONE', #17945, 1.999999999999994893 ) ;
#17908 = ORIENTED_EDGE ( 'NONE', *, *, #36170, .F. ) ;
#17909 =( BOUNDED_CURVE ( )  B_SPLINE_CURVE ( 3, ( #712, #7624, #48724, #7377 ),
 .UNSPECIFIED., .F., .F. ) 
 B_SPLINE_CURVE_WITH_KNOTS ( ( 4, 4 ),
 ( 0.4074455897393636228, 0.5000000000000000000 ),
 .UNSPECIFIED. ) 
 CURVE ( )  GEOMETRIC_REPRESENTATION_ITEM ( )  RATIONAL_B_SPLINE_CURVE ( ( 0.6983129098260894008, 0.7760317562606912078, 0.8765941196519937417, 0.9999999999999938938 ) ) 
 REPRESENTATION_ITEM ( '' )  );
#17910 = AXIS2_PLACEMENT_3D ( 'NONE', #3167, #10330, #32941 ) ;
#17911 = EDGE_CURVE ( 'NONE', #26590, #28413, #10523, .T. ) ;
#17912 = ADVANCED_FACE ( 'NONE', ( #10282 ), #2943, .T. ) ;
#17913 = B_SPLINE_CURVE_WITH_KNOTS ( 'NONE', 3,
 ( #33384, #425, #4353, #14654, #19361, #44759, #26033, #41050, #14917, #29974 ),
 .UNSPECIFIED., .F., .F.,
 ( 4, 2, 2, 2, 4 ),
 ( 0.000000000000000000, 0.2500000000000000000, 0.5000000000000000000, 0.7500000000000000000, 1.000000000000000000 ),
 .UNSPECIFIED. ) ;
#17914 = CARTESIAN_POINT ( 'NONE',  ( -22.18998830427770841, -20.00468049915955859, 65.71893796558269685 ) ) ;
#17915 = CARTESIAN_POINT ( 'NONE',  ( -12.74558454090558257, -9.602248860578644241, 74.54596281605876129 ) ) ;
#17916 = AXIS2_PLACEMENT_3D ( 'NONE', #34235, #14767, #38170 ) ;
#17917 = CARTESIAN_POINT ( 'NONE',  ( -17.19980212172655953, -7.762775302065858085, 70.79035839668003405 ) ) ;
#17918 = DIRECTION ( 'NONE',  ( -0.7489133456531319455, -0.6626679415081375701, 6.686399169904807035E-09 ) ) ;
#17919 = VERTEX_POINT ( 'NONE', #2638 ) ;
#17920 = CARTESIAN_POINT ( 'NONE',  ( -24.72409385541305582, -14.80920654474413745, 60.91764705882351905 ) ) ;
#17921 =( BOUNDED_CURVE ( )  B_SPLINE_CURVE ( 3, ( #46464, #42995, #42526, #9270 ),
 .UNSPECIFIED., .F., .F. ) 
 B_SPLINE_CURVE_WITH_KNOTS ( ( 4, 4 ),
 ( 0.5000000000000000000, 0.9074455897393698400 ),
 .UNSPECIFIED. ) 
 CURVE ( )  GEOMETRIC_REPRESENTATION_ITEM ( )  RATIONAL_B_SPLINE_CURVE ( ( 1.000000000000002220, 0.4567392136813248626, 0.3561768502900259925, 0.6983129098261080525 ) ) 
 REPRESENTATION_ITEM ( '' )  );
#17922 = ORIENTED_EDGE ( 'NONE', *, *, #663, .F. ) ;
#17923 = DIRECTION ( 'NONE',  ( 0.8398192074808118468, 0.5428661886195297326, 7.907900705247677662E-08 ) ) ;
#17924 = ORIENTED_EDGE ( 'NONE', *, *, #36392, .F. ) ;
#17925 = CARTESIAN_POINT ( 'NONE',  ( -45.92409385541306222, -14.80920654474410902, 69.15000000000000568 ) ) ;
#17926 = ADVANCED_FACE ( 'NONE', ( #44031 ), #45124, .T. ) ;
#17927 = CARTESIAN_POINT ( 'NONE',  ( -14.84909385650551705, -8.104110260919579645, 48.81699501597546487 ) ) ;
#17928 = ORIENTED_EDGE ( 'NONE', *, *, #8995, .T. ) ;
#17929 = ADVANCED_BREP_SHAPE_REPRESENTATION ( '', ( #32222, #29031 ), #4656 ) ;
#17930 = DIRECTION ( 'NONE',  ( 1.000000000000000000, 1.669677910507523057E-21, 6.493791346278465266E-22 ) ) ;
#17931 = CARTESIAN_POINT ( 'NONE',  ( -20.89331258220900978, -11.64059849529350643, 49.52966884056655772 ) ) ;
#17932 = CARTESIAN_POINT ( 'NONE',  ( -24.86169257816691314, -14.37661386440606037, 66.34326115264040880 ) ) ;
#17933 = EDGE_LOOP ( 'NONE', ( #42088, #21983, #46711, #42133, #43217 ) ) ;
#17934 = LINE ( 'NONE', #13988, #27083 ) ;
#17935 = LINE ( 'NONE', #13756, #29036 ) ;
#17936 = DIRECTION ( 'NONE',  ( 1.927470528863184130E-16, 1.434740771370715221E-29, -1.000000000000000000 ) ) ;
#17937 = ORIENTED_EDGE ( 'NONE', *, *, #45803, .T. ) ;
#17938 = EDGE_LOOP ( 'NONE', ( #45583, #40828, #46602, #37378 ) ) ;
#17939 = CARTESIAN_POINT ( 'NONE',  ( -19.38197731428664028, -19.06713733463150007, 52.02966884056656482 ) ) ;
#17940 = DIRECTION ( 'NONE',  ( 1.000000000000000000, 2.866981220435666553E-17, 0.000000000000000000 ) ) ;
#17942 = CARTESIAN_POINT ( 'NONE',  ( -13.82526118368687484, -18.63162768858978779, 52.02966884056656482 ) ) ;
#17941 = AXIS2_PLACEMENT_3D ( 'NONE', #11584, #39137, #16227 ) ;
#17943 = CARTESIAN_POINT ( 'NONE',  ( -15.41159385759799072, -8.990409506049202193, 49.61344411288074951 ) ) ;
#17944 = CARTESIAN_POINT ( 'NONE',  ( -24.12000719736520438, -11.54295319193055214, 63.20864192093194589 ) ) ;
#17945 = AXIS2_PLACEMENT_3D ( 'NONE', #12991, #28019, #9323 ) ;
#17946 = LINE ( 'NONE', #25841, #44806 ) ;
#17947 = CARTESIAN_POINT ( 'NONE',  ( -23.66547331395526044, -18.87718802671421159, 69.40097851167932674 ) ) ;
#17948 = AXIS2_PLACEMENT_3D ( 'NONE', #47882, #36762, #14114 ) ;
#17949 = CIRCLE ( 'NONE', #41563, 5.249999999999998224 ) ;
#17950 = CARTESIAN_POINT ( 'NONE',  ( -14.76438121721707830, -8.332445897900056409, 63.90051825552988873 ) ) ;
#17951 = ORIENTED_EDGE ( 'NONE', *, *, #25702, .T. ) ;
#17952 = CARTESIAN_POINT ( 'NONE',  ( -20.81971067820157728, -8.177204663279967534, 59.95469905373763453 ) ) ;
#17953 = CARTESIAN_POINT ( 'NONE',  ( -13.46747890590686403, -9.034676489092227314, 60.43950277890026967 ) ) ;
#17954 = CARTESIAN_POINT ( 'NONE',  ( -24.05845762361657947, -12.57644656616312773, 73.24225570276865938 ) ) ;
#17955 = CARTESIAN_POINT ( 'NONE',  ( -13.49987067987283673, -9.012482076563856026, 60.73950329009904436 ) ) ;
#17956 = VERTEX_POINT ( 'NONE', #36116 ) ;
#17957 = VERTEX_POINT ( 'NONE', #47468 ) ;
#17958 = EDGE_CURVE ( 'NONE', #42977, #36746, #23652, .T. ) ;
#17959 = CYLINDRICAL_SURFACE ( 'NONE', #26477, 0.1499999999999953038 ) ;
#17960 = CARTESIAN_POINT ( 'NONE',  ( -19.67760665824181388, -21.48965406232008490, 65.75014118398131302 ) ) ;
#17961 = CARTESIAN_POINT ( 'NONE',  ( -23.31260078967427063, -19.37299621621055579, 58.98436398315890727 ) ) ;
#17962 = CYLINDRICAL_SURFACE ( 'NONE', #37414, 1.249999999999998668 ) ;
#17963 = EDGE_LOOP ( 'NONE', ( #41774, #27313 ) ) ;
#17964 = CYLINDRICAL_SURFACE ( 'NONE', #43189, 1.949999999999999734 ) ;
#17965 = ADVANCED_FACE ( 'NONE', ( #29230 ), #44502, .F. ) ;
#17966 = CARTESIAN_POINT ( 'NONE',  ( -23.81432972337535858, -17.66677937220956451, 59.07666504472891233 ) ) ;
#17967 = ORIENTED_EDGE ( 'NONE', *, *, #19086, .T. ) ;
#17968 = EDGE_CURVE ( 'NONE', #39713, #24660, #6821, .T. ) ;
#17969 = CARTESIAN_POINT ( 'NONE',  ( -13.65852477070391480, -21.23755994396627145, 68.64963458044397271 ) ) ;
#17970 = CIRCLE ( 'NONE', #40008, 5.249999999999998224 ) ;
#17971 = CARTESIAN_POINT ( 'NONE',  ( -12.50776634899986384, -20.40684016789016297, 71.92158251742569064 ) ) ;
#17972 = EDGE_CURVE ( 'NONE', #7134, #19297, #37717, .T. ) ;
#17973 = PRODUCT_DEFINITION_FORMATION_WITH_SPECIFIED_SOURCE ( 'ANY', '', #46082, .NOT_KNOWN. ) ;
#17974 = EDGE_LOOP ( 'NONE', ( #36735, #15817, #5726, #1952, #34356 ) ) ;
#17975 = CARTESIAN_POINT ( 'NONE',  ( -11.86969123986252406, -10.46139627614129708, 67.49896775950338679 ) ) ;
#17976 = CIRCLE ( 'NONE', #3854, 1.000000000000000888 ) ;
#17977 = ORIENTED_EDGE ( 'NONE', *, *, #3619, .F. ) ;
#17978 = CARTESIAN_POINT ( 'NONE',  ( -19.75048190521760461, -21.47275536819973141, 62.15070614013394135 ) ) ;
#17979 = DIRECTION ( 'NONE',  ( -0.3478314405900309603, -0.9375570856950864451, 9.567072274253696421E-17 ) ) ;
#17980 = ORIENTED_EDGE ( 'NONE', *, *, #40896, .T. ) ;
#17981 = CARTESIAN_POINT ( 'NONE',  ( -24.43392429566424440, -14.02363658386207668, 69.65275204483315008 ) ) ;
#17982 = CARTESIAN_POINT ( 'NONE',  ( -24.49584582974870628, -12.46528025919705485, 73.49871492906470394 ) ) ;
#17983 = EDGE_CURVE ( 'NONE', #45657, #45009, #16462, .T. ) ;
#17984 = DIRECTION ( 'NONE',  ( 0.9477661110324760996, -0.3189661404888857188, 2.738326501554841424E-08 ) ) ;
#17985 = CIRCLE ( 'NONE', #40819, 3.982850737850967437 ) ;
#17986 = B_SPLINE_CURVE_WITH_KNOTS ( 'NONE', 3,
 ( #6910, #45092, #26356, #30069, #48509, #3453, #21927, #29816, #7910, #273 ),
 .UNSPECIFIED., .F., .F.,
 ( 4, 2, 2, 2, 4 ),
 ( 0.000000000000000000, 0.2500000000000000000, 0.5000000000000000000, 0.7500000000000000000, 1.000000000000000000 ),
 .UNSPECIFIED. ) ;
#17987 = DIRECTION ( 'NONE',  ( 1.224646799147353207E-16, 1.000000000000000000, -1.912410701131276611E-32 ) ) ;
#17988 = DIRECTION ( 'NONE',  ( -4.133538128552115272E-06, 2.214839418041148178E-07, -0.9999999999914322979 ) ) ;
#17989 = DIRECTION ( 'NONE',  ( 0.9687793358424821033, -0.2479245821708680464, 0.000000000000000000 ) ) ;
#17990 = VERTEX_POINT ( 'NONE', #8064 ) ;
#17991 = CARTESIAN_POINT ( 'NONE',  ( -16.90422089642926906, -22.24121457338818431, 72.30509853249346008 ) ) ;
#17992 = CARTESIAN_POINT ( 'NONE',  ( -22.46373187589079379, -16.28044704940516496, 52.02966884056656482 ) ) ;
#17993 = DIRECTION ( 'NONE',  ( 2.699622411496199987E-06, -1.161037829314838553E-05, -0.9999999999289554964 ) ) ;
#17994 = PLANE ( 'NONE',  #11651 ) ;
#17995 = CARTESIAN_POINT ( 'NONE',  ( -13.54823245630066175, -20.69819609872914157, 61.81646323537678001 ) ) ;
#17996 = CARTESIAN_POINT ( 'NONE',  ( -13.80534385650551776, -8.801233750844183135, 48.81488406609782515 ) ) ;
#17997 = EDGE_LOOP ( 'NONE', ( #46877, #34385, #46129, #6074, #45023 ) ) ;
#17998 = VERTEX_POINT ( 'NONE', #419 ) ;
#17999 = CARTESIAN_POINT ( 'NONE',  ( -11.06796828401846078, -18.69550736580278993, 61.53356777548469125 ) ) ;
#18000 = CARTESIAN_POINT ( 'NONE',  ( -11.03230881600246427, -10.98182333549695322, 60.79390388117851529 ) ) ;
#18001 = ORIENTED_EDGE ( 'NONE', *, *, #14831, .T. ) ;
#18003 = CARTESIAN_POINT ( 'NONE',  ( -13.78034385650551563, -6.424090610841176385, 49.80797279389977916 ) ) ;
#18002 = CARTESIAN_POINT ( 'NONE',  ( -15.35852799358099929, -7.651226727379689230, 74.18647339208507674 ) ) ;
#18004 = CARTESIAN_POINT ( 'NONE',  ( -14.01837044221388417, -8.636059239884620098, 74.48482605064899076 ) ) ;
#18005 = CARTESIAN_POINT ( 'NONE',  ( -12.44869005970189058, -9.885249076858732664, 57.08935532200567309 ) ) ;
#18006 = CARTESIAN_POINT ( 'NONE',  ( -12.05727448861903639, -19.97649948735875114, 61.65324539733175868 ) ) ;
#18007 = CARTESIAN_POINT ( 'NONE',  ( -22.07241914523459769, -20.11453564365663027, 65.79601743996857977 ) ) ;
#18008 = CARTESIAN_POINT ( 'NONE',  ( -23.91439714532632621, -17.43141235356291574, 65.94357239632037704 ) ) ;
#18009 = CARTESIAN_POINT ( 'NONE',  ( -12.64995474452274138, -19.99670071527213366, 68.63657438322856308 ) ) ;
#18010 = DIRECTION ( 'NONE',  ( 0.000000000000000000, 0.9999954153791273948, 0.003028072113821686159 ) ) ;
#18011 = ORIENTED_EDGE ( 'NONE', *, *, #25091, .T. ) ;
#18012 = DIRECTION ( 'NONE',  ( 1.000000000000000000, 2.866981220435666553E-17, 0.000000000000000000 ) ) ;
#18013 = CARTESIAN_POINT ( 'NONE',  ( -11.60439305645412844, -10.15781863991614031, 71.14705871384585123 ) ) ;
#18014 = CARTESIAN_POINT ( 'NONE',  ( -16.91855125566938511, -22.24212016642244905, 72.28047911973106920 ) ) ;
#18015 = CARTESIAN_POINT ( 'NONE',  ( -15.28291064399146215, -21.52618758091310980, 68.57592918174772478 ) ) ;
#18016 = CARTESIAN_POINT ( 'NONE',  ( -24.61562913124599916, -12.86357381044341430, 66.55892682786348757 ) ) ;
#18017 = EDGE_CURVE ( 'NONE', #24237, #45073, #653, .T. ) ;
#18018 = DIRECTION ( 'NONE',  ( -2.430360958779124298E-06, -9.751098539734333949E-07, 0.9999999999965712982 ) ) ;
#18019 = CYLINDRICAL_SURFACE ( 'NONE', #40127, 0.1500000000000047407 ) ;
#18020 = CIRCLE ( 'NONE', #41628, 4.686499999999998778 ) ;
#18021 = CIRCLE ( 'NONE', #15677, 5.249999999999998224 ) ;
#18022 = VERTEX_POINT ( 'NONE', #37085 ) ;
#18023 = ORIENTED_EDGE ( 'NONE', *, *, #33642, .T. ) ;
#18024 = CARTESIAN_POINT ( 'NONE',  ( -16.05534385541304232, -8.623186033802570094, 49.24843789510467218 ) ) ;
#18025 = ORIENTED_EDGE ( 'NONE', *, *, #34392, .T. ) ;
#18026 = CARTESIAN_POINT ( 'NONE',  ( -23.54173688680538135, -19.06112029705675681, 66.00202217072055078 ) ) ;
#18027 = CARTESIAN_POINT ( 'NONE',  ( -20.06397283958904865, -8.325598795413901243, 74.00479983096190040 ) ) ;
#18028 = VECTOR ( 'NONE', #38733, 1000.000000000000000 ) ;
#18029 = DIRECTION ( 'NONE',  ( -3.071710424422018668E-17, 6.404604876783312462E-16, 1.000000000000000000 ) ) ;
#18030 = FACE_OUTER_BOUND ( 'NONE', #46562, .T. ) ;
#18031 = ORIENTED_EDGE ( 'NONE', *, *, #9992, .T. ) ;
#18032 = EDGE_CURVE ( 'NONE', #17998, #21919, #26543, .T. ) ;
#18033 = APPLICATION_CONTEXT ( 'automotive_design' ) ;
#18034 = CARTESIAN_POINT ( 'NONE',  ( -13.76849323099554567, -20.83774554052356365, 65.27156739751333703 ) ) ;
#18035 = CARTESIAN_POINT ( 'NONE',  ( -21.00520398765801744, -21.34214743040633167, 62.37117330845665464 ) ) ;
#18036 = EDGE_CURVE ( 'NONE', #23317, #6093, #7159, .T. ) ;
#18037 =( BOUNDED_CURVE ( )  B_SPLINE_CURVE ( 3, ( #46024, #19424, #26095, #19187 ),
 .UNSPECIFIED., .F., .F. ) 
 B_SPLINE_CURVE_WITH_KNOTS ( ( 4, 4 ),
 ( 0.000000000000000000, 0.4074455897393680082 ),
 .UNSPECIFIED. ) 
 CURVE ( )  GEOMETRIC_REPRESENTATION_ITEM ( )  RATIONAL_B_SPLINE_CURVE ( ( 1.000000000000000000, 0.4567392136813361314, 0.3561768502900318767, 0.6983129098260871803 ) ) 
 REPRESENTATION_ITEM ( '' )  );
#18038 = EDGE_LOOP ( 'NONE', ( #39339, #33879, #21411, #48516, #47409 ) ) ;
#18039 = CARTESIAN_POINT ( 'NONE',  ( -18.50932193227059841, -21.77517953109191495, 72.58510940649489385 ) ) ;
#18040 = CARTESIAN_POINT ( 'NONE',  ( -18.08884787034790875, -9.601462109806339740, 49.52966884056655772 ) ) ;
#18041 = ORIENTED_EDGE ( 'NONE', *, *, #38886, .T. ) ;
#18042 = ADVANCED_FACE ( 'NONE', ( #18612 ), #26509, .T. ) ;
#18043 = CARTESIAN_POINT ( 'NONE',  ( -23.00441930688031889, -19.11762475274336737, 59.03410642058399560 ) ) ;
#18044 = DIRECTION ( 'NONE',  ( -1.000000000000000000, 1.224646799147353207E-16, -3.435970187611875923E-15 ) ) ;
#18045 = DIRECTION ( 'NONE',  ( -0.4251432040024066272, -0.9051260995521939190, -1.185120001106687566E-09 ) ) ;
#18046 = ORIENTED_EDGE ( 'NONE', *, *, #12128, .T. ) ;
#18047 = CARTESIAN_POINT ( 'NONE',  ( -10.98892314574976226, -11.92244160250971419, 70.97372176798174337 ) ) ;
#18048 = CARTESIAN_POINT ( 'NONE',  ( -23.38668188022877814, -18.47650611194418957, 72.76368285100856781 ) ) ;
#18049 = AXIS2_PLACEMENT_3D ( 'NONE', #27446, #42231, #11283 ) ;
#18050 = EDGE_CURVE ( 'NONE', #48039, #4198, #18927, .T. ) ;
#18051 =( BOUNDED_SURFACE ( )  B_SPLINE_SURFACE ( 3, 1, ( 
 ( #24094, #43042 ),
 ( #32448, #16442 ),
 ( #2405, #12515 ),
 ( #20644, #46511 ),
 ( #27540, #42583 ),
 ( #8845, #23861 ),
 ( #5141, #31475 ) ),
 .UNSPECIFIED., .T., .F., .F. ) 
 B_SPLINE_SURFACE_WITH_KNOTS ( ( 4, 3, 4 ),
 ( 2, 2 ),
 ( 0.000000000000000000, 0.5000000000000000000, 1.000000000000000000 ),
 ( 0.000000000000000000, 1.000000000000000000 ),
 .UNSPECIFIED. ) 
 GEOMETRIC_REPRESENTATION_ITEM ( )  RATIONAL_B_SPLINE_SURFACE ( (
 ( 1.000000000000000000, 1.000000000000000000),
 ( 0.3333333333333335369, 0.3333333333333330373),
 ( 0.3333333333333335369, 0.3333333333333330373),
 ( 1.000000000000000000, 1.000000000000000000),
 ( 0.3333333333333333703, 0.3333333333333333703),
 ( 0.3333333333333333703, 0.3333333333333333703),
 ( 1.000000000000000000, 1.000000000000000000) ) ) 
 REPRESENTATION_ITEM ( '' )  SURFACE ( )  );
#18052 = CARTESIAN_POINT ( 'NONE',  ( -14.01837044221388417, -8.636059239884620098, 74.48482605064899076 ) ) ;
#18053 = CARTESIAN_POINT ( 'NONE',  ( -12.22871965896205460, -20.14873714605892019, 65.01674887276816150 ) ) ;
#18054 = EDGE_LOOP ( 'NONE', ( #161, #6123 ) ) ;
#18055 = CARTESIAN_POINT ( 'NONE',  ( -13.88293547364789404, -20.90532801101632998, 68.75625136993008368 ) ) ;
#18056 = AXIS2_PLACEMENT_3D ( 'NONE', #31670, #46691, #20096 ) ;
#18057 = CARTESIAN_POINT ( 'NONE',  ( -10.72769102952926978, -12.77004266858777726, 60.98956792496692714 ) ) ;
#18058 = CARTESIAN_POINT ( 'NONE',  ( -23.16275847746607752, -18.91806288495012112, 69.43805163930900903 ) ) ;
#18059 = CARTESIAN_POINT ( 'NONE',  ( -11.47236147394688111, -10.32806163424019985, 74.55389795262664165 ) ) ;
#18060 = LINE ( 'NONE', #14585, #6251 ) ;
#18061 = DIRECTION ( 'NONE',  ( -0.07061531369766042843, -0.9975036227860933913, -1.268851337311104735E-08 ) ) ;
#18062 = VERTEX_POINT ( 'NONE', #48421 ) ;
#18063 = CARTESIAN_POINT ( 'NONE',  ( -41.55277032600130127, -14.80920654474423159, 69.97058823529410176 ) ) ;
#18064 = AXIS2_PLACEMENT_3D ( 'NONE', #1428, #24337, #16921 ) ;
#18065 = CARTESIAN_POINT ( 'NONE',  ( -18.92409385541305511, -14.80920654474410547, 52.21286476528345588 ) ) ;
#18066 = CARTESIAN_POINT ( 'NONE',  ( -18.59601872632196873, -7.856991649524070809, 73.85536540707786912 ) ) ;
#18067 = ORIENTED_EDGE ( 'NONE', *, *, #25606, .F. ) ;
#18068 = CARTESIAN_POINT ( 'NONE',  ( -6.424093855413055110, -27.10920654474410796, 79.99999999999998579 ) ) ;
#18069 =( BOUNDED_CURVE ( )  B_SPLINE_CURVE ( 3, ( #8163, #15505, #45597, #38166 ),
 .UNSPECIFIED., .F., .F. ) 
 B_SPLINE_CURVE_WITH_KNOTS ( ( 4, 4 ),
 ( 0.000000000000000000, 0.4074455897393648440 ),
 .UNSPECIFIED. ) 
 CURVE ( )  GEOMETRIC_REPRESENTATION_ITEM ( )  RATIONAL_B_SPLINE_CURVE ( ( 1.000000000000000000, 0.4567392136813316905, 0.3561768502900302114, 0.6983129098260953960 ) ) 
 REPRESENTATION_ITEM ( '' )  );
#18070 = ORIENTED_EDGE ( 'NONE', *, *, #24031, .F. ) ;
#18071 = ORIENTED_EDGE ( 'NONE', *, *, #20670, .F. ) ;
#18072 = ORIENTED_EDGE ( 'NONE', *, *, #30419, .F. ) ;
#18073 = CARTESIAN_POINT ( 'NONE',  ( -22.37985709289073455, -19.82347726015160205, 69.17417989525732480 ) ) ;
#18074 = EDGE_CURVE ( 'NONE', #44032, #15954, #41530, .T. ) ;
#18075 = FACE_OUTER_BOUND ( 'NONE', #12890, .T. ) ;
#18076 = ORIENTED_EDGE ( 'NONE', *, *, #429, .F. ) ;
#18077 = EDGE_LOOP ( 'NONE', ( #8075, #3965, #5721, #941 ) ) ;
#18078 = CARTESIAN_POINT ( 'NONE',  ( -16.81784385650551528, -9.790100578890868377, 49.79778022625163203 ) ) ;
#18079 = AXIS2_PLACEMENT_3D ( 'NONE', #43275, #2134, #10506 ) ;
#18080 = B_SPLINE_CURVE_WITH_KNOTS ( 'NONE', 1,
 ( #8300, #20346 ),
 .UNSPECIFIED., .F., .F.,
 ( 2, 2 ),
 ( 0.000000000000000000, 1.000000000000000000 ),
 .UNSPECIFIED. ) ;
#18081 = CARTESIAN_POINT ( 'NONE',  ( -10.86589828222802545, -17.25666868831298828, 61.34846333097007687 ) ) ;
#18082 = CONICAL_SURFACE ( 'NONE', #37742, 0.5560000000000009379, 0.06981317007976595157 ) ;
#18083 = CARTESIAN_POINT ( 'NONE',  ( -17.09909385650551528, -8.114302828567740988, 52.18300498402516041 ) ) ;
#18084 = EDGE_CURVE ( 'NONE', #18613, #35420, #18020, .T. ) ;
#18085 = AXIS2_PLACEMENT_3D ( 'NONE', #7465, #45136, #25662 ) ;
#18086 = EDGE_LOOP ( 'NONE', ( #33803, #28253, #9627, #5090 ) ) ;
#18087 = DIRECTION ( 'NONE',  ( 1.277734862359329272E-05, 2.482875502418557358E-06, 0.9999999999152874297 ) ) ;
#18088 = EDGE_CURVE ( 'NONE', #12513, #20130, #19542, .T. ) ;
#18089 = FACE_OUTER_BOUND ( 'NONE', #4582, .T. ) ;
#18090 = AXIS2_PLACEMENT_3D ( 'NONE', #30256, #26545, #41821 ) ;
#18091 = FACE_OUTER_BOUND ( 'NONE', #28266, .T. ) ;
#18092 = ORIENTED_EDGE ( 'NONE', *, *, #43249, .T. ) ;
#18093 = FACE_OUTER_BOUND ( 'NONE', #27330, .T. ) ;
#18094 = VERTEX_POINT ( 'NONE', #26761 ) ;
#18095 = EDGE_CURVE ( 'NONE', #42959, #34898, #4803, .T. ) ;
#18096 = CARTESIAN_POINT ( 'NONE',  ( -33.52409385541305653, -25.10920654474410441, 52.29999999999998295 ) ) ;
#18097 = CARTESIAN_POINT ( 'NONE',  ( -15.22116837037893866, -21.50650591823945845, 68.59065000974109694 ) ) ;
#18098 = CARTESIAN_POINT ( 'NONE',  ( -17.51784385541255773, -6.860780111193798270, 51.02154966934632796 ) ) ;
#18099 = VERTEX_POINT ( 'NONE', #4348 ) ;
#18100 = CARTESIAN_POINT ( 'NONE',  ( -14.79207564484453563, -7.839496205118279271, 57.02716913942106913 ) ) ;
#18101 = DIRECTION ( 'NONE',  ( -1.642720032068235908E-15, -0.8949343913984794119, 0.4461977533473619473 ) ) ;
#18102 = EDGE_CURVE ( 'NONE', #26191, #39816, #35908, .T. ) ;
#18103 = DIRECTION ( 'NONE',  ( -1.896855589470121649E-06, -2.136244919983285370E-06, -0.9999999999959192643 ) ) ;
#18104 = CARTESIAN_POINT ( 'NONE',  ( -19.82546683696349277, -21.43766614373956259, 69.23482471120810544 ) ) ;
#18105 = ORIENTED_EDGE ( 'NONE', *, *, #8966, .T. ) ;
#18106 = CARTESIAN_POINT ( 'NONE',  ( -17.42409385541300892, -14.80920654474439502, 75.49999999999994316 ) ) ;
#18107 = CARTESIAN_POINT ( 'NONE',  ( -21.38384743419493361, -20.64229702430353086, 72.81886605551670755 ) ) ;
#18108 = CARTESIAN_POINT ( 'NONE',  ( -21.50786275526073510, -9.062390040748779185, 70.43132511361099546 ) ) ;
#18109 = EDGE_LOOP ( 'NONE', ( #24543, #7926, #19769, #43075 ) ) ;
#18110 = FACE_BOUND ( 'NONE', #42430, .T. ) ;
#18111 = VERTEX_POINT ( 'NONE', #42511 ) ;
#18112 = DIRECTION ( 'NONE',  ( 2.662580029140978055E-06, -1.091441817711415488E-05, 0.9999999999368930359 ) ) ;
#18113 = CARTESIAN_POINT ( 'NONE',  ( -11.45752044641470668, -19.27057170535650954, 71.87181270239314301 ) ) ;
#18114 = CARTESIAN_POINT ( 'NONE',  ( -13.11945872550529835, -9.225962324091906197, 67.67942785705487552 ) ) ;
#18115 = VECTOR ( 'NONE', #4948, 1000.000000000000000 ) ;
#18116 = CARTESIAN_POINT ( 'NONE',  ( -22.63008487438422733, -10.12971324841507581, 70.31178520543817001 ) ) ;
#18117 = ORIENTED_EDGE ( 'NONE', *, *, #8880, .T. ) ;
#18118 = DIRECTION ( 'NONE',  ( 0.09855345062332551698, 0.9951317587989213509, 3.188559572831062401E-08 ) ) ;
#18119 = ORIENTED_EDGE ( 'NONE', *, *, #48610, .F. ) ;
#18120 = CARTESIAN_POINT ( 'NONE',  ( -10.92750371411227128, -11.16255126880030701, 64.26386748351472988 ) ) ;
#18122 = EDGE_CURVE ( 'NONE', #41418, #30144, #31583, .T. ) ;
#18121 = CARTESIAN_POINT ( 'NONE',  ( -23.34440357289541979, -18.54427947304066038, 69.30874357600073665 ) ) ;
#18123 = ORIENTED_EDGE ( 'NONE', *, *, #2846, .F. ) ;
#18124 = DIRECTION ( 'NONE',  ( 1.000000000000000000, 0.000000000000000000, 0.000000000000000000 ) ) ;
#18125 = VECTOR ( 'NONE', #6122, 1000.000000000000000 ) ;
#18126 = EDGE_CURVE ( 'NONE', #39502, #22557, #33543, .T. ) ;
#18127 = CARTESIAN_POINT ( 'NONE',  ( -24.65023673758593148, -12.99629830290576038, 63.01759453279318279 ) ) ;
#18128 = ADVANCED_FACE ( 'NONE', ( #12702, #27720, #8784, #23557, #17538, #35094, #9923, #24940, #8527, #38552, #45955, #12453, #19859, #34859, #36250, #19606, #46683, #12929, #1362, #39957, #12217, #15898, #42750, #1126, #45735, #34612, #43670, #16128, #23305, #24041, #2533, #31174, #39037, #30944, #23800, #38802, #5318, #16627, #26994, #31663, #38295, #4587, #46195, #27477, #5081, #20090, #10644, #44165, #41165, #29355, #25904, #2759, #3739, #17767, #7449, #44386, #22213, #47595, #25652, #6475, #32563, #40666, #33261, #18253, #6949, #10415, #32796, #22455, #21966, #37201, #13828 ), #44880, .T. ) ;
#18129 = ORIENTED_EDGE ( 'NONE', *, *, #24223, .T. ) ;
#18130 = ORIENTED_EDGE ( 'NONE', *, *, #4779, .T. ) ;
#18131 = CARTESIAN_POINT ( 'NONE',  ( -14.90123591195245112, -21.39555782113924209, 65.52085318447059592 ) ) ;
#18132 = CARTESIAN_POINT ( 'NONE',  ( -50.42609385541305755, -14.90920654474411577, 58.00588235294116402 ) ) ;
#18133 = AXIS2_PLACEMENT_3D ( 'NONE', #41064, #10538, #14426 ) ;
#18134 = CARTESIAN_POINT ( 'NONE',  ( -10.50893933415051507, -13.43540278197274063, 74.96345540680638919 ) ) ;
#18135 = DIRECTION ( 'NONE',  ( -0.3478314405900307937, -0.9375570856950865561, 0.000000000000000000 ) ) ;
#18136 = DIRECTION ( 'NONE',  ( 3.413470714839332458E-33, -1.190614954331866791E-16, 1.000000000000000000 ) ) ;
#18137 = FACE_OUTER_BOUND ( 'NONE', #17718, .T. ) ;
#18138 = LINE ( 'NONE', #29727, #37759 ) ;
#18139 = VERTEX_POINT ( 'NONE', #14782 ) ;
#18140 = ORIENTED_EDGE ( 'NONE', *, *, #38869, .T. ) ;
#18141 = B_SPLINE_CURVE_WITH_KNOTS ( 'NONE', 1,
 ( #2192, #24619 ),
 .UNSPECIFIED., .F., .F.,
 ( 2, 2 ),
 ( 0.000000000000000000, 1.000000000000000000 ),
 .UNSPECIFIED. ) ;
#18142 = CARTESIAN_POINT ( 'NONE',  ( -15.92409385541305333, -15.80920654474410725, 47.99999999999998579 ) ) ;
#18143 = CIRCLE ( 'NONE', #45704, 2.000000000000000000 ) ;
#18144 = LINE ( 'NONE', #47487, #8706 ) ;
#18145 = CARTESIAN_POINT ( 'NONE',  ( -21.87050228503520799, -9.402212662412775757, 63.47537209186675256 ) ) ;
#18146 = CARTESIAN_POINT ( 'NONE',  ( -12.46122051107220230, -19.81685944811288635, 64.88146935704573082 ) ) ;
#18147 =( BOUNDED_CURVE ( )  B_SPLINE_CURVE ( 3, ( #5807, #2095, #32146, #29653 ),
 .UNSPECIFIED., .F., .F. ) 
 B_SPLINE_CURVE_WITH_KNOTS ( ( 4, 4 ),
 ( 0.5000000000000000000, 0.9074455897393565174 ),
 .UNSPECIFIED. ) 
 CURVE ( )  GEOMETRIC_REPRESENTATION_ITEM ( )  RATIONAL_B_SPLINE_CURVE ( ( 1.000000000000062395, 0.4567392136813611669, 0.3561768502899974043, 0.6983129098260387746 ) ) 
 REPRESENTATION_ITEM ( '' )  );
#18148 = CARTESIAN_POINT ( 'NONE',  ( -24.40591063191072152, -15.81373627858385866, 73.30303958064588699 ) ) ;
#18149 = ORIENTED_EDGE ( 'NONE', *, *, #26487, .F. ) ;
#18150 = CARTESIAN_POINT ( 'NONE',  ( -18.58659385650551599, -9.302874398569244363, 51.68646062012417985 ) ) ;
#18151 = ORIENTED_EDGE ( 'NONE', *, *, #48000, .T. ) ;
#18152 = VECTOR ( 'NONE', #15671, 1000.000000000000114 ) ;
#18153 = PLANE ( 'NONE',  #30406 ) ;
#18154 = FACE_OUTER_BOUND ( 'NONE', #36156, .T. ) ;
#18155 = VECTOR ( 'NONE', #24809, 1000.000000000000227 ) ;
#18156 = CARTESIAN_POINT ( 'NONE',  ( -11.79904658571650877, -10.55909629022110963, 74.44444907532985667 ) ) ;
#18157 = CARTESIAN_POINT ( 'NONE',  ( -18.20084761934894146, -22.21872609085398764, 65.46719399146324747 ) ) ;
#18158 = ORIENTED_EDGE ( 'NONE', *, *, #2059, .T. ) ;
#18159 = B_SPLINE_CURVE_WITH_KNOTS ( 'NONE', 3,
 ( #31703, #20629, #31457, #30750, #19659, #5619, #16174, #9063, #27281, #4632 ),
 .UNSPECIFIED., .F., .F.,
 ( 4, 2, 2, 2, 4 ),
 ( 0.1272669073658515837, 0.2522669073439512966, 0.3772669073220510372, 0.5022669073001506668, 0.6272669072782504074 ),
 .UNSPECIFIED. ) ;
#18160 = AXIS2_PLACEMENT_3D ( 'NONE', #21530, #17324, #9954 ) ;
#18161 = EDGE_CURVE ( 'NONE', #4839, #21061, #28868, .T. ) ;
#18162 = CARTESIAN_POINT ( 'NONE',  ( -12.14425517392406917, -10.13739710456042964, 64.17914326607970565 ) ) ;
#18163 = CARTESIAN_POINT ( 'NONE',  ( -11.91343869374197695, -19.82283377674160718, 58.04186948019505365 ) ) ;
#18164 = ORIENTED_EDGE ( 'NONE', *, *, #44104, .F. ) ;
#18165 = VECTOR ( 'NONE', #7475, 1000.000000000000000 ) ;
#18166 = CARTESIAN_POINT ( 'NONE',  ( -11.35719102664687874, -18.40077844947705188, 58.09242476654641507 ) ) ;
#18167 = CARTESIAN_POINT ( 'NONE',  ( -16.11395021683892281, -7.881860907381922132, 63.67570853548351550 ) ) ;
#18168 = ORIENTED_EDGE ( 'NONE', *, *, #21422, .F. ) ;
#18169 = CARTESIAN_POINT ( 'NONE',  ( -18.31357640787765462, -21.80286941108919763, 68.81514702304139064 ) ) ;
#18170 = ORIENTED_EDGE ( 'NONE', *, *, #19020, .F. ) ;
#18171 = CARTESIAN_POINT ( 'NONE',  ( -17.42409385541299471, -14.80920654474435594, 52.02966884056656482 ) ) ;
#18172 = CARTESIAN_POINT ( 'NONE',  ( -24.87230691347358302, -14.64571622948453111, 62.91307683260841088 ) ) ;
#18173 = ORIENTED_EDGE ( 'NONE', *, *, #3275, .T. ) ;
#18174 = CARTESIAN_POINT ( 'NONE',  ( -18.42426029547229405, -21.73782819656517873, 72.56894429655113754 ) ) ;
#18175 = VECTOR ( 'NONE', #12250, 1000.000000000000000 ) ;
#18176 = CARTESIAN_POINT ( 'NONE',  ( -10.40277073914389661, -15.44443991871667343, 57.56792809063193772 ) ) ;
#18177 = VERTEX_POINT ( 'NONE', #21496 ) ;
#18178 = CARTESIAN_POINT ( 'NONE',  ( -13.60236376389480384, -20.73382277062339085, 61.80174179654961364 ) ) ;
#18179 = FACE_OUTER_BOUND ( 'NONE', #26918, .T. ) ;
#18180 = CARTESIAN_POINT ( 'NONE',  ( -23.39635208968330105, -11.04794396834914494, 70.04777744521437910 ) ) ;
#18181 = ORIENTED_EDGE ( 'NONE', *, *, #35108, .T. ) ;
#18182 = DIRECTION ( 'NONE',  ( -2.027460363947684990E-06, -1.195255637520530846E-05, 0.9999999999265128947 ) ) ;
#18183 = ADVANCED_FACE ( 'NONE', ( #43913 ), #8024, .T. ) ;
#18184 = CARTESIAN_POINT ( 'NONE',  ( -11.40126873537406205, -11.24191379345135999, 60.97885781058090515 ) ) ;
#18185 = PRESENTATION_LAYER_ASSIGNMENT (  '', '', ( #45756 ) ) ;
#18186 = CARTESIAN_POINT ( 'NONE',  ( -33.52409385541305653, -2.423472813913224222, 48.79999999999998295 ) ) ;
#18187 = EDGE_CURVE ( 'NONE', #39328, #43944, #37157, .T. ) ;
#18188 = EDGE_CURVE ( 'NONE', #4721, #21230, #38182, .T. ) ;
#18189 = ORIENTED_EDGE ( 'NONE', *, *, #6420, .T. ) ;
#18190 = EDGE_LOOP ( 'NONE', ( #14566, #650, #39064, #9856 ) ) ;
#18191 = VECTOR ( 'NONE', #24760, 1000.000000000000000 ) ;
#18192 = CARTESIAN_POINT ( 'NONE',  ( -16.85779285108784009, -7.832151056010677515, 74.06904305648112086 ) ) ;
#18193 = DIRECTION ( 'NONE',  ( -0.2393415023380396633, 0.9709354485539016810, -6.438601123826609832E-08 ) ) ;
#18194 = CARTESIAN_POINT ( 'NONE',  ( -14.28659385759798894, -7.222650657624104298, 49.61879703869476543 ) ) ;
#18195 = PLANE ( 'NONE',  #32106 ) ;
#18196 =( BOUNDED_SURFACE ( )  B_SPLINE_SURFACE ( 3, 1, ( 
 ( #25258, #10483 ),
 ( #3075, #23268 ),
 ( #15358, #45436 ),
 ( #41479, #7772 ),
 ( #27196, #26466 ),
 ( #41980, #8252 ),
 ( #34084, #11690 ) ),
 .UNSPECIFIED., .T., .F., .F. ) 
 B_SPLINE_SURFACE_WITH_KNOTS ( ( 4, 3, 4 ),
 ( 2, 2 ),
 ( 0.000000000000000000, 0.5000000000000000000, 1.000000000000000000 ),
 ( 0.000000000000000000, 1.000000000000000000 ),
 .UNSPECIFIED. ) 
 GEOMETRIC_REPRESENTATION_ITEM ( )  RATIONAL_B_SPLINE_SURFACE ( (
 ( 1.000000000000000000, 1.000000000000000000),
 ( 0.3333333333333335369, 0.3333333333333330373),
 ( 0.3333333333333335369, 0.3333333333333330373),
 ( 1.000000000000000000, 1.000000000000000000),
 ( 0.3333333333333333703, 0.3333333333333333703),
 ( 0.3333333333333333703, 0.3333333333333333703),
 ( 1.000000000000000000, 1.000000000000000000) ) ) 
 REPRESENTATION_ITEM ( '' )  SURFACE ( )  );
#18197 = CARTESIAN_POINT ( 'NONE',  ( -13.89248387370423110, -21.36903859207333412, 71.96961763246901000 ) ) ;
#18198 = CARTESIAN_POINT ( 'NONE',  ( -12.34063849734112850, -9.996720310667569720, 60.55918082403523073 ) ) ;
#18199 = CARTESIAN_POINT ( 'NONE',  ( -10.62027216904274241, -17.84408883714660732, 71.71718193840895594 ) ) ;
#18200 = EDGE_LOOP ( 'NONE', ( #8418, #17851 ) ) ;
#18201 = CARTESIAN_POINT ( 'NONE',  ( -10.01440787728688520, -14.03439562150409969, 61.03325889150411143 ) ) ;
#18202 = CARTESIAN_POINT ( 'NONE',  ( -14.06695675121984301, -8.606427752881131710, 70.61468953885895417 ) ) ;
#18203 = CIRCLE ( 'NONE', #14252, 1.250000000000001110 ) ;
#18204 = CARTESIAN_POINT ( 'NONE',  ( -24.72409385541305582, -14.90920654474426499, 72.98823529411762934 ) ) ;
#18205 = CARTESIAN_POINT ( 'NONE',  ( -10.61641583932764910, -11.78277314028518319, 74.74335662173743344 ) ) ;
#18206 =( BOUNDED_CURVE ( )  B_SPLINE_CURVE ( 3, ( #407, #8513, #11724, #34353 ),
 .UNSPECIFIED., .F., .F. ) 
 B_SPLINE_CURVE_WITH_KNOTS ( ( 4, 4 ),
 ( 0.000000000000000000, 0.4074455897393702841 ),
 .UNSPECIFIED. ) 
 CURVE ( )  GEOMETRIC_REPRESENTATION_ITEM ( )  RATIONAL_B_SPLINE_CURVE ( ( 1.000000000000000000, 0.4567392136813254733, 0.3561768502900278799, 0.6983129098261073864 ) ) 
 REPRESENTATION_ITEM ( '' )  );
#18207 = ORIENTED_EDGE ( 'NONE', *, *, #27152, .T. ) ;
#18208 = VERTEX_POINT ( 'NONE', #14305 ) ;
#18209 = EDGE_CURVE ( 'NONE', #32937, #37435, #27127, .T. ) ;
#18210 = CARTESIAN_POINT ( 'NONE',  ( -17.42409385541306222, -14.80920654474411080, 75.49999999999998579 ) ) ;
#18211 = CARTESIAN_POINT ( 'NONE',  ( -10.71808830285582914, -12.63376213818331628, 61.09853562115718262 ) ) ;
#18212 = CARTESIAN_POINT ( 'NONE',  ( -13.93897074462874919, -20.93787812888889377, 68.74153005185598886 ) ) ;
#18213 = ORIENTED_EDGE ( 'NONE', *, *, #23639, .T. ) ;
#18214 = DIRECTION ( 'NONE',  ( 3.413470714839332458E-33, -1.190614954331866791E-16, 1.000000000000000000 ) ) ;
#18215 = B_SPLINE_CURVE_WITH_KNOTS ( 'NONE', 3,
 ( #34124, #8717, #35033, #12637, #11002, #27659, #5254, #42692, #22568, #45239 ),
 .UNSPECIFIED., .F., .F.,
 ( 4, 2, 2, 2, 4 ),
 ( 0.6272669072877217200, 0.7522669073072643098, 0.8772669073268068995, 1.002266907346349489, 1.127266907365892079 ),
 .UNSPECIFIED. ) ;
#18216 = CARTESIAN_POINT ( 'NONE',  ( -12.52712847051791378, -9.194636617869647921, 74.36277061998997340 ) ) ;
#18217 = ORIENTED_EDGE ( 'NONE', *, *, #23758, .F. ) ;
#18218 = AXIS2_PLACEMENT_3D ( 'NONE', #7398, #14988, #22400 ) ;
#18219 = CARTESIAN_POINT ( 'NONE',  ( -13.63887963148984817, -21.22614835001067490, 68.61771678319368561 ) ) ;
#18220 = CARTESIAN_POINT ( 'NONE',  ( -24.86960059988683014, -14.52975442119237748, 62.82641240410487171 ) ) ;
#18221 = CARTESIAN_POINT ( 'NONE',  ( -23.34288328645119037, -19.33377384263253873, 59.06905932422779415 ) ) ;
#18222 = ORIENTED_EDGE ( 'NONE', *, *, #20900, .F. ) ;
#18223 = CARTESIAN_POINT ( 'NONE',  ( -24.14084320357540747, -12.83654105174326077, 69.78859659034802121 ) ) ;
#18224 = VERTEX_POINT ( 'NONE', #18751 ) ;
#18225 = CARTESIAN_POINT ( 'NONE',  ( -19.50844099596679371, -21.96177777289817357, 62.11008350414853396 ) ) ;
#18226 = CARTESIAN_POINT ( 'NONE',  ( -24.39574017056938615, -14.17912290068383108, 69.93809931784123535 ) ) ;
#18227 = VERTEX_POINT ( 'NONE', #42392 ) ;
#18228 = DIRECTION ( 'NONE',  ( -3.071710424422018668E-17, 6.404604876783312462E-16, 1.000000000000000000 ) ) ;
#18229 = CARTESIAN_POINT ( 'NONE',  ( -24.08517543038346531, -12.49907855475201579, 73.52753481283211556 ) ) ;
#18230 = CARTESIAN_POINT ( 'NONE',  ( -22.33034385650551812, -9.794322478646142471, 51.19202720610083190 ) ) ;
#18231 = B_SPLINE_CURVE_WITH_KNOTS ( 'NONE', 1,
 ( #29738, #44774 ),
 .UNSPECIFIED., .F., .F.,
 ( 2, 2 ),
 ( 0.000000000000000000, 1.000000000000000000 ),
 .UNSPECIFIED. ) ;
#18232 = LINE ( 'NONE', #36941, #1621 ) ;
#18233 = CARTESIAN_POINT ( 'NONE',  ( -10.75331705403316818, -16.93070056221711184, 57.98760548944069626 ) ) ;
#18234 = DIRECTION ( 'NONE',  ( 1.000000000000000000, 1.669677910507523057E-21, 6.493791346278465266E-22 ) ) ;
#18235 = FACE_OUTER_BOUND ( 'NONE', #45788, .T. ) ;
#18236 = ORIENTED_EDGE ( 'NONE', *, *, #47916, .F. ) ;
#18237 = CARTESIAN_POINT ( 'NONE',  ( -24.87106857282577721, -14.59265502392501546, 62.83483757625009503 ) ) ;
#18238 = DIRECTION ( 'NONE',  ( -5.731567514496413899E-31, -1.020425574103664789E-16, -1.000000000000000000 ) ) ;
#18239 = CARTESIAN_POINT ( 'NONE',  ( -17.42409385541299471, -14.80920654474435771, 49.52966884056655772 ) ) ;
#18240 = CARTESIAN_POINT ( 'NONE',  ( -50.42609385541305755, -14.80920654474425291, 71.08235294117645253 ) ) ;
#18241 = CARTESIAN_POINT ( 'NONE',  ( -11.32522400900782067, -11.27219014254736074, 60.96413645226084554 ) ) ;
#18242 = EDGE_CURVE ( 'NONE', #16383, #31039, #30727, .T. ) ;
#18243 = EDGE_LOOP ( 'NONE', ( #45675, #11557 ) ) ;
#18244 = ORIENTED_EDGE ( 'NONE', *, *, #41305, .T. ) ;
#18245 = CARTESIAN_POINT ( 'NONE',  ( -11.31808814922340822, -18.33929587155208552, 61.69199689979424051 ) ) ;
#18246 = CARTESIAN_POINT ( 'NONE',  ( -14.98927377128267047, -8.246306944878837086, 57.14999999999994884 ) ) ;
#18247 = EDGE_LOOP ( 'NONE', ( #5433, #13171, #22930, #40031, #48620 ) ) ;
#18249 = CARTESIAN_POINT ( 'NONE',  ( -12.55411140858086760, -19.90724249994213935, 65.15202838036978505 ) ) ;
#18248 = CARTESIAN_POINT ( 'NONE',  ( -24.11793993921729395, -12.76166543249827434, 70.07243002473258286 ) ) ;
#18250 = DIRECTION ( 'NONE',  ( 1.000000000000000000, -4.164305804376849172E-17, 1.614929280266638808E-16 ) ) ;
#18251 = CARTESIAN_POINT ( 'NONE',  ( 18.46573386768564973, 0.6652513346184721899, 50.77657095919170871 ) ) ;
#18252 = CARTESIAN_POINT ( 'NONE',  ( -22.14851325272248062, -9.572347091288939680, 60.13659902389549927 ) ) ;
#18253 = FACE_BOUND ( 'NONE', #35961, .T. ) ;
#18254 = DIRECTION ( 'NONE',  ( 1.927470528863184130E-16, 1.434740771370715221E-29, -1.000000000000000000 ) ) ;
#18255 = CARTESIAN_POINT ( 'NONE',  ( -10.42462062702805703, -14.89507852762941198, 74.79778901763455679 ) ) ;
#18256 = EDGE_CURVE ( 'NONE', #12881, #2612, #37702, .T. ) ;
#18257 = EDGE_CURVE ( 'NONE', #35003, #454, #27358, .T. ) ;
#18258 = CARTESIAN_POINT ( 'NONE',  ( -24.28619334359350290, -16.42731978468327014, 59.13804568661029037 ) ) ;
#18259 = ORIENTED_EDGE ( 'NONE', *, *, #11815, .F. ) ;
#18260 = CYLINDRICAL_SURFACE ( 'NONE', #15635, 0.1500000000000031586 ) ;
#18261 = CARTESIAN_POINT ( 'NONE',  ( -21.63336539757928634, -9.153348366551478321, 66.94677872351418557 ) ) ;
#18262 = ADVANCED_FACE ( 'NONE', ( #31061 ), #9597, .T. ) ;
#18263 = CARTESIAN_POINT ( 'NONE',  ( -17.04413539470109740, -21.84925844046378174, 72.45071136019464575 ) ) ;
#18264 = EDGE_CURVE ( 'NONE', #26255, #17956, #43243, .T. ) ;
#18265 = CARTESIAN_POINT ( 'NONE',  ( -20.58659385759798965, -7.222650657624104298, 49.61879703869476543 ) ) ;
#18266 = CARTESIAN_POINT ( 'NONE',  ( -28.42409385541305511, -6.359206544744109735, 52.99999999999997158 ) ) ;
#18267 = CARTESIAN_POINT ( 'NONE',  ( -11.89177157637785598, -10.51836466457079844, 74.51055518672704636 ) ) ;
#18268 = CARTESIAN_POINT ( 'NONE',  ( -21.99178428503401861, -9.439038574390064440, 60.02171213140443484 ) ) ;
#18269 = ORIENTED_EDGE ( 'NONE', *, *, #26130, .T. ) ;
#18270 = ORIENTED_EDGE ( 'NONE', *, *, #8960, .F. ) ;
#18271 = CARTESIAN_POINT ( 'NONE',  ( -14.76159385541304303, -7.228003583438117552, 51.38655588711986155 ) ) ;
#18272 = VERTEX_POINT ( 'NONE', #26892 ) ;
#18273 = EDGE_CURVE ( 'NONE', #30917, #29274, #23431, .T. ) ;
#18274 = CARTESIAN_POINT ( 'NONE',  ( -15.69284385759799427, -8.630756214087126565, 51.74842643355248129 ) ) ;
#18275 = CARTESIAN_POINT ( 'NONE',  ( -23.98474799315784978, -17.25007060033011896, 69.41339792561625188 ) ) ;
#18276 = LINE ( 'NONE', #11157, #19821 ) ;
#18277 = CARTESIAN_POINT ( 'NONE',  ( -16.23263389423368963, -22.16407464444966280, 58.39930168947970657 ) ) ;
#18278 = EDGE_LOOP ( 'NONE', ( #47990, #40107, #16328, #28314, #5723 ) ) ;
#18279 = CARTESIAN_POINT ( 'NONE',  ( -13.76849323099554567, -20.83774554052356365, 65.27156739751333703 ) ) ;
#18280 = CARTESIAN_POINT ( 'NONE',  ( -21.06634951290973845, -21.30826427787840771, 62.29966696806321380 ) ) ;
#18281 = ORIENTED_EDGE ( 'NONE', *, *, #9768, .T. ) ;
#18282 = CARTESIAN_POINT ( 'NONE',  ( -18.89909385759798965, -8.105421454601382081, 49.25000573077640098 ) ) ;
#18283 = CARTESIAN_POINT ( 'NONE',  ( -12.94360638298142163, -11.59623166875815237, 53.69233794759168177 ) ) ;
#18284 = ORIENTED_EDGE ( 'NONE', *, *, #24293, .F. ) ;
#18285 = CARTESIAN_POINT ( 'NONE',  ( -17.76896499593897261, -7.367070395244857295, 60.20248019549192975 ) ) ;
#18286 = CARTESIAN_POINT ( 'NONE',  ( -11.09636557211808849, -11.81291458199088495, 74.78669872099975180 ) ) ;
#18287 = CARTESIAN_POINT ( 'NONE',  ( -18.47409385541327964, -6.859212275519742441, 50.50378509014038997 ) ) ;
#18288 = ORIENTED_EDGE ( 'NONE', *, *, #32254, .F. ) ;
#18289 = CARTESIAN_POINT ( 'NONE',  ( -11.95600649777366264, -19.86917281586842066, 58.03344075405964020 ) ) ;
#18290 = PLANE ( 'NONE',  #7704 ) ;
#18291 = EDGE_CURVE ( 'NONE', #45009, #35691, #41873, .T. ) ;
#18292 = FACE_OUTER_BOUND ( 'NONE', #39769, .T. ) ;
#18293 = CARTESIAN_POINT ( 'NONE',  ( -15.34465393633500518, -21.54586957516256263, 68.86120835375241711 ) ) ;
#18294 = EDGE_LOOP ( 'NONE', ( #23987, #3492 ) ) ;
#18295 = CARTESIAN_POINT ( 'NONE',  ( -24.30048588269890431, -16.36411231998812710, 59.12332431758469653 ) ) ;
#18296 = DIRECTION ( 'NONE',  ( -7.623677603559713149E-06, -4.209792907790860808E-06, 0.9999999999620784452 ) ) ;
#18297 = CARTESIAN_POINT ( 'NONE',  ( -17.73224099643095286, -22.30287356026373047, 54.27966884056655061 ) ) ;
#18298 = FACE_OUTER_BOUND ( 'NONE', #17167, .T. ) ;
#18299 = EDGE_CURVE ( 'NONE', #30729, #35243, #21886, .T. ) ;
#18300 = ORIENTED_EDGE ( 'NONE', *, *, #10005, .T. ) ;
#18301 = CARTESIAN_POINT ( 'NONE',  ( -16.46477641927899782, -7.821750181629138154, 60.61517342399707076 ) ) ;
#18302 = DIRECTION ( 'NONE',  ( 0.9687793358424821033, -0.2479245821708677133, 0.000000000000000000 ) ) ;
#18303 = EDGE_LOOP ( 'NONE', ( #17354, #48216, #31563, #32263, #22412 ) ) ;
#18304 = DIRECTION ( 'NONE',  ( -0.5351595679979681552, -0.8447509909909712844, 0.000000000000000000 ) ) ;
#18305 = CARTESIAN_POINT ( 'NONE',  ( -15.37798316477759109, -8.114859020620054153, 74.30658946014833077 ) ) ;
#18306 = CARTESIAN_POINT ( 'NONE',  ( -10.51729459156483237, -16.22293329152201480, 71.59750383216309899 ) ) ;
#18307 = ORIENTED_EDGE ( 'NONE', *, *, #9570, .T. ) ;
#18308 = CARTESIAN_POINT ( 'NONE',  ( -17.63034385541255489, -6.857644439845357986, 49.98602051094380982 ) ) ;
#18309 = DIRECTION ( 'NONE',  ( -1.000000000000000000, 0.000000000000000000, 8.260587980841940012E-17 ) ) ;
#18310 = ORIENTED_EDGE ( 'NONE', *, *, #4432, .F. ) ;
#18311 = ORIENTED_EDGE ( 'NONE', *, *, #26295, .T. ) ;
#18312 = ORIENTED_EDGE ( 'NONE', *, *, #43442, .F. ) ;
#18313 = AXIS2_PLACEMENT_3D ( 'NONE', #27934, #17075, #32125 ) ;
#18314 = CARTESIAN_POINT ( 'NONE',  ( -15.83034385650551634, -9.794322478646142471, 51.19202720610083901 ) ) ;
#18315 = EDGE_CURVE ( 'NONE', #44745, #24840, #48248, .T. ) ;
#18316 = ADVANCED_FACE ( 'NONE', ( #37950 ), #31295, .F. ) ;
#18317 = CARTESIAN_POINT ( 'NONE',  ( -11.25339550917664333, -11.39346175823023088, 60.56396915994215391 ) ) ;
#18318 = CARTESIAN_POINT ( 'NONE',  ( -24.42398663107514523, -15.65075326911586906, 73.01775867260030850 ) ) ;
#18319 = CARTESIAN_POINT ( 'NONE',  ( -24.85291224181648317, -14.24716073839753250, 69.84613574404021108 ) ) ;
#18320 = CARTESIAN_POINT ( 'NONE',  ( -13.71586683582447819, -8.803873544643577631, 60.58383457371648717 ) ) ;
#18321 = EDGE_LOOP ( 'NONE', ( #46817, #32841, #14382, #35919, #18964 ) ) ;
#18322 = ORIENTED_EDGE ( 'NONE', *, *, #40487, .F. ) ;
#18323 = EDGE_CURVE ( 'NONE', #41749, #26170, #39164, .T. ) ;
#18324 = CARTESIAN_POINT ( 'NONE',  ( -13.72409385650551528, -6.426201560718813433, 50.50509628382439331 ) ) ;
#18325 = FACE_OUTER_BOUND ( 'NONE', #2599, .T. ) ;
#18326 = DIRECTION ( 'NONE',  ( -3.071710424422018668E-17, 6.404604876783312462E-16, 1.000000000000000000 ) ) ;
#18327 = EDGE_CURVE ( 'NONE', #10986, #43000, #4539, .T. ) ;
#18328 =( BOUNDED_CURVE ( )  B_SPLINE_CURVE ( 3, ( #26386, #22453, #40664, #10641 ),
 .UNSPECIFIED., .F., .F. ) 
 B_SPLINE_CURVE_WITH_KNOTS ( ( 4, 4 ),
 ( 0.9074455897393624015, 1.000000000000000000 ),
 .UNSPECIFIED. ) 
 CURVE ( )  GEOMETRIC_REPRESENTATION_ITEM ( )  RATIONAL_B_SPLINE_CURVE ( ( 0.6983129098260856260, 0.7760317562606918740, 0.8765941196519966283, 1.000000000000000000 ) ) 
 REPRESENTATION_ITEM ( '' )  );
#18329 = CARTESIAN_POINT ( 'NONE',  ( -14.11784385650551954, -9.790100578890868377, 49.79778022625163203 ) ) ;
#18330 = VERTEX_POINT ( 'NONE', #13049 ) ;
#18331 = CARTESIAN_POINT ( 'NONE',  ( -10.81170448216924740, -12.36318809540519048, 57.34329390664808557 ) ) ;
#18332 = PRODUCT_DEFINITION ( 'UNKNOWN', '', #36852, #19409 ) ;
#18333 = CARTESIAN_POINT ( 'NONE',  ( -45.55409385541305767, -16.70920654474410938, 70.50000000000000000 ) ) ;
#18334 = CARTESIAN_POINT ( 'NONE',  ( -23.55638786360989911, -11.43265490025598119, 70.17594215464632157 ) ) ;
#18335 = VERTEX_POINT ( 'NONE', #42643 ) ;
#18336 =( BOUNDED_SURFACE ( )  B_SPLINE_SURFACE ( 3, 1, ( 
 ( #3092, #33118 ),
 ( #14389, #29447 ),
 ( #44478, #19333 ),
 ( #34340, #8271 ),
 ( #15878, #37294 ),
 ( #628, #4098 ),
 ( #26738, #30682 ) ),
 .UNSPECIFIED., .T., .F., .F. ) 
 B_SPLINE_SURFACE_WITH_KNOTS ( ( 4, 3, 4 ),
 ( 2, 2 ),
 ( 0.000000000000000000, 0.5000000000000000000, 1.000000000000000000 ),
 ( 0.000000000000000000, 1.000000000000000000 ),
 .UNSPECIFIED. ) 
 GEOMETRIC_REPRESENTATION_ITEM ( )  RATIONAL_B_SPLINE_SURFACE ( (
 ( 1.000000000000000000, 1.000000000000000000),
 ( 0.3333333333333335369, 0.3333333333333330373),
 ( 0.3333333333333335369, 0.3333333333333330373),
 ( 1.000000000000000000, 1.000000000000000000),
 ( 0.3333333333333333703, 0.3333333333333333703),
 ( 0.3333333333333333703, 0.3333333333333333703),
 ( 1.000000000000000000, 1.000000000000000000) ) ) 
 REPRESENTATION_ITEM ( '' )  SURFACE ( )  );
#18337 = CARTESIAN_POINT ( 'NONE',  ( -24.47751270253307609, -14.87344405244085443, 63.01296453033411638 ) ) ;
#18338 = B_SPLINE_CURVE_WITH_KNOTS ( 'NONE', 3,
 ( #16219, #5170, #46545, #1457, #12787, #39381, #24124, #9353, #13019, #16469 ),
 .UNSPECIFIED., .F., .F.,
 ( 4, 2, 2, 2, 4 ),
 ( 0.1272669073658746208, 0.2522669073488398861, 0.3772669073318051236, 0.5022669073147704166, 0.6272669072977357096 ),
 .UNSPECIFIED. ) ;
#18339 =( BOUNDED_CURVE ( )  B_SPLINE_CURVE ( 3, ( #15071, #18781, #22480, #26914 ),
 .UNSPECIFIED., .F., .F. ) 
 B_SPLINE_CURVE_WITH_KNOTS ( ( 4, 4 ),
 ( 0.4074455897393629011, 0.5000000000000000000 ),
 .UNSPECIFIED. ) 
 CURVE ( )  GEOMETRIC_REPRESENTATION_ITEM ( )  RATIONAL_B_SPLINE_CURVE ( ( 0.6983129098260921763, 0.7760317562606997566, 0.8765941196520031786, 1.000000000000003775 ) ) 
 REPRESENTATION_ITEM ( '' )  );
#18340 = VERTEX_POINT ( 'NONE', #42871 ) ;
#18341 = B_SPLINE_CURVE_WITH_KNOTS ( 'NONE', 1,
 ( #14207, #6367 ),
 .UNSPECIFIED., .F., .F.,
 ( 2, 2 ),
 ( 0.000000000000000000, 1.000000000000000000 ),
 .UNSPECIFIED. ) ;
#18342 = CARTESIAN_POINT ( 'NONE',  ( -21.31800817620502286, -20.62620158190326336, 72.82446429882371319 ) ) ;
#18343 = DIRECTION ( 'NONE',  ( -3.071710424422018668E-17, 6.404604876783312462E-16, 1.000000000000000000 ) ) ;
#18344 = DIRECTION ( 'NONE',  ( 0.000000000000000000, -1.912410701131276611E-32, -1.000000000000000000 ) ) ;
#18345 = CARTESIAN_POINT ( 'NONE',  ( -10.40918007552567914, -12.30049416576506083, 57.42833712013332814 ) ) ;
#18346 = AXIS2_PLACEMENT_3D ( 'NONE', #19459, #34224, #15753 ) ;
#18347 = ORIENTED_EDGE ( 'NONE', *, *, #20722, .T. ) ;
#18348 = CARTESIAN_POINT ( 'NONE',  ( -23.04367560227575140, -10.55211830211007396, 59.60203429193362012 ) ) ;
#18349 = EDGE_CURVE ( 'NONE', #46160, #48120, #32278, .T. ) ;
#18350 = CARTESIAN_POINT ( 'NONE',  ( -14.49326647312025074, -18.48150914673672673, 52.02966884056656482 ) ) ;
#18351 = CARTESIAN_POINT ( 'NONE',  ( -10.08201403285261577, -16.07297148251123531, 68.17106154205173141 ) ) ;
#18352 = ORIENTED_EDGE ( 'NONE', *, *, #12834, .T. ) ;
#18353 = CARTESIAN_POINT ( 'NONE',  ( -22.66727108289645543, -10.09628893573625064, 70.01178520457129650 ) ) ;
#18354 = DIRECTION ( 'NONE',  ( 0.9477661110324762106, -0.3189661404888857743, 2.738326501554842086E-08 ) ) ;
#18356 =( BOUNDED_CURVE ( )  B_SPLINE_CURVE ( 3, ( #32899, #10520, #17408, #39819 ),
 .UNSPECIFIED., .F., .F. ) 
 B_SPLINE_CURVE_WITH_KNOTS ( ( 4, 4 ),
 ( 0.9074455897393565174, 1.000000000000000000 ),
 .UNSPECIFIED. ) 
 CURVE ( )  GEOMETRIC_REPRESENTATION_ITEM ( )  RATIONAL_B_SPLINE_CURVE ( ( 0.6983129098260613121, 0.7760317562606708908, 0.8765941196519837497, 1.000000000000000000 ) ) 
 REPRESENTATION_ITEM ( '' )  );
#18355 = CARTESIAN_POINT ( 'NONE',  ( -19.05639634586962572, -7.942579960324152921, 70.51501210008177623 ) ) ;
#18357 = VERTEX_POINT ( 'NONE', #47298 ) ;
#18358 = CARTESIAN_POINT ( 'NONE',  ( -6.424093855413055110, -25.10920654474410441, 79.99999999999998579 ) ) ;
#18359 = ORIENTED_EDGE ( 'NONE', *, *, #3689, .F. ) ;
#18360 = CARTESIAN_POINT ( 'NONE',  ( -22.05923648098858791, -20.05472392750071720, 62.23439162613904330 ) ) ;
#18361 = CARTESIAN_POINT ( 'NONE',  ( -13.71154894328531704, -21.26836094557570433, 68.49979187789318757 ) ) ;
#18362 = CARTESIAN_POINT ( 'NONE',  ( -16.93379202924731430, -21.84228538806570796, 72.17103004438159530 ) ) ;
#18363 = CARTESIAN_POINT ( 'NONE',  ( -14.48034385541302527, -9.360768649639460648, 51.01397948905905366 ) ) ;
#18364 = ORIENTED_EDGE ( 'NONE', *, *, #39608, .T. ) ;
#18365 = DIRECTION ( 'NONE',  ( -0.4461977533475101065, -0.8949343913984055821, 2.835129006680928249E-16 ) ) ;
#18366 = ORIENTED_EDGE ( 'NONE', *, *, #41390, .F. ) ;
#18367 = CARTESIAN_POINT ( 'NONE',  ( -22.01615059517208906, -8.856209313517616977, 54.02312124697528617 ) ) ;
#18368 = CARTESIAN_POINT ( 'NONE',  ( -23.30282330091471366, -18.60927750845715067, 69.29371984660140527 ) ) ;
#18369 = ORIENTED_EDGE ( 'NONE', *, *, #45144, .F. ) ;
#18370 = DIRECTION ( 'NONE',  ( -1.000000000000000000, 1.224646799147353207E-16, 5.551115123125782702E-17 ) ) ;
#18371 = CARTESIAN_POINT ( 'NONE',  ( -13.41327670018355001, -20.54622194888242603, 58.34650078082590596 ) ) ;
#18372 = VERTEX_POINT ( 'NONE', #27842 ) ;
#18373 = ORIENTED_EDGE ( 'NONE', *, *, #7164, .F. ) ;
#18374 = CARTESIAN_POINT ( 'NONE',  ( -12.17647495751581133, -14.96730746957505076, 50.77966884056655772 ) ) ;
#18375 = ADVANCED_FACE ( 'NONE', ( #28580 ), #14562, .T. ) ;
#18376 = CARTESIAN_POINT ( 'NONE',  ( -19.11145711862998553, -7.964113067175272676, 63.58089235102941217 ) ) ;
#18377 = CARTESIAN_POINT ( 'NONE',  ( -21.89826263122328953, -8.852228171720549099, 66.84645388252840803 ) ) ;
#18378 = EDGE_CURVE ( 'NONE', #27894, #15973, #24344, .T. ) ;
#18379 = CARTESIAN_POINT ( 'NONE',  ( -17.42409385541300892, -14.80920654474439502, 77.49999999999994316 ) ) ;
#18380 = CARTESIAN_POINT ( 'NONE',  ( -21.19055157706816672, -21.23704344223776985, 65.69179803007084217 ) ) ;
#18381 = CARTESIAN_POINT ( 'NONE',  ( -14.10113443798904065, -8.141252799482343150, 70.98603544959661349 ) ) ;
#18382 = CARTESIAN_POINT ( 'NONE',  ( -17.85433243000881376, -7.371517279143424695, 60.25873515745463038 ) ) ;
#18383 = ORIENTED_EDGE ( 'NONE', *, *, #16596, .F. ) ;
#18384 = ORIENTED_EDGE ( 'NONE', *, *, #41920, .F. ) ;
#18385 = VECTOR ( 'NONE', #32014, 1000.000000000000114 ) ;
#18386 = EDGE_CURVE ( 'NONE', #17101, #12756, #3085, .T. ) ;
#18387 = CARTESIAN_POINT ( 'NONE',  ( -17.00410561000564513, -7.771727611841389383, 74.26018273220857679 ) ) ;
#18388 = AXIS2_PLACEMENT_3D ( 'NONE', #21231, #32069, #16549 ) ;
#18389 = CARTESIAN_POINT ( 'NONE',  ( -24.72409385541305582, -14.90920654474423124, 69.07058823529411029 ) ) ;
#18390 = DIRECTION ( 'NONE',  ( -0.06357898915124172989, 0.9979768094191899808, 0.000000000000000000 ) ) ;
#18391 = CARTESIAN_POINT ( 'NONE',  ( -10.99934536236922611, -17.58926721141864746, 71.58334779160672667 ) ) ;
#18392 = EDGE_CURVE ( 'NONE', #12877, #47438, #13304, .T. ) ;
#18393 = DIRECTION ( 'NONE',  ( 0.1571515419521612722, -0.9875744999047174622, 7.433889655140131751E-08 ) ) ;
#18394 = ORIENTED_EDGE ( 'NONE', *, *, #20722, .F. ) ;
#18395 = CARTESIAN_POINT ( 'NONE',  ( -17.63034385650551528, -9.794322478646142471, 51.19202720610083901 ) ) ;
#18396 = ORIENTED_EDGE ( 'NONE', *, *, #2103, .F. ) ;
#18397 = CARTESIAN_POINT ( 'NONE',  ( -24.33635513415894280, -15.92417079501564459, 69.72234651700993879 ) ) ;
#18398 = DIRECTION ( 'NONE',  ( 5.408674103422956756E-06, -4.460197091461694596E-06, -0.9999999999754264346 ) ) ;
#18399 = CARTESIAN_POINT ( 'NONE',  ( -10.03904583415351581, -13.82694187778184158, 57.56329747881408565 ) ) ;
#18400 = EDGE_CURVE ( 'NONE', #7211, #31812, #1981, .T. ) ;
#18401 = VERTEX_POINT ( 'NONE', #32025 ) ;
#18402 = EDGE_CURVE ( 'NONE', #19923, #4090, #2329, .T. ) ;
#18403 = B_SPLINE_CURVE_WITH_KNOTS ( 'NONE', 1,
 ( #38772, #388 ),
 .UNSPECIFIED., .F., .F.,
 ( 2, 2 ),
 ( 0.000000000000000000, 1.000000000000000000 ),
 .UNSPECIFIED. ) ;
#18404 = CARTESIAN_POINT ( 'NONE',  ( -18.89726480061343494, -7.914800429535790549, 67.20071754334654202 ) ) ;
#18405 = CARTESIAN_POINT ( 'NONE',  ( -19.98813031515369332, -21.37641424997302053, 72.70478737316020101 ) ) ;
#18406 = VERTEX_POINT ( 'NONE', #31784 ) ;
#18407 = CARTESIAN_POINT ( 'NONE',  ( -10.43125892716163960, -13.91323834088958122, 57.44825034920751960 ) ) ;
#18408 = DIRECTION ( 'NONE',  ( 1.000000000000000000, -6.517531090241554163E-16, 3.534154189880001717E-15 ) ) ;
#18409 = ORIENTED_EDGE ( 'NONE', *, *, #3322, .T. ) ;
#18410 = CARTESIAN_POINT ( 'NONE',  ( -10.51950677724785166, -15.96138457174308556, 64.58059568819477647 ) ) ;
#18411 = EDGE_LOOP ( 'NONE', ( #35955, #7622 ) ) ;
#18412 = DIRECTION ( 'NONE',  ( 0.9998756790481365675, 0.01576789294826319576, 3.907472227867916492E-09 ) ) ;
#18413 = DIRECTION ( 'NONE',  ( -0.2479245821708678799, -0.9687793358424819923, -2.626836608253746575E-18 ) ) ;
#18414 = ORIENTED_EDGE ( 'NONE', *, *, #44587, .F. ) ;
#18415 = CARTESIAN_POINT ( 'NONE',  ( -23.98503169607928953, -17.39005800936845603, 66.22885190747201989 ) ) ;
#18416 = AXIS2_PLACEMENT_3D ( 'NONE', #1180, #35870, #46505 ) ;
#18417 = CARTESIAN_POINT ( 'NONE',  ( -18.61312572184442615, -22.16383290914719595, 72.40698155103602573 ) ) ;
#18418 = ORIENTED_EDGE ( 'NONE', *, *, #23706, .F. ) ;
#18419 = CARTESIAN_POINT ( 'NONE',  ( -20.38226146016681994, -7.971588334861294811, 70.36604906519886526 ) ) ;
#18420 = CARTESIAN_POINT ( 'NONE',  ( -19.70791841144649581, -21.90059652173849969, 65.72132139802793915 ) ) ;
#18421 = LINE ( 'NONE', #29771, #4611 ) ;
#18422 = VERTEX_POINT ( 'NONE', #46805 ) ;
#18423 = CARTESIAN_POINT ( 'NONE',  ( -13.46651328273216031, -21.12124922736007449, 65.16441668658305275 ) ) ;
#18424 = CARTESIAN_POINT ( 'NONE',  ( -12.64372748113232703, -9.622537150800651418, 74.52742792958225948 ) ) ;
#18425 = DIRECTION ( 'NONE',  ( 0.04086606279946446846, 0.9938001236776478065, 0.1033986416233887984 ) ) ;
#18426 = VERTEX_POINT ( 'NONE', #28081 ) ;
#18427 = EDGE_LOOP ( 'NONE', ( #35939, #7341, #4497, #10081, #12005 ) ) ;
#18428 = CARTESIAN_POINT ( 'NONE',  ( -22.80070500595625660, -9.652102806524988310, 73.52515182072782807 ) ) ;
#18429 = DIRECTION ( 'NONE',  ( -3.071710424422018668E-17, 6.404604876783312462E-16, 1.000000000000000000 ) ) ;
#18430 = PLANE ( 'NONE',  #16223 ) ;
#18431 =( BOUNDED_CURVE ( )  B_SPLINE_CURVE ( 3, ( #25103, #9843, #36632, #10079 ),
 .UNSPECIFIED., .F., .F. ) 
 B_SPLINE_CURVE_WITH_KNOTS ( ( 4, 4 ),
 ( 0.000000000000000000, 0.4074455897393585158 ),
 .UNSPECIFIED. ) 
 CURVE ( )  GEOMETRIC_REPRESENTATION_ITEM ( )  RATIONAL_B_SPLINE_CURVE ( ( 1.000000000000000000, 0.4567392136813423487, 0.3561768502900341526, 0.6983129098260754120 ) ) 
 REPRESENTATION_ITEM ( '' )  );
#18432 = CARTESIAN_POINT ( 'NONE',  ( -14.62409385759799108, -9.359200813967568422, 50.49621490985803263 ) ) ;
#18433 = CARTESIAN_POINT ( 'NONE',  ( -10.56627932147773308, -16.21290872759732693, 71.74750383609593030 ) ) ;
#18434 = CARTESIAN_POINT ( 'NONE',  ( -12.85387012802420514, -9.430729208696401855, 67.53509681483876648 ) ) ;
#18435 = CARTESIAN_POINT ( 'NONE',  ( -17.19980177718173664, -7.762775310937220397, 70.49035839668022163 ) ) ;
#18436 = B_SPLINE_CURVE_WITH_KNOTS ( 'NONE', 1,
 ( #32231, #37347 ),
 .UNSPECIFIED., .F., .F.,
 ( 2, 2 ),
 ( 0.000000000000000000, 1.000000000000000000 ),
 .UNSPECIFIED. ) ;
#18437 = CARTESIAN_POINT ( 'NONE',  ( -14.76438133403450692, -8.332445847819730744, 63.97905807186954519 ) ) ;
#18438 = EDGE_LOOP ( 'NONE', ( #48191, #22874, #39576, #14997 ) ) ;
#18439 = B_SPLINE_CURVE_WITH_KNOTS ( 'NONE', 3,
 ( #9761, #42996, #20601, #31677, #43739, #5823, #20835, #42766, #28701, #16398 ),
 .UNSPECIFIED., .F., .F.,
 ( 4, 2, 2, 2, 4 ),
 ( 0.1272669073658294903, 0.2522669073463160716, 0.3772669073268026807, 0.5022669073072892898, 0.6272669072877758989 ),
 .UNSPECIFIED. ) ;
#18440 = ADVANCED_FACE ( 'NONE', ( #39652 ), #5923, .F. ) ;
#18441 = CARTESIAN_POINT ( 'NONE',  ( -24.32449541900864176, -13.36385115766270637, 59.36827749005163213 ) ) ;
#18442 =( NAMED_UNIT ( * ) PLANE_ANGLE_UNIT ( ) SI_UNIT ( $, .RADIAN. ) );
#18443 = EDGE_CURVE ( 'NONE', #35820, #22785, #21980, .T. ) ;
#18444 = CARTESIAN_POINT ( 'NONE',  ( -45.92409385541306222, -14.90920654474410867, 70.50000000000000000 ) ) ;
#18445 = CARTESIAN_POINT ( 'NONE',  ( -13.46747565276156422, -9.034678650756244878, 60.73950277887485072 ) ) ;
#18446 = ORIENTED_EDGE ( 'NONE', *, *, #42111, .F. ) ;
#18447 = AXIS2_PLACEMENT_3D ( 'NONE', #7393, #37897, #22643 ) ;
#18448 = ORIENTED_EDGE ( 'NONE', *, *, #15530, .F. ) ;
#18449 = CARTESIAN_POINT ( 'NONE',  ( -17.02358301252079542, -7.369853539629952266, 74.08301376234730640 ) ) ;
#18450 = CIRCLE ( 'NONE', #10596, 1.999999999999994893 ) ;
#18451 = FILL_AREA_STYLE_COLOUR ( '', #921 ) ;
#18452 = CARTESIAN_POINT ( 'NONE',  ( -11.68672710392437608, -10.05669134056747005, 67.68392285705759548 ) ) ;
#18453 = CARTESIAN_POINT ( 'NONE',  ( -15.22116837037893866, -21.50650591823945845, 68.59065000974109694 ) ) ;
#18454 = EDGE_CURVE ( 'NONE', #21691, #29632, #17946, .T. ) ;
#18455 = ORIENTED_EDGE ( 'NONE', *, *, #40850, .T. ) ;
#18456 = EDGE_CURVE ( 'NONE', #29639, #31825, #22773, .T. ) ;
#18457 = CARTESIAN_POINT ( 'NONE',  ( -23.59266626310239090, -11.50006285152738705, 66.72214495366867482 ) ) ;
#18458 = CARTESIAN_POINT ( 'NONE',  ( -11.16004581379495342, -11.56782820372427167, 64.03393219759587396 ) ) ;
#18459 = ADVANCED_FACE ( 'NONE', ( #44563 ), #6165, .T. ) ;
#18460 = ADVANCED_FACE ( 'NONE', ( #14716 ), #19646, .T. ) ;
#18461 = ADVANCED_FACE ( 'NONE', ( #32963 ), #40087, .T. ) ;
#18462 = ORIENTED_EDGE ( 'NONE', *, *, #19280, .F. ) ;
#18463 = DIRECTION ( 'NONE',  ( -5.731567514496413899E-31, -1.020425574103664789E-16, -1.000000000000000000 ) ) ;
#18464 = CARTESIAN_POINT ( 'NONE',  ( -10.90314314408274399, -12.12021994783307299, 74.76660409782968486 ) ) ;
#18465 = CARTESIAN_POINT ( 'NONE',  ( -10.43125892716163960, -13.91323834088957945, 57.44825034920751960 ) ) ;
#18466 = ORIENTED_EDGE ( 'NONE', *, *, #25989, .T. ) ;
#18467 = CARTESIAN_POINT ( 'NONE',  ( -21.77427962766001812, -9.323007061219151126, 66.85077123041597247 ) ) ;
#18468 = EDGE_LOOP ( 'NONE', ( #4731, #42395, #18925, #6654, #30341 ) ) ;
#18469 = CARTESIAN_POINT ( 'NONE',  ( -22.37499513144005903, -19.83249348569362880, 73.05889139438880875 ) ) ;
#18470 = ORIENTED_EDGE ( 'NONE', *, *, #37251, .F. ) ;
#18471 = DIRECTION ( 'NONE',  ( -1.653275063147722522E-06, 1.135554159962570470E-05, 0.9999999999341591117 ) ) ;
#18472 = CARTESIAN_POINT ( 'NONE',  ( -20.24909385650551386, -8.104110260919579645, 48.81699501597546487 ) ) ;
#18473 = FACE_OUTER_BOUND ( 'NONE', #32664, .T. ) ;
#18474 = B_SPLINE_CURVE_WITH_KNOTS ( 'NONE', 3,
 ( #1357, #46191, #23550, #42746, #31895, #12696, #38797, #39285, #15894, #39034 ),
 .UNSPECIFIED., .F., .F.,
 ( 4, 2, 2, 2, 4 ),
 ( 0.000000000000000000, 0.2500000000000000000, 0.5000000000000000000, 0.7500000000000000000, 1.000000000000000000 ),
 .UNSPECIFIED. ) ;
#18475 =( BOUNDED_CURVE ( )  B_SPLINE_CURVE ( 2, ( #14923, #26277, #45255, #11498, #15663, #911, #27004, #38072, #38305 ),
 .UNSPECIFIED., .F., .F. ) 
 B_SPLINE_CURVE_WITH_KNOTS ( ( 3, 2, 2, 2, 3 ),
 ( 0.02753876536673079828, 0.02852216368270100999, 0.02950556199867122517, 0.03048896031464144035, 0.03147235863061165206 ),
 .UNSPECIFIED. ) 
 CURVE ( )  GEOMETRIC_REPRESENTATION_ITEM ( )  RATIONAL_B_SPLINE_CURVE ( ( 0.9999999999995842215, 0.9238795325117025170, 1.000000000000000000, 0.9238795325112867385, 1.000000000000000000, 0.9238795325112867385, 1.000000000000000000, 0.9238795325112867385, 1.000000000000000000 ) ) 
 REPRESENTATION_ITEM ( '' )  );
#18476 = CARTESIAN_POINT ( 'NONE',  ( -46.29409385541305255, -14.20920654474410760, 69.94787228701220272 ) ) ;
#18477 = CARTESIAN_POINT ( 'NONE',  ( -14.97188219925329378, -8.199429090594037461, 56.99999999999994316 ) ) ;
#18478 = FACE_OUTER_BOUND ( 'NONE', #46579, .T. ) ;
#18479 = ORIENTED_EDGE ( 'NONE', *, *, #35978, .F. ) ;
#18480 = CARTESIAN_POINT ( 'NONE',  ( -12.14425528403576848, -10.13739698163135117, 64.02914326607979945 ) ) ;
#18481 = CARTESIAN_POINT ( 'NONE',  ( -9.990623107247818879, -14.31192343302863179, 64.57299167182827659 ) ) ;
#18482 = CARTESIAN_POINT ( 'NONE',  ( -14.43654735092019514, -7.984457654175056263, 63.98967627971388339 ) ) ;
#18483 = CARTESIAN_POINT ( 'NONE',  ( -23.56697050129053750, -18.27597851715990984, 72.97187965531796294 ) ) ;
#18484 = CARTESIAN_POINT ( 'NONE',  ( -10.79744546256606341, -12.55229233887115114, 61.08236992542625643 ) ) ;
#18485 = CARTESIAN_POINT ( 'NONE',  ( -17.12463553450013265, -7.815553531953688626, 70.77570529858661530 ) ) ;
#18486 = EDGE_CURVE ( 'NONE', #5788, #26302, #42401, .T. ) ;
#18487 = AXIS2_PLACEMENT_3D ( 'NONE', #33749, #41393, #37433 ) ;
#18488 = ORIENTED_EDGE ( 'NONE', *, *, #10210, .T. ) ;
#18489 = ORIENTED_EDGE ( 'NONE', *, *, #13927, .F. ) ;
#18490 = DIRECTION ( 'NONE',  ( -3.071710424422018668E-17, 6.404604876783312462E-16, 1.000000000000000000 ) ) ;
#18491 = CARTESIAN_POINT ( 'NONE',  ( -17.69678476813674095, -21.85754569590755736, 61.96715964058037684 ) ) ;
#18492 = ORIENTED_EDGE ( 'NONE', *, *, #38689, .T. ) ;
#18494 = CARTESIAN_POINT ( 'NONE',  ( -10.11824970337647223, -16.26811690260224452, 71.56254994910038647 ) ) ;
#18493 = FACE_OUTER_BOUND ( 'NONE', #42799, .T. ) ;
#18495 = CARTESIAN_POINT ( 'NONE',  ( -13.30711473254145716, -9.147892019113847084, 63.90946529584681457 ) ) ;
#18496 = CARTESIAN_POINT ( 'NONE',  ( -12.44869033171645611, -9.885248809711741913, 57.38935532200543577 ) ) ;
#18497 = CARTESIAN_POINT ( 'NONE',  ( -14.91789657710648598, -21.40191547797545724, 58.05129291223532562 ) ) ;
#18498 = B_SPLINE_CURVE_WITH_KNOTS ( 'NONE', 3,
 ( #18377, #43545, #9809, #24821, #40080, #26768, #27000, #22331, #11990, #37575 ),
 .UNSPECIFIED., .F., .F.,
 ( 4, 2, 2, 2, 4 ),
 ( 0.6272669072877582463, 0.7522669073072830725, 0.8772669073268077877, 1.002266907346332614, 1.127266907365857440 ),
 .UNSPECIFIED. ) ;
#18499 = CARTESIAN_POINT ( 'NONE',  ( -24.38811251953670478, -14.09928673046249159, 73.12271532470063562 ) ) ;
#18500 = CARTESIAN_POINT ( 'NONE',  ( -11.43009896910331413, -19.23352928037464693, 71.88697091451700771 ) ) ;
#18501 =( BOUNDED_CURVE ( )  B_SPLINE_CURVE ( 3, ( #19287, #15824, #8707, #23004 ),
 .UNSPECIFIED., .F., .F. ) 
 B_SPLINE_CURVE_WITH_KNOTS ( ( 4, 4 ),
 ( 0.4074455897393687853, 0.5000000000000000000 ),
 .UNSPECIFIED. ) 
 CURVE ( )  GEOMETRIC_REPRESENTATION_ITEM ( )  RATIONAL_B_SPLINE_CURVE ( ( 0.6983129098261011691, 0.7760317562606855457, 0.8765941196519793088, 0.9999999999999688027 ) ) 
 REPRESENTATION_ITEM ( '' )  );
#18502 = CARTESIAN_POINT ( 'NONE',  ( -10.42413886794138556, -14.85581422461645396, 75.09778936447564490 ) ) ;
#18503 = PRODUCT_DEFINITION_SHAPE ( 'NONE', 'NONE',  #48739 ) ;
#18504 = CARTESIAN_POINT ( 'NONE',  ( -16.19813999035177332, -21.75179513556690480, 58.28585572029249562 ) ) ;
#18505 = EDGE_LOOP ( 'NONE', ( #44178, #40351, #37662, #21100, #25276 ) ) ;
#18506 = CARTESIAN_POINT ( 'NONE',  ( -20.31413516131974717, -8.378470924821744603, 67.06632013881642251 ) ) ;
#18507 = CARTESIAN_POINT ( 'NONE',  ( -11.46876066122178095, -18.48806595306161071, 61.57710833523393035 ) ) ;
#18508 = ADVANCED_FACE ( 'NONE', ( #6409 ), #24688, .T. ) ;
#18509 = LINE ( 'NONE', #35826, #6655 ) ;
#18510 = CARTESIAN_POINT ( 'NONE',  ( -24.27556694116850977, -13.13524334109580671, 66.71735578995932769 ) ) ;
#18511 = CARTESIAN_POINT ( 'NONE',  ( -16.58751391467172098, -21.80939466075598077, 65.52564390317479592 ) ) ;
#18512 = CARTESIAN_POINT ( 'NONE',  ( -12.10369268100898132, -9.594121713099781346, 57.27430968559156810 ) ) ;
#18513 = ORIENTED_EDGE ( 'NONE', *, *, #34751, .T. ) ;
#18514 = ORIENTED_EDGE ( 'NONE', *, *, #34209, .T. ) ;
#18515 = CARTESIAN_POINT ( 'NONE',  ( -13.52409385541304410, -9.359200813967568422, 50.49621490985803263 ) ) ;
#18516 = ORIENTED_EDGE ( 'NONE', *, *, #35444, .T. ) ;
#18517 = CARTESIAN_POINT ( 'NONE',  ( -17.02397506063647015, -21.79788470884169627, 72.46543205081314909 ) ) ;
#18518 = CARTESIAN_POINT ( 'NONE',  ( -10.43949455435184603, -13.84896052950683298, 57.46297163929641982 ) ) ;
#18519 = CIRCLE ( 'NONE', #2011, 2.000000000000001776 ) ;
#18520 = CARTESIAN_POINT ( 'NONE',  ( -15.39459761884875100, -7.640960489892825613, 74.27996863187141230 ) ) ;
#18521 = ADVANCED_FACE ( 'NONE', ( #44820 ), #29709, .T. ) ;
#18522 = EDGE_CURVE ( 'NONE', #10266, #10553, #22411, .T. ) ;
#18523 = DIRECTION ( 'NONE',  ( 0.5589780652556124441, -0.8291824422665291516, 7.938832475108296738E-08 ) ) ;
#18524 = VERTEX_POINT ( 'NONE', #45307 ) ;
#18525 = CARTESIAN_POINT ( 'NONE',  ( -23.12987884181161391, -10.01876350439231977, 66.71995018326251170 ) ) ;
#18526 = DIRECTION ( 'NONE',  ( -1.277734862951525411E-05, -2.482875507175237739E-06, -0.9999999999152874297 ) ) ;
#18527 = VERTEX_POINT ( 'NONE', #8123 ) ;
#18528 = CARTESIAN_POINT ( 'NONE',  ( -22.32518170918469380, -20.42023717105881175, 62.41251914304209691 ) ) ;
#18529 = CARTESIAN_POINT ( 'NONE',  ( -24.43362379028604536, -14.05489247495133753, 73.12271507725591846 ) ) ;
#18530 = ORIENTED_EDGE ( 'NONE', *, *, #39104, .T. ) ;
#18531 = EDGE_CURVE ( 'NONE', #14429, #13748, #42453, .T. ) ;
#18532 = ADVANCED_FACE ( 'NONE', ( #7392 ), #13011, .T. ) ;
#18533 = CARTESIAN_POINT ( 'NONE',  ( -19.62622408449249178, -21.50961356628077326, 61.88014844347227950 ) ) ;
#18534 = CARTESIAN_POINT ( 'NONE',  ( -15.38020936669038008, -6.822612233742264110, 53.49999999999995026 ) ) ;
#18535 = CARTESIAN_POINT ( 'NONE',  ( -9.982716954774490503, -14.44908413001617298, 67.97304700561097945 ) ) ;
#18536 = ORIENTED_EDGE ( 'NONE', *, *, #2914, .T. ) ;
#18537 = CARTESIAN_POINT ( 'NONE',  ( -24.22092373047179237, -12.93688097883364385, 66.30246741375938768 ) ) ;
#18538 = CARTESIAN_POINT ( 'NONE',  ( -24.72409385541305582, -14.90920654474427565, 73.09411764705880898 ) ) ;
#18539 = CARTESIAN_POINT ( 'NONE',  ( -14.97037710525490262, -21.36678034756659272, 65.29523681788728595 ) ) ;
#18540 = CARTESIAN_POINT ( 'NONE',  ( -21.89264518680100835, -20.26253109894388160, 58.77915004610761684 ) ) ;
#18541 = ORIENTED_EDGE ( 'NONE', *, *, #44676, .T. ) ;
#18542 = CARTESIAN_POINT ( 'NONE',  ( -10.96921284960095555, -11.97350354382807680, 74.84368195529052059 ) ) ;
#18543 = LINE ( 'NONE', #14342, #13263 ) ;
#18544 = CARTESIAN_POINT ( 'NONE',  ( -24.72409385541305582, -14.80920654474428488, 74.99999999999998579 ) ) ;
#18545 = CARTESIAN_POINT ( 'NONE',  ( -17.20812589326699182, -22.32442570159451734, 54.02312124697527906 ) ) ;
#18546 = CARTESIAN_POINT ( 'NONE',  ( -18.98034385650551670, -6.424090610841176385, 49.80797279389978627 ) ) ;
#18547 = EDGE_CURVE ( 'NONE', #8929, #35456, #18037, .T. ) ;
#18548 = VERTEX_POINT ( 'NONE', #45070 ) ;
#18549 = CARTESIAN_POINT ( 'NONE',  ( -17.71634532009226248, -22.25352164097983376, 58.59891670633793126 ) ) ;
#18550 = CARTESIAN_POINT ( 'NONE',  ( 10.57590614458695377, 2.137037847100790255, 51.75577699556767897 ) ) ;
#18551 = ORIENTED_EDGE ( 'NONE', *, *, #24588, .F. ) ;
#18552 = DIRECTION ( 'NONE',  ( -0.9524241471993248886, 0.0009228828802118167144, -0.3047743298226213704 ) ) ;
#18553 = CARTESIAN_POINT ( 'NONE',  ( -22.49805058420730219, -9.986866540729424813, 73.78161091687563555 ) ) ;
#18554 = CARTESIAN_POINT ( 'NONE',  ( -11.68672710392437608, -10.05669134056747005, 67.68392285705759548 ) ) ;
#18555 = EDGE_LOOP ( 'NONE', ( #23422, #34609, #28211, #44690, #4781 ) ) ;
#18556 = DIRECTION ( 'NONE',  ( 0.000000000000000000, 0.000000000000000000, 1.000000000000000000 ) ) ;
#18557 = CIRCLE ( 'NONE', #26450, 1.250000000000001110 ) ;
#18558 = DIRECTION ( 'NONE',  ( -0.9930145540378111368, 0.1179919296777755672, 4.526730167978065139E-08 ) ) ;
#18559 = ORIENTED_EDGE ( 'NONE', *, *, #42892, .T. ) ;
#18560 = ORIENTED_EDGE ( 'NONE', *, *, #10235, .T. ) ;
#18561 = CARTESIAN_POINT ( 'NONE',  ( -15.99909385650551741, -8.114302828567740988, 52.18300498402516041 ) ) ;
#18562 = CARTESIAN_POINT ( 'NONE',  ( -11.36795091080559850, -18.31963851737709348, 58.10714594516144871 ) ) ;
#18563 = DIRECTION ( 'NONE',  ( 1.000000000000000000, -4.164305804376849172E-17, 1.614929280266638808E-16 ) ) ;
#18564 = CARTESIAN_POINT ( 'NONE',  ( -14.02588861851693380, -8.179183006140712919, 70.88991002814806563 ) ) ;
#18565 = LINE ( 'NONE', #19069, #15744 ) ;
#18566 = ORIENTED_EDGE ( 'NONE', *, *, #42891, .T. ) ;
#18567 = VERTEX_POINT ( 'NONE', #31003 ) ;
#18568 = CARTESIAN_POINT ( 'NONE',  ( -15.58034385650551634, -6.424090610841176385, 49.80797279389977916 ) ) ;
#18569 = CARTESIAN_POINT ( 'NONE',  ( -11.45716883000597086, -10.34844295181603790, 74.63896264531059899 ) ) ;
#18570 = DIRECTION ( 'NONE',  ( 0.000000000000000000, 0.007114381193220381018, -0.9999746924698831307 ) ) ;
#18571 = CARTESIAN_POINT ( 'NONE',  ( -15.41159385650551705, -6.922745924619793101, 51.69366785382590024 ) ) ;
#18572 = VERTEX_POINT ( 'NONE', #3677 ) ;
#18573 = EDGE_CURVE ( 'NONE', #15587, #29512, #27627, .T. ) ;
#18574 = CARTESIAN_POINT ( 'NONE',  ( -16.59344707466788549, -21.75974795715521282, 65.52564390620075585 ) ) ;
#18575 = CARTESIAN_POINT ( 'NONE',  ( -13.79242041809915875, -8.303469675591347965, 74.31299407998417905 ) ) ;
#18576 = CYLINDRICAL_SURFACE ( 'NONE', #17042, 0.1500000000000017708 ) ;
#18577 = VERTEX_POINT ( 'NONE', #41344 ) ;
#18578 = CARTESIAN_POINT ( 'NONE',  ( -9.905916914905521509, -14.85586088411330330, 53.76227901944321985 ) ) ;
#18579 = CIRCLE ( 'NONE', #33550, 0.5000000000000004441 ) ;
#18580 = AXIS2_PLACEMENT_3D ( 'NONE', #5708, #32039, #5936 ) ;
#18581 = ORIENTED_EDGE ( 'NONE', *, *, #26864, .F. ) ;
#18582 = EDGE_CURVE ( 'NONE', #4090, #18227, #34431, .T. ) ;
#18583 = CARTESIAN_POINT ( 'NONE',  ( -12.58530871590044242, -9.144360103953445673, 74.49735781771244092 ) ) ;
#18584 = CARTESIAN_POINT ( 'NONE',  ( -24.82831796749689701, -13.98412716734901373, 73.31545655147931484 ) ) ;
#18585 = CARTESIAN_POINT ( 'NONE',  ( -17.90106345612152694, -14.65920654474411045, 52.21286476528345588 ) ) ;
#18586 = ADVANCED_FACE ( 'NONE', ( #7637 ), #33690, .T. ) ;
#18587 = ORIENTED_EDGE ( 'NONE', *, *, #15351, .F. ) ;
#18588 = CARTESIAN_POINT ( 'NONE',  ( -13.71073213066623531, -18.52046572475128983, 50.77966884056655772 ) ) ;
#18589 = DIRECTION ( 'NONE',  ( -0.8017593358536259096, -0.5976470257363776240, 1.209213344977627713E-07 ) ) ;
#18590 = AXIS2_PLACEMENT_3D ( 'NONE', #8812, #46222, #31925 ) ;
#18591 = EDGE_CURVE ( 'NONE', #12927, #27084, #42085, .T. ) ;
#18592 = FACE_OUTER_BOUND ( 'NONE', #25602, .T. ) ;
#18593 = CARTESIAN_POINT ( 'NONE',  ( -10.08052675126636721, -16.06451543208143917, 68.09272439531302723 ) ) ;
#18594 = ORIENTED_EDGE ( 'NONE', *, *, #5745, .F. ) ;
#18595 = CARTESIAN_POINT ( 'NONE',  ( -10.55417862675165175, -17.69166933648559592, 68.21909214388388421 ) ) ;
#18596 = CARTESIAN_POINT ( 'NONE',  ( -17.20086775249401612, -7.362538796574944477, 70.59061584993096972 ) ) ;
#18597 = CARTESIAN_POINT ( 'NONE',  ( -10.73745268310985246, -11.52390413789708568, 71.21143970991980154 ) ) ;
#18598 = FACE_BOUND ( 'NONE', #28636, .T. ) ;
#18599 = ORIENTED_EDGE ( 'NONE', *, *, #19543, .T. ) ;
#18600 = CARTESIAN_POINT ( 'NONE',  ( -18.24684318355141599, -9.624075539355221309, 49.52966884056655772 ) ) ;
#18601 = DIRECTION ( 'NONE',  ( 1.000000000000000000, 2.866981220435670867E-17, -3.652049423109068320E-16 ) ) ;
#18602 = CARTESIAN_POINT ( 'NONE',  ( -16.78865379391102408, -21.78030513117466072, 68.69560651887046276 ) ) ;
#18603 = CARTESIAN_POINT ( 'NONE',  ( -16.02724665508026192, -7.491242618400526077, 63.78515750052793010 ) ) ;
#18604 = EDGE_LOOP ( 'NONE', ( #17242, #40639, #47470, #48370, #44223 ) ) ;
#18605 = CARTESIAN_POINT ( 'NONE',  ( -10.44762891037015962, -14.23035630910777627, 64.67187305841532918 ) ) ;
#18606 = ORIENTED_EDGE ( 'NONE', *, *, #14082, .F. ) ;
#18607 = CARTESIAN_POINT ( 'NONE',  ( -12.23358651314992152, -10.11189197570513443, 64.04530931701648910 ) ) ;
#18608 = CARTESIAN_POINT ( 'NONE',  ( -23.56138404952065457, -11.33988834032952830, 70.19210750372964469 ) ) ;
#18609 = CARTESIAN_POINT ( 'NONE',  ( -7.424093855413048892, -25.10920654474410441, 56.99999999999997868 ) ) ;
#18610 = VERTEX_POINT ( 'NONE', #31962 ) ;
#18611 = CARTESIAN_POINT ( 'NONE',  ( -12.91576191806997542, -9.388722997169708151, 71.13453240065665284 ) ) ;
#18612 = FACE_OUTER_BOUND ( 'NONE', #10511, .T. ) ;
#18613 = VERTEX_POINT ( 'NONE', #35642 ) ;
#18614 = EDGE_LOOP ( 'NONE', ( #35236, #4012 ) ) ;
#18615 = VERTEX_POINT ( 'NONE', #42329 ) ;
#18616 = CARTESIAN_POINT ( 'NONE',  ( -41.18104770156690364, -14.90920654474428630, 72.94436923076921175 ) ) ;
#18617 = DIRECTION ( 'NONE',  ( 0.9163203205182085531, 0.4004460890125010053, -2.380681616944615956E-09 ) ) ;
#18618 = DIRECTION ( 'NONE',  ( 2.866981220435666553E-17, -1.000000000000000000, -1.190614954331866791E-16 ) ) ;
#18619 = CARTESIAN_POINT ( 'NONE',  ( -46.47622156840087371, -14.20920654474410760, 70.43449436244988249 ) ) ;
#18620 =( BOUNDED_CURVE ( )  B_SPLINE_CURVE ( 3, ( #14411, #13936, #39824, #28512 ),
 .UNSPECIFIED., .F., .F. ) 
 B_SPLINE_CURVE_WITH_KNOTS ( ( 4, 4 ),
 ( 0.4074455897393655102, 0.5000000000000000000 ),
 .UNSPECIFIED. ) 
 CURVE ( )  GEOMETRIC_REPRESENTATION_ITEM ( )  RATIONAL_B_SPLINE_CURVE ( ( 0.6983129098261007250, 0.7760317562606782182, 0.8765941196519702050, 0.9999999999999577005 ) ) 
 REPRESENTATION_ITEM ( '' )  );
#18621 = DIRECTION ( 'NONE',  ( -3.071710424422018668E-17, 6.404604876783312462E-16, 1.000000000000000000 ) ) ;
#18622 = CARTESIAN_POINT ( 'NONE',  ( -14.19282086353638839, -8.542981675383003903, 71.01485553001869278 ) ) ;
#18623 = CARTESIAN_POINT ( 'NONE',  ( -12.99284385759799143, -8.630756214087126565, 51.74842643355248129 ) ) ;
#18624 = CIRCLE ( 'NONE', #43037, 2.000000000000000444 ) ;
#18625 = ORIENTED_EDGE ( 'NONE', *, *, #9822, .T. ) ;
#18626 = VERTEX_POINT ( 'NONE', #8849 ) ;
#18627 = CARTESIAN_POINT ( 'NONE',  ( -17.63706249495991685, -7.362172851917661909, 63.80702937774674410 ) ) ;
#18628 = CARTESIAN_POINT ( 'NONE',  ( -11.87301334638075545, -9.840320147444462151, 64.20727067481126937 ) ) ;
#18629 = CARTESIAN_POINT ( 'NONE',  ( -45.37196614242555626, -14.20920654474410760, 70.87000000000000455 ) ) ;
#18630 = VECTOR ( 'NONE', #41430, 1000.000000000000000 ) ;
#18631 = CARTESIAN_POINT ( 'NONE',  ( -18.53201708017407157, -7.846807123103141102, 74.14064401780549929 ) ) ;
#18632 = ORIENTED_EDGE ( 'NONE', *, *, #20786, .T. ) ;
#18633 = ADVANCED_FACE ( 'NONE', ( #9087 ), #1191, .F. ) ;
#18634 =( BOUNDED_SURFACE ( )  B_SPLINE_SURFACE ( 3, 1, ( 
 ( #19227, #34229 ),
 ( #15504, #42123 ),
 ( #30570, #15999 ),
 ( #8162, #46059 ),
 ( #27098, #8391 ),
 ( #31276, #12800 ),
 ( #1962, #23905 ) ),
 .UNSPECIFIED., .T., .F., .F. ) 
 B_SPLINE_SURFACE_WITH_KNOTS ( ( 4, 3, 4 ),
 ( 2, 2 ),
 ( 0.000000000000000000, 0.5000000000000000000, 1.000000000000000000 ),
 ( 0.000000000000000000, 1.000000000000000000 ),
 .UNSPECIFIED. ) 
 GEOMETRIC_REPRESENTATION_ITEM ( )  RATIONAL_B_SPLINE_SURFACE ( (
 ( 1.000000000000000000, 1.000000000000000000),
 ( 0.3333333333333335369, 0.3333333333333330373),
 ( 0.3333333333333335369, 0.3333333333333330373),
 ( 1.000000000000000000, 1.000000000000000000),
 ( 0.3333333333333333703, 0.3333333333333333703),
 ( 0.3333333333333333703, 0.3333333333333333703),
 ( 1.000000000000000000, 1.000000000000000000) ) ) 
 REPRESENTATION_ITEM ( '' )  SURFACE ( )  );
#18635 = CARTESIAN_POINT ( 'NONE',  ( -14.87409385650551741, -9.792211528768504536, 50.49490371617623197 ) ) ;
#18636 =( BOUNDED_SURFACE ( )  B_SPLINE_SURFACE ( 3, 1, ( 
 ( #7763, #14123 ),
 ( #3315, #26215 ),
 ( #18317, #22780 ),
 ( #26459, #32851 ),
 ( #25479, #36774 ),
 ( #45190, #7515 ),
 ( #3064, #14600 ) ),
 .UNSPECIFIED., .T., .F., .F. ) 
 B_SPLINE_SURFACE_WITH_KNOTS ( ( 4, 3, 4 ),
 ( 2, 2 ),
 ( 0.000000000000000000, 0.5000000000000000000, 1.000000000000000000 ),
 ( 0.000000000000000000, 1.000000000000000000 ),
 .UNSPECIFIED. ) 
 GEOMETRIC_REPRESENTATION_ITEM ( )  RATIONAL_B_SPLINE_SURFACE ( (
 ( 1.000000000000000000, 1.000000000000000000),
 ( 0.3333333333333335369, 0.3333333333333330373),
 ( 0.3333333333333335369, 0.3333333333333330373),
 ( 1.000000000000000000, 1.000000000000000000),
 ( 0.3333333333333333703, 0.3333333333333333703),
 ( 0.3333333333333333703, 0.3333333333333333703),
 ( 1.000000000000000000, 1.000000000000000000) ) ) 
 REPRESENTATION_ITEM ( '' )  SURFACE ( )  );
#18637 = VERTEX_POINT ( 'NONE', #16687 ) ;
#18638 = FACE_OUTER_BOUND ( 'NONE', #35195, .T. ) ;
#18639 = FACE_OUTER_BOUND ( 'NONE', #27559, .T. ) ;
#18640 = CARTESIAN_POINT ( 'NONE',  ( -15.17058493111871975, -21.43790244863053118, 68.80422765957334263 ) ) ;
#18641 = ORIENTED_EDGE ( 'NONE', *, *, #28789, .F. ) ;
#18642 = B_SPLINE_CURVE_WITH_KNOTS ( 'NONE', 3,
 ( #33233, #40178, #2732, #40891, #47796, #21467, #29085, #29567, #21224, #44597 ),
 .UNSPECIFIED., .F., .F.,
 ( 4, 2, 2, 2, 4 ),
 ( 0.6272669072877683494, 0.7522669073072896229, 0.8772669073268110074, 1.002266907346332392, 1.127266907365853665 ),
 .UNSPECIFIED. ) ;
#18643 = DIRECTION ( 'NONE',  ( 3.071710424422018668E-17, -6.404604876783312462E-16, -1.000000000000000000 ) ) ;
#18644 =( BOUNDED_CURVE ( )  B_SPLINE_CURVE ( 2, ( #24494, #2716, #17723, #26595, #11824, #34206, #41359, #45809, #41616 ),
 .UNSPECIFIED., .F., .F. ) 
 B_SPLINE_CURVE_WITH_KNOTS ( ( 3, 2, 2, 2, 3 ),
 ( 0.07081306277049698172, 0.07179665212962056675, 0.07278024148874416566, 0.07376383084786776456, 0.07474742020699134959 ),
 .UNSPECIFIED. ) 
 CURVE ( )  GEOMETRIC_REPRESENTATION_ITEM ( )  RATIONAL_B_SPLINE_CURVE ( ( 0.9999999999999642508, 0.9238795325113224877, 1.000000000000000000, 0.9238795325112867385, 1.000000000000000000, 0.9238795325112867385, 1.000000000000000000, 0.9238795325101858413, 1.000000000001100897 ) ) 
 REPRESENTATION_ITEM ( '' )  );
#18645 = CARTESIAN_POINT ( 'NONE',  ( -10.52207825420198439, -16.24630393939493800, 71.74750352243894724 ) ) ;
#18646 = DIRECTION ( 'NONE',  ( 0.9294853595766542353, 0.3688590060343623911, 0.000000000000000000 ) ) ;
#18647 = EDGE_CURVE ( 'NONE', #24138, #8953, #12769, .T. ) ;
#18648 = ORIENTED_EDGE ( 'NONE', *, *, #22229, .F. ) ;
#18649 = CARTESIAN_POINT ( 'NONE',  ( -18.70336468933619045, -7.876203269624392433, 70.67067999151545621 ) ) ;
#18650 = EDGE_CURVE ( 'NONE', #28963, #26610, #12520, .T. ) ;
#18651 = CARTESIAN_POINT ( 'NONE',  ( -10.47910621644337326, -16.03883162486972935, 64.39282756246913664 ) ) ;
#18652 = DIRECTION ( 'NONE',  ( -5.731567514496413899E-31, -1.020425574103664789E-16, -1.000000000000000000 ) ) ;
#18653 = EDGE_LOOP ( 'NONE', ( #19887, #10230, #19608, #7769 ) ) ;
#18654 = CARTESIAN_POINT ( 'NONE',  ( -10.52199164562254197, -15.97581925089275678, 64.61657531926886122 ) ) ;
#18655 = AXIS2_PLACEMENT_3D ( 'NONE', #9816, #21617, #47712 ) ;
#18656 = VECTOR ( 'NONE', #19029, 1000.000000000000000 ) ;
#18657 = VERTEX_POINT ( 'NONE', #27783 ) ;
#18658 = CARTESIAN_POINT ( 'NONE',  ( -24.47412807302115212, -14.81851119574499975, 59.54300240094892160 ) ) ;
#18659 = CARTESIAN_POINT ( 'NONE',  ( -19.17988342541450209, -7.569006731055750947, 63.62363369258376622 ) ) ;
#18660 = EDGE_CURVE ( 'NONE', #14479, #41118, #3953, .T. ) ;
#18661 = VERTEX_POINT ( 'NONE', #46750 ) ;
#18662 = CARTESIAN_POINT ( 'NONE',  ( -12.95651447042595095, -9.351591191262567548, 67.26453940287311184 ) ) ;
#18663 = DIRECTION ( 'NONE',  ( 0.5351595679979623821, 0.8447509909909748371, 0.000000000000000000 ) ) ;
#18664 = ORIENTED_EDGE ( 'NONE', *, *, #2839, .T. ) ;
#18665 = CARTESIAN_POINT ( 'NONE',  ( -21.44147796085869118, -20.54162532479978509, 72.63332330819365268 ) ) ;
#18666 = AXIS2_PLACEMENT_3D ( 'NONE', #43641, #20979, #39691 ) ;
#18667 = EDGE_CURVE ( 'NONE', #6775, #42405, #23106, .T. ) ;
#18668 = CARTESIAN_POINT ( 'NONE',  ( -12.77013062424865630, -8.927826924028671840, 54.27966884056655061 ) ) ;
#18669 = CARTESIAN_POINT ( 'NONE',  ( -10.89657404688168363, -17.34179118677383613, 68.20794932300812263 ) ) ;
#18670 = ORIENTED_EDGE ( 'NONE', *, *, #30494, .F. ) ;
#18671 = CARTESIAN_POINT ( 'NONE',  ( -17.79108452803360763, -21.84994637594637368, 58.69081321602850920 ) ) ;
#18672 = CARTESIAN_POINT ( 'NONE',  ( -11.74108458883011963, -23.16273580036827440, 54.49999999999995026 ) ) ;
#18673 = FACE_OUTER_BOUND ( 'NONE', #13816, .T. ) ;
#18674 = EDGE_LOOP ( 'NONE', ( #17254, #38269, #15792, #134, #25571 ) ) ;
#18675 = ORIENTED_EDGE ( 'NONE', *, *, #19302, .F. ) ;
#18676 = DIRECTION ( 'NONE',  ( -1.423524324494147398E-15, 0.8949343913984055821, 0.4461977533475100510 ) ) ;
#18677 = CARTESIAN_POINT ( 'NONE',  ( -19.51784385759798468, -6.860780111191484565, 51.02154966934377711 ) ) ;
#18678 = CARTESIAN_POINT ( 'NONE',  ( -23.24415167771102020, -18.79314401478295338, 62.23918030722157368 ) ) ;
#18679 = CARTESIAN_POINT ( 'NONE',  ( -13.71073213066623531, -18.52046572475128983, 52.02966884056656482 ) ) ;
#18680 = CARTESIAN_POINT ( 'NONE',  ( -16.03034385759799108, -6.857644439848013640, 49.98602051094139398 ) ) ;
#18681 = CARTESIAN_POINT ( 'NONE',  ( -24.84263255441417328, -14.11714595057820354, 73.30926835346492965 ) ) ;
#18682 = CARTESIAN_POINT ( 'NONE',  ( -11.42587710518540334, -11.10406226247761019, 57.49431069621225276 ) ) ;
#18683 = CARTESIAN_POINT ( 'NONE',  ( -16.93697101831087792, -7.375022458023401839, 74.13735168198904546 ) ) ;
#18684 = CARTESIAN_POINT ( 'NONE',  ( -16.49697044570162774, -22.20142030250349663, 65.34847517160625330 ) ) ;
#18685 = ORIENTED_EDGE ( 'NONE', *, *, #24449, .F. ) ;
#18686 = FACE_OUTER_BOUND ( 'NONE', #46808, .T. ) ;
#18687 = B_SPLINE_CURVE_WITH_KNOTS ( 'NONE', 3,
 ( #37475, #44652, #45152, #4023, #10913, #19028, #25933, #7233, #48575, #22238 ),
 .UNSPECIFIED., .F., .F.,
 ( 4, 2, 2, 2, 4 ),
 ( 0.000000000000000000, 0.2500000000000000000, 0.5000000000000000000, 0.7500000000000000000, 1.000000000000000000 ),
 .UNSPECIFIED. ) ;
#18688 = CARTESIAN_POINT ( 'NONE',  ( -14.03871066829747249, -8.172719617054283958, 70.91452941929576070 ) ) ;
#18689 = PLANE ( 'NONE',  #37415 ) ;
#18690 = DIRECTION ( 'NONE',  ( 6.865757730863489906E-07, 1.412849154798944614E-06, 0.9999999999987662092 ) ) ;
#18691 = EDGE_CURVE ( 'NONE', #26808, #26269, #42813, .T. ) ;
#18692 = AXIS2_PLACEMENT_3D ( 'NONE', #17812, #17085, #24520 ) ;
#18693 = ORIENTED_EDGE ( 'NONE', *, *, #41061, .F. ) ;
#18694 = VECTOR ( 'NONE', #629, 1000.000000000000000 ) ;
#18695 = ORIENTED_EDGE ( 'NONE', *, *, #18963, .T. ) ;
#18696 = CARTESIAN_POINT ( 'NONE',  ( -16.99059232606724734, -7.371822389834469469, 74.16029473639015634 ) ) ;
#18697 = DIRECTION ( 'NONE',  ( 0.9999247414263408018, -0.01226831216845470154, -5.367905339470937357E-08 ) ) ;
#18698 = B_SPLINE_CURVE_WITH_KNOTS ( 'NONE', 3,
 ( #12280, #5389, #28525, #32455, #25539, #24824, #2412, #17423, #36130, #31963 ),
 .UNSPECIFIED., .F., .F.,
 ( 4, 2, 2, 2, 4 ),
 ( 0.1272669073658538319, 0.2522669073463127409, 0.3772669073267717055, 0.5022669073072305590, 0.6272669072876895235 ),
 .UNSPECIFIED. ) ;
#18699 = CARTESIAN_POINT ( 'NONE',  ( -15.55648817577099585, -8.010769314271311003, 74.09457776258329886 ) ) ;
#18700 = CARTESIAN_POINT ( 'NONE',  ( -13.81866929095069096, -21.32886163922821154, 72.08754233397257849 ) ) ;
#18701 = VECTOR ( 'NONE', #13335, 1000.000000000000114 ) ;
#18702 = ORIENTED_EDGE ( 'NONE', *, *, #27553, .F. ) ;
#18703 = EDGE_CURVE ( 'NONE', #39770, #41197, #31470, .T. ) ;
#18704 = AXIS2_PLACEMENT_3D ( 'NONE', #17285, #6218, #35997 ) ;
#18705 = CARTESIAN_POINT ( 'NONE',  ( -13.58233848012166511, -8.897862878211833859, 57.26967725704754741 ) ) ;
#18706 = CARTESIAN_POINT ( 'NONE',  ( -14.73037927113499812, -8.285490617698924254, 67.40407820626249702 ) ) ;
#18707 = ORIENTED_EDGE ( 'NONE', *, *, #42284, .F. ) ;
#18708 = DIRECTION ( 'NONE',  ( -0.9524241471993249997, -0.3047743298226212039, -0.0009228828802129951337 ) ) ;
#18709 = CARTESIAN_POINT ( 'NONE',  ( -17.42409385541300182, -14.80920654474440745, 52.02966884056655061 ) ) ;
#18710 = CARTESIAN_POINT ( 'NONE',  ( -24.38756562526642213, -15.91227465074932290, 66.34852784166324113 ) ) ;
#18711 = ORIENTED_EDGE ( 'NONE', *, *, #46041, .F. ) ;
#18712 = CARTESIAN_POINT ( 'NONE',  ( -12.20424117383341311, -20.12491952255346206, 65.12320790045656338 ) ) ;
#18713 = ORIENTED_EDGE ( 'NONE', *, *, #13490, .F. ) ;
#18714 = CARTESIAN_POINT ( 'NONE',  ( -19.57699507595987143, -21.94144279212693860, 62.17998934563075153 ) ) ;
#18715 = EDGE_CURVE ( 'NONE', #18422, #32374, #35164, .T. ) ;
#18716 = CARTESIAN_POINT ( 'NONE',  ( -20.40606020541642707, -8.476062491149917832, 63.38409570189014630 ) ) ;
#18717 = ORIENTED_EDGE ( 'NONE', *, *, #33265, .T. ) ;
#18718 = DIRECTION ( 'NONE',  ( 0.9687793358424821033, -0.2479245821708680464, 0.000000000000000000 ) ) ;
#18719 = CARTESIAN_POINT ( 'NONE',  ( -16.78411710364782650, -21.83009890335197767, 68.99560651669348488 ) ) ;
#18720 = CARTESIAN_POINT ( 'NONE',  ( -20.75534385650551528, -7.417179338643134834, 52.18511593390279302 ) ) ;
#18721 = EDGE_CURVE ( 'NONE', #30644, #46754, #31728, .T. ) ;
#18722 = AXIS2_PLACEMENT_3D ( 'NONE', #45460, #634, #11717 ) ;
#18723 = DIRECTION ( 'NONE',  ( 3.549360974551883545E-17, -6.371834667872732552E-18, -1.000000000000000000 ) ) ;
#18724 =( BOUNDED_SURFACE ( )  B_SPLINE_SURFACE ( 3, 1, ( 
 ( #36278, #6736 ),
 ( #13850, #28660 ),
 ( #43693, #10914 ),
 ( #25211, #33286 ),
 ( #40233, #21750 ),
 ( #6502, #18035 ),
 ( #14090, #18280 ) ),
 .UNSPECIFIED., .T., .F., .F. ) 
 B_SPLINE_SURFACE_WITH_KNOTS ( ( 4, 3, 4 ),
 ( 2, 2 ),
 ( 0.000000000000000000, 0.5000000000000000000, 1.000000000000000000 ),
 ( 0.000000000000000000, 1.000000000000000000 ),
 .UNSPECIFIED. ) 
 GEOMETRIC_REPRESENTATION_ITEM ( )  RATIONAL_B_SPLINE_SURFACE ( (
 ( 1.000000000000000000, 1.000000000000000000),
 ( 0.3333333333333335369, 0.3333333333333330373),
 ( 0.3333333333333335369, 0.3333333333333330373),
 ( 1.000000000000000000, 1.000000000000000000),
 ( 0.3333333333333333703, 0.3333333333333333703),
 ( 0.3333333333333333703, 0.3333333333333333703),
 ( 1.000000000000000000, 1.000000000000000000) ) ) 
 REPRESENTATION_ITEM ( '' )  SURFACE ( )  );
#18725 = EDGE_CURVE ( 'NONE', #10981, #38205, #26496, .T. ) ;
#18726 = AXIS2_PLACEMENT_3D ( 'NONE', #18813, #33823, #15103 ) ;
#18727 = CARTESIAN_POINT ( 'NONE',  ( -10.06068050546405246, -15.94284296925492939, 64.64625047982192996 ) ) ;
#18728 = CARTESIAN_POINT ( 'NONE',  ( -22.52409385541004383, -9.359200813967481380, 50.49621490983041383 ) ) ;
#18729 = CARTESIAN_POINT ( 'NONE',  ( -15.75291993497911136, -20.06326719075875076, 53.69233794759168177 ) ) ;
#18730 = EDGE_LOOP ( 'NONE', ( #10487, #39015 ) ) ;
#18731 = CARTESIAN_POINT ( 'NONE',  ( -22.46784385541121054, -9.357632978284044611, 49.97845033064507447 ) ) ;
#18732 = VECTOR ( 'NONE', #39, 1000.000000000000000 ) ;
#18733 = VECTOR ( 'NONE', #28970, 1000.000000000000000 ) ;
#18734 = DIRECTION ( 'NONE',  ( 0.4461977533473615032, -0.8949343913984796339, 0.000000000000000000 ) ) ;
#18735 = CARTESIAN_POINT ( 'NONE',  ( -12.55411140858086760, -19.90724249994213935, 65.15202838036978505 ) ) ;
#18736 = DIRECTION ( 'NONE',  ( -6.312331220146435760E-07, -6.220915576521675503E-06, -0.9999999999804509709 ) ) ;
#18737 = DIRECTION ( 'NONE',  ( -1.916827911674356108E-06, -6.156520247306097078E-06, 0.9999999999792114069 ) ) ;
#18738 = CARTESIAN_POINT ( 'NONE',  ( -24.18450351543707555, -12.99348042298125883, 62.94150088911103325 ) ) ;
#18739 = VERTEX_POINT ( 'NONE', #5640 ) ;
#18740 = VERTEX_POINT ( 'NONE', #16926 ) ;
#18741 = DIRECTION ( 'NONE',  ( 0.9687793358424821033, -0.2479245821708677133, 0.000000000000000000 ) ) ;
#18742 = CARTESIAN_POINT ( 'NONE',  ( -9.975704095843513031, -14.64835857301500255, 71.45065776245529321 ) ) ;
#18743 = VERTEX_POINT ( 'NONE', #38870 ) ;
#18745 = CARTESIAN_POINT ( 'NONE',  ( -12.72364920584387349, -9.064356868646193277, 49.69365772853683438 ) ) ;
#18744 = CARTESIAN_POINT ( 'NONE',  ( -15.39793084389211764, -7.640011784162778596, 74.18011415750440563 ) ) ;
#18746 = CARTESIAN_POINT ( 'NONE',  ( -11.30083408395673317, -18.20384969151142940, 58.03544514041180946 ) ) ;
#18747 = AXIS2_PLACEMENT_3D ( 'NONE', #25034, #5839, #13679 ) ;
#18748 = CARTESIAN_POINT ( 'NONE',  ( -14.30855566557790404, -8.484641631233271752, 70.74429704309763167 ) ) ;
#18749 = CARTESIAN_POINT ( 'NONE',  ( -21.83505603848428933, -9.305730678460758298, 59.60682523891489382 ) ) ;
#18750 = ADVANCED_FACE ( 'NONE', ( #42587 ), #28124, .T. ) ;
#18751 = CARTESIAN_POINT ( 'NONE',  ( -15.87557863975121819, -7.931372594209569193, 67.14007279017359053 ) ) ;
#18752 = CYLINDRICAL_SURFACE ( 'NONE', #23156, 4.686499999999997002 ) ;
#18753 = EDGE_CURVE ( 'NONE', #37481, #35750, #15707, .T. ) ;
#18754 = CARTESIAN_POINT ( 'NONE',  ( -23.88415217903648724, -17.63235132829416685, 62.77360984996715842 ) ) ;
#18755 = CARTESIAN_POINT ( 'NONE',  ( -16.63927388632151505, -21.76668874189256542, 68.80633768154915231 ) ) ;
#18756 = DIRECTION ( 'NONE',  ( 1.274157597653189794E-05, 2.329884815184971665E-06, -0.9999999999161119923 ) ) ;
#18757 = EDGE_CURVE ( 'NONE', #40480, #17650, #5307, .T. ) ;
#18758 = ADVANCED_FACE ( 'NONE', ( #9811 ), #25065, .T. ) ;
#18759 = ORIENTED_EDGE ( 'NONE', *, *, #44878, .T. ) ;
#18760 = DIRECTION ( 'NONE',  ( 0.9753750245375037986, 0.2205528542287732707, 7.244220459260263973E-08 ) ) ;
#18761 = CARTESIAN_POINT ( 'NONE',  ( -10.25416474409032652, -12.78293385988982678, 67.92487701448251869 ) ) ;
#18762 = DIRECTION ( 'NONE',  ( 3.071710424422018668E-17, -6.404604876783312462E-16, -1.000000000000000000 ) ) ;
#18763 = CARTESIAN_POINT ( 'NONE',  ( -11.13733870171179596, -11.61806121328041996, 67.90392505421056057 ) ) ;
#18764 = CARTESIAN_POINT ( 'NONE',  ( -21.99213670719075253, -20.17946569659695299, 59.04970794435396897 ) ) ;
#18765 = CARTESIAN_POINT ( 'NONE',  ( -14.47717485532954029, -21.65240259781455023, 58.35273132940589136 ) ) ;
#18766 = CARTESIAN_POINT ( 'NONE',  ( -18.19389323530821301, -22.21941482433020809, 65.53027461949925225 ) ) ;
#18767 = ORIENTED_EDGE ( 'NONE', *, *, #25485, .F. ) ;
#18768 = ORIENTED_EDGE ( 'NONE', *, *, #45101, .F. ) ;
#18769 = SURFACE_SIDE_STYLE ('',( #37464 ) ) ;
#18770 = B_SPLINE_CURVE_WITH_KNOTS ( 'NONE', 3,
 ( #22895, #8844, #11546, #45791, #38359, #23621, #4400, #34920, #30997, #19674 ),
 .UNSPECIFIED., .F., .F.,
 ( 4, 2, 2, 2, 4 ),
 ( 0.000000000000000000, 0.2500000000000000000, 0.5000000000000000000, 0.7500000000000000000, 1.000000000000000000 ),
 .UNSPECIFIED. ) ;
#18771 = ORIENTED_EDGE ( 'NONE', *, *, #40228, .T. ) ;
#18772 = CARTESIAN_POINT ( 'NONE',  ( -17.05964169383668150, -21.79977244010465753, 72.18045664228594660 ) ) ;
#18773 = AXIS2_PLACEMENT_3D ( 'NONE', #32318, #28615, #35740 ) ;
#18774 = CARTESIAN_POINT ( 'NONE',  ( -24.72409385541305582, -14.80920654474410902, 57.89999999999999147 ) ) ;
#18775 = FACE_OUTER_BOUND ( 'NONE', #18109, .T. ) ;
#18776 = EDGE_CURVE ( 'NONE', #93, #18791, #29240, .T. ) ;
#18777 = CARTESIAN_POINT ( 'NONE',  ( -17.99631655628617466, -7.779455715877602984, 60.49549448422539655 ) ) ;
#18778 = ORIENTED_EDGE ( 'NONE', *, *, #5549, .F. ) ;
#18779 = FACE_BOUND ( 'NONE', #26205, .T. ) ;
#18780 = AXIS2_PLACEMENT_3D ( 'NONE', #39692, #21227, #43643 ) ;
#18781 = CARTESIAN_POINT ( 'NONE',  ( -21.85939164964043613, -9.329133344058289978, 63.19153770872092224 ) ) ;
#18782 = ORIENTED_EDGE ( 'NONE', *, *, #25344, .F. ) ;
#18783 =( BOUNDED_CURVE ( )  B_SPLINE_CURVE ( 3, ( #45138, #11381, #21389, #27129 ),
 .UNSPECIFIED., .F., .F. ) 
 B_SPLINE_CURVE_WITH_KNOTS ( ( 4, 4 ),
 ( 0.5000000000000000000, 0.9074455897393582937 ),
 .UNSPECIFIED. ) 
 CURVE ( )  GEOMETRIC_REPRESENTATION_ITEM ( )  RATIONAL_B_SPLINE_CURVE ( ( 0.9999999999999932276, 0.4567392136813395176, 0.3561768502900377054, 0.6983129098260805190 ) ) 
 REPRESENTATION_ITEM ( '' )  );
#18784 = CARTESIAN_POINT ( 'NONE',  ( -19.06784385759798894, -9.357632978295834292, 49.97845033065683396 ) ) ;
#18785 = CARTESIAN_POINT ( 'NONE',  ( -23.75674853543430842, -11.71073052589263774, 62.95218282383657993 ) ) ;
#18786 = VERTEX_POINT ( 'NONE', #39834 ) ;
#18787 = DIRECTION ( 'NONE',  ( 0.7915359335728471279, 0.6111226275167354061, 5.146443701300904349E-08 ) ) ;
#18788 = CYLINDRICAL_SURFACE ( 'NONE', #40114, 4.686499999999997002 ) ;
#18789 = EDGE_CURVE ( 'NONE', #46893, #9283, #22934, .T. ) ;
#18790 = CARTESIAN_POINT ( 'NONE',  ( -12.93827254315284669, -9.365655574729560229, 67.37942539479081461 ) ) ;
#18791 = VERTEX_POINT ( 'NONE', #40083 ) ;
#18792 = CARTESIAN_POINT ( 'NONE',  ( -10.60714174419670464, -13.01136550127550606, 68.03832326220812377 ) ) ;
#18793 = DIRECTION ( 'NONE',  ( 0.9811758422909350186, 0.1931164583992469597, 7.863147543881891826E-08 ) ) ;
#18794 = CARTESIAN_POINT ( 'NONE',  ( -24.27133562072960871, -13.11802050994479707, 59.24779033130878503 ) ) ;
#18795 = DIRECTION ( 'NONE',  ( -0.5327540375067998379, -0.8462701315302333382, -7.203825861310614672E-08 ) ) ;
#18796 = ORIENTED_EDGE ( 'NONE', *, *, #15362, .T. ) ;
#18797 = CARTESIAN_POINT ( 'NONE',  ( -24.31477923169101629, -16.30090137217950641, 59.40860294853779777 ) ) ;
#18798 = CARTESIAN_POINT ( 'NONE',  ( -12.20309422964675150, -20.12380354524033521, 64.98179449731530610 ) ) ;
#18800 =( BOUNDED_CURVE ( )  B_SPLINE_CURVE ( 3, ( #34389, #677, #4145, #15922 ),
 .UNSPECIFIED., .F., .F. ) 
 B_SPLINE_CURVE_WITH_KNOTS ( ( 4, 4 ),
 ( 0.5000000000000000000, 0.9074455897393631787 ),
 .UNSPECIFIED. ) 
 CURVE ( )  GEOMETRIC_REPRESENTATION_ITEM ( )  RATIONAL_B_SPLINE_CURVE ( ( 0.9999999999999981126, 0.4567392136813338555, 0.3561768502900322098, 0.6983129098260911771 ) ) 
 REPRESENTATION_ITEM ( '' )  );
#18799 = CARTESIAN_POINT ( 'NONE',  ( -15.44651063079976794, -21.52416795175674835, 72.34575487467760979 ) ) ;
#18801 = CARTESIAN_POINT ( 'NONE',  ( -19.09526777584694202, -9.555145898730048160, 53.69233794759168887 ) ) ;
#18802 = CARTESIAN_POINT ( 'NONE',  ( -16.16063032598464133, -7.467038112641824377, 60.38523865926408263 ) ) ;
#18803 = LINE ( 'NONE', #8226, #37785 ) ;
#18804 = CARTESIAN_POINT ( 'NONE',  ( -19.14909385650551954, -8.104110260919579645, 48.81699501597546487 ) ) ;
#18805 = ORIENTED_EDGE ( 'NONE', *, *, #34007, .F. ) ;
#18806 = VECTOR ( 'NONE', #20430, 1000.000000000000000 ) ;
#18807 = DIRECTION ( 'NONE',  ( 0.4683180279402422430, -0.8835599723313412035, 4.589753183357165928E-08 ) ) ;
#18808 = CARTESIAN_POINT ( 'NONE',  ( -14.54749350918765671, -8.372447261038937327, 64.07506791522041567 ) ) ;
#18809 = ORIENTED_EDGE ( 'NONE', *, *, #1937, .F. ) ;
#18810 = CARTESIAN_POINT ( 'NONE',  ( -27.42409385541305156, -25.10920654474410441, 47.99999999999997868 ) ) ;
#18811 = PRODUCT_DEFINITION_FORMATION_WITH_SPECIFIED_SOURCE ( 'ANY', '', #23692, .NOT_KNOWN. ) ;
#18812 = CARTESIAN_POINT ( 'NONE',  ( -15.46800725202396265, -8.087938728663994326, 74.07985622482316046 ) ) ;
#18813 = CARTESIAN_POINT ( 'NONE',  ( -24.45670955521185164, -12.20012290887857098, 53.49999999999995026 ) ) ;
#18814 = VERTEX_POINT ( 'NONE', #44278 ) ;
#18815 = LINE ( 'NONE', #839, #46740 ) ;
#18816 = CIRCLE ( 'NONE', #43972, 2.000000000000001776 ) ;
#18817 = AXIS2_PLACEMENT_3D ( 'NONE', #31341, #5965, #5498 ) ;
#18818 = EDGE_CURVE ( 'NONE', #45931, #36781, #40020, .T. ) ;
#18819 = CARTESIAN_POINT ( 'NONE',  ( -10.00368807899092971, -15.89896712085359098, 53.49999999999994316 ) ) ;
#18820 = EDGE_CURVE ( 'NONE', #12407, #34367, #32684, .T. ) ;
#18821 = ADVANCED_FACE ( 'NONE', ( #13942 ), #25784, .T. ) ;
#18822 = ORIENTED_EDGE ( 'NONE', *, *, #48257, .T. ) ;
#18823 = CARTESIAN_POINT ( 'NONE',  ( -15.71784385650551741, -9.790100578890868377, 49.79778022625163203 ) ) ;
#18824 = AXIS2_PLACEMENT_3D ( 'NONE', #19536, #4286, #8955 ) ;
#18825 = CARTESIAN_POINT ( 'NONE',  ( -18.84975023778164172, -7.496717724788733328, 70.53214580459695071 ) ) ;
#18826 = CARTESIAN_POINT ( 'NONE',  ( -24.79900369310859531, -15.86464144874165072, 69.72645810305080261 ) ) ;
#18827 = CARTESIAN_POINT ( 'NONE',  ( -24.84985713749398073, -14.20864767979305121, 69.85264054281394408 ) ) ;
#18828 = CARTESIAN_POINT ( 'NONE',  ( -13.56484994756444173, -8.969080399747948462, 56.98470132832054702 ) ) ;
#18829 = ORIENTED_EDGE ( 'NONE', *, *, #12180, .F. ) ;
#18830 = EDGE_LOOP ( 'NONE', ( #7809, #19861, #28938, #36874 ) ) ;
#18831 = EDGE_CURVE ( 'NONE', #41762, #21252, #7086, .T. ) ;
#18832 = CARTESIAN_POINT ( 'NONE',  ( -16.03034385650551386, -9.794322478646142471, 51.19202720610083901 ) ) ;
#18833 = LINE ( 'NONE', #38021, #46538 ) ;
#18834 = DIRECTION ( 'NONE',  ( -1.274157596560980788E-05, -2.329884826735012561E-06, 0.9999999999161118813 ) ) ;
#18835 = CARTESIAN_POINT ( 'NONE',  ( -15.63659385650551670, -6.915538690918075382, 49.31353937987644542 ) ) ;
#18836 = VERTEX_POINT ( 'NONE', #47232 ) ;
#18837 = EDGE_CURVE ( 'NONE', #37616, #946, #8890, .T. ) ;
#18838 = FACE_OUTER_BOUND ( 'NONE', #8547, .T. ) ;
#18839 = VECTOR ( 'NONE', #21999, 1000.000000000000000 ) ;
#18840 = CARTESIAN_POINT ( 'NONE',  ( -13.85393748347032528, -8.270264590973253505, 74.38449983516251507 ) ) ;
#18841 = FACE_OUTER_BOUND ( 'NONE', #15709, .T. ) ;
#18842 = CARTESIAN_POINT ( 'NONE',  ( -11.17943887680513981, -18.87220427245064513, 65.00353025264104190 ) ) ;
#18843 = ORIENTED_EDGE ( 'NONE', *, *, #26341, .F. ) ;
#18844 = CARTESIAN_POINT ( 'NONE',  ( -23.05949278649137923, -18.96177454351483860, 62.65406924023815805 ) ) ;
#18845 = CIRCLE ( 'NONE', #31430, 1.999999999999999778 ) ;
#18846 = EDGE_LOOP ( 'NONE', ( #13308, #30664, #37018, #6288, #5718 ) ) ;
#18847 = FACE_OUTER_BOUND ( 'NONE', #13938, .T. ) ;
#18848 = CARTESIAN_POINT ( 'NONE',  ( -24.83590064562855559, -14.05458946445556201, 73.30084269368599337 ) ) ;
#18849 = CARTESIAN_POINT ( 'NONE',  ( -11.82099675438171005, -9.899106633794131582, 64.21409753874590365 ) ) ;
#18850 = CARTESIAN_POINT ( 'NONE',  ( -17.06879511326789256, -7.767867012253359071, 73.97490359703523666 ) ) ;
#18851 = VERTEX_POINT ( 'NONE', #10045 ) ;
#18852 = PLANE ( 'NONE',  #41460 ) ;
#18853 = AXIS2_PLACEMENT_3D ( 'NONE', #45187, #18558, #4296 ) ;
#18854 = CARTESIAN_POINT ( 'NONE',  ( -22.77158737830997026, -19.99662634883771517, 72.78367152623742697 ) ) ;
#18855 = DIRECTION ( 'NONE',  ( -0.9132646967824439299, 0.4073666574609056124, -8.344532079829881716E-09 ) ) ;
#18856 = CARTESIAN_POINT ( 'NONE',  ( -11.98246295270348405, -15.60836430055780433, 54.07175714974878389 ) ) ;
#18857 = ORIENTED_EDGE ( 'NONE', *, *, #7357, .F. ) ;
#18858 = CARTESIAN_POINT ( 'NONE',  ( -19.51667102011501953, -21.95933653056138013, 62.18841959269452246 ) ) ;
#18859 = CARTESIAN_POINT ( 'NONE',  ( -20.38066051823377478, -10.47086428435309280, 50.77966884056655772 ) ) ;
#18860 = CARTESIAN_POINT ( 'NONE',  ( -18.66311988809301425, -7.868636481342422329, 70.65595886192740238 ) ) ;
#18861 = FACE_BOUND ( 'NONE', #13302, .T. ) ;
#18862 = ORIENTED_EDGE ( 'NONE', *, *, #36604, .F. ) ;
#18863 = CARTESIAN_POINT ( 'NONE',  ( -13.14696836414372250, -20.90910850243368913, 58.24661284486880675 ) ) ;
#18864 = CARTESIAN_POINT ( 'NONE',  ( -10.53619963070230625, -16.06595416482938887, 71.63677569188099881 ) ) ;
#18865 = DIRECTION ( 'NONE',  ( -3.071710424422018668E-17, 6.404604876783312462E-16, 1.000000000000000000 ) ) ;
#18866 = B_SPLINE_CURVE_WITH_KNOTS ( 'NONE', 3,
 ( #32863, #40277, #47658, #33580, #48627, #18081, #36547, #14861, #2604, #33335 ),
 .UNSPECIFIED., .F., .F.,
 ( 4, 2, 2, 2, 4 ),
 ( 0.000000000000000000, 0.2500000000000000000, 0.5000000000000000000, 0.7500000000000000000, 1.000000000000000000 ),
 .UNSPECIFIED. ) ;
#18867 = CARTESIAN_POINT ( 'NONE',  ( -10.42302287260171312, -13.97751933429587012, 57.73352905910142852 ) ) ;
#18868 = ORIENTED_EDGE ( 'NONE', *, *, #7438, .T. ) ;
#18869 = CARTESIAN_POINT ( 'NONE',  ( -14.27401838705792159, -8.498068067913044032, 74.29134615490499982 ) ) ;
#18870 = ORIENTED_EDGE ( 'NONE', *, *, #8199, .T. ) ;
#18871 = DIRECTION ( 'NONE',  ( 3.071710424422018668E-17, -6.404604876783312462E-16, -1.000000000000000000 ) ) ;
#18872 = CARTESIAN_POINT ( 'NONE',  ( -17.13503149044196405, -7.764836982087095052, 70.77563787455143540 ) ) ;
#18873 = CARTESIAN_POINT ( 'NONE',  ( -14.41828383943595959, -8.428772226827717873, 63.67490250008367525 ) ) ;
#18874 = ORIENTED_EDGE ( 'NONE', *, *, #6754, .F. ) ;
#18875 = CARTESIAN_POINT ( 'NONE',  ( -10.59985822842712189, -17.79832335570924684, 71.70684799831278156 ) ) ;
#18876 = CARTESIAN_POINT ( 'NONE',  ( -18.31455597897553389, -22.20596705496988221, 68.97661230289300249 ) ) ;
#18877 = VERTEX_POINT ( 'NONE', #41791 ) ;
#18878 = EDGE_CURVE ( 'NONE', #16655, #3147, #33136, .T. ) ;
#18879 = ORIENTED_EDGE ( 'NONE', *, *, #46416, .F. ) ;
#18880 = ORIENTED_EDGE ( 'NONE', *, *, #7236, .F. ) ;
#18881 = CARTESIAN_POINT ( 'NONE',  ( -45.92409385541306932, -16.70920654474410938, 70.13000000000000966 ) ) ;
#18883 = CARTESIAN_POINT ( 'NONE',  ( -20.50928888383101167, -8.027964920953767347, 66.82458168832727097 ) ) ;
#18882 = CIRCLE ( 'NONE', #47212, 3.951441697420869481 ) ;
#18884 = CARTESIAN_POINT ( 'NONE',  ( -24.72409385541305582, -14.80920654474412679, 59.91176470588234793 ) ) ;
#18885 = CARTESIAN_POINT ( 'NONE',  ( -20.49170831689750827, -8.461258797198503601, 63.59649424907591708 ) ) ;
#18886 = CARTESIAN_POINT ( 'NONE',  ( -18.92409385541303024, -9.359200813967568422, 50.49621490985794026 ) ) ;
#18887 = CARTESIAN_POINT ( 'NONE',  ( -11.77169715766437008, -10.59578624409953207, 74.58885051661056309 ) ) ;
#18888 = CARTESIAN_POINT ( 'NONE',  ( -19.04042241193164386, -7.536568769452434147, 67.01576393362593365 ) ) ;
#18889 = VECTOR ( 'NONE', #41599, 1000.000000000000000 ) ;
#18890 = VERTEX_POINT ( 'NONE', #30228 ) ;
#18891 = VERTEX_POINT ( 'NONE', #11495 ) ;
#18892 = ADVANCED_FACE ( 'NONE', ( #193 ), #45742, .T. ) ;
#18893 = EDGE_CURVE ( 'NONE', #26956, #47302, #3620, .T. ) ;
#18894 = CARTESIAN_POINT ( 'NONE',  ( -9.974456273375457371, -14.72748566909688073, 71.51278126739182994 ) ) ;
#18895 = EDGE_CURVE ( 'NONE', #31648, #7640, #19428, .T. ) ;
#18896 = CARTESIAN_POINT ( 'NONE',  ( -13.91686280105865947, -8.236299372188803147, 74.31459218752463869 ) ) ;
#18897 = DIRECTION ( 'NONE',  ( 0.5263399769092094171, -0.8502742079512979334, -7.678741023867494836E-08 ) ) ;
#18898 = VECTOR ( 'NONE', #30502, 1000.000000000000000 ) ;
#18899 = CARTESIAN_POINT ( 'NONE',  ( -17.42409385541305511, -14.80920654474410725, 81.99999999999998579 ) ) ;
#18900 = EDGE_CURVE ( 'NONE', #39233, #24954, #32250, .T. ) ;
#18901 = ORIENTED_EDGE ( 'NONE', *, *, #24615, .F. ) ;
#18902 = CARTESIAN_POINT ( 'NONE',  ( -16.73034385650551670, -9.794322478646142471, 51.19202720610083901 ) ) ;
#18903 = VERTEX_POINT ( 'NONE', #26770 ) ;
#18904 = FACE_OUTER_BOUND ( 'NONE', #29254, .T. ) ;
#18905 = EDGE_CURVE ( 'NONE', #45281, #19709, #7338, .T. ) ;
#18906 = CARTESIAN_POINT ( 'NONE',  ( -12.37139604325248499, -19.73008851950320519, 57.81193715039307079 ) ) ;
#18907 = LINE ( 'NONE', #4146, #25254 ) ;
#18908 = ORIENTED_EDGE ( 'NONE', *, *, #3759, .T. ) ;
#18909 = CARTESIAN_POINT ( 'NONE',  ( -20.39546626481018876, -7.977226069863096569, 70.39066949591953914 ) ) ;
#18910 = LINE ( 'NONE', #33175, #31965 ) ;
#18911 = AXIS2_PLACEMENT_3D ( 'NONE', #10620, #17335, #9492 ) ;
#18912 = EDGE_LOOP ( 'NONE', ( #30070, #38773 ) ) ;
#18913 = CARTESIAN_POINT ( 'NONE',  ( -18.66311988809301425, -7.868636481342422329, 70.65595886192740238 ) ) ;
#18914 = DIRECTION ( 'NONE',  ( 6.517531090241554163E-16, 1.000000000000000000, 1.799495156056576137E-30 ) ) ;
#18915 = DIRECTION ( 'NONE',  ( 0.000000000000000000, -1.000000000000000000, 0.000000000000000000 ) ) ;
#18916 = EDGE_LOOP ( 'NONE', ( #26678, #20568, #27249, #27730 ) ) ;
#18917 = DIRECTION ( 'NONE',  ( -0.2466764125338440639, -0.9690979039805150963, 7.162324212089591066E-08 ) ) ;
#18918 = VECTOR ( 'NONE', #35416, 1000.000000000000000 ) ;
#18919 = ORIENTED_EDGE ( 'NONE', *, *, #47646, .F. ) ;
#18920 = CARTESIAN_POINT ( 'NONE',  ( -18.19389434033494268, -22.21941471489327569, 65.53027570717884487 ) ) ;
#18921 = CARTESIAN_POINT ( 'NONE',  ( -45.55409385541306477, -14.20920654474410760, 71.05212771298751306 ) ) ;
#18922 = ORIENTED_EDGE ( 'NONE', *, *, #34313, .F. ) ;
#18923 = CARTESIAN_POINT ( 'NONE',  ( -24.47368665962210343, -14.70950332193510590, 62.72768537250228604 ) ) ;
#18924 = DIRECTION ( 'NONE',  ( -0.9372362738803845517, -0.3486949482324240290, 5.386914174889910583E-09 ) ) ;
#18925 = ORIENTED_EDGE ( 'NONE', *, *, #17498, .T. ) ;
#18926 = CARTESIAN_POINT ( 'NONE',  ( -22.06946820259537390, -8.984793454286846170, 63.38427902854760987 ) ) ;
#18927 = B_SPLINE_CURVE_WITH_KNOTS ( 'NONE', 3,
 ( #26028, #48667, #37322, #18876, #33626, #37826, #3611, #41280, #37568, #22088 ),
 .UNSPECIFIED., .F., .F.,
 ( 4, 2, 2, 2, 4 ),
 ( 0.1272669073657949346, 0.2522669073462943112, 0.3772669073267936324, 0.5022669073072929535, 0.6272669072877923302 ),
 .UNSPECIFIED. ) ;
#18928 =( BOUNDED_CURVE ( )  B_SPLINE_CURVE ( 3, ( #26394, #34502, #31066, #12345 ),
 .UNSPECIFIED., .F., .F. ) 
 B_SPLINE_CURVE_WITH_KNOTS ( ( 4, 4 ),
 ( 0.4074455897393636228, 0.5000000000000000000 ),
 .UNSPECIFIED. ) 
 CURVE ( )  GEOMETRIC_REPRESENTATION_ITEM ( )  RATIONAL_B_SPLINE_CURVE ( ( 0.6983129098260818513, 0.7760317562606880992, 0.8765941196519940748, 0.9999999999999992228 ) ) 
 REPRESENTATION_ITEM ( '' )  );
#18929 = EDGE_CURVE ( 'NONE', #45391, #43613, #16454, .T. ) ;
#18930 = CARTESIAN_POINT ( 'NONE',  ( -16.40208609235968140, -7.882922330141489020, 60.27198835172391966 ) ) ;
#18931 = LINE ( 'NONE', #33939, #11755 ) ;
#18932 = EDGE_LOOP ( 'NONE', ( #31693, #43716 ) ) ;
#18933 = EDGE_CURVE ( 'NONE', #14728, #30719, #12955, .T. ) ;
#18934 = EDGE_LOOP ( 'NONE', ( #3413, #45696 ) ) ;
#18935 = ORIENTED_EDGE ( 'NONE', *, *, #5816, .T. ) ;
#18936 = DIRECTION ( 'NONE',  ( -1.000000000000000000, 0.000000000000000000, 8.260587980841940012E-17 ) ) ;
#18937 = LINE ( 'NONE', #27298, #38272 ) ;
#18938 = CARTESIAN_POINT ( 'NONE',  ( -23.08487763607990928, -19.01185175973044039, 62.36879011380454330 ) ) ;
#18939 = ORIENTED_EDGE ( 'NONE', *, *, #39494, .T. ) ;
#18940 = CARTESIAN_POINT ( 'NONE',  ( -15.63659385759799036, -8.995762431863214559, 51.38120296130585274 ) ) ;
#18941 = CARTESIAN_POINT ( 'NONE',  ( -20.50074447585702941, -8.457105438040551704, 70.39533052524389234 ) ) ;
#18942 = DIRECTION ( 'NONE',  ( 2.181982678098338148E-16, 0.000000000000000000, -1.000000000000000000 ) ) ;
#18943 = FACE_OUTER_BOUND ( 'NONE', #15402, .T. ) ;
#18944 =( BOUNDED_CURVE ( )  B_SPLINE_CURVE ( 3, ( #12588, #28086, #27611, #23928 ),
 .UNSPECIFIED., .F., .F. ) 
 B_SPLINE_CURVE_WITH_KNOTS ( ( 4, 4 ),
 ( 0.4074455897393611248, 0.5000000000000000000 ),
 .UNSPECIFIED. ) 
 CURVE ( )  GEOMETRIC_REPRESENTATION_ITEM ( )  RATIONAL_B_SPLINE_CURVE ( ( 0.6983129098260809631, 0.7760317562606844355, 0.8765941196519896339, 0.9999999999999945599 ) ) 
 REPRESENTATION_ITEM ( '' )  );
#18945 = DIRECTION ( 'NONE',  ( 2.342027643795563533E-48, 1.912410701131276611E-32, 1.000000000000000000 ) ) ;
#18946 = EDGE_LOOP ( 'NONE', ( #31232, #27391, #33410, #36646, #39457 ) ) ;
#18948 = CARTESIAN_POINT ( 'NONE',  ( -13.07136655094769750, -8.762923122256669473, 64.02451139116674028 ) ) ;
#18947 = VECTOR ( 'NONE', #18393, 1000.000000000000000 ) ;
#18949 = EDGE_CURVE ( 'NONE', #29256, #13129, #8299, .T. ) ;
#18950 = VECTOR ( 'NONE', #23120, 1000.000000000000000 ) ;
#18951 = CARTESIAN_POINT ( 'NONE',  ( -10.56492563526530759, -13.18000101695786341, 71.20828586226983248 ) ) ;
#18952 = FACE_OUTER_BOUND ( 'NONE', #30796, .T. ) ;
#18953 = EDGE_CURVE ( 'NONE', #27537, #24743, #46477, .T. ) ;
#18954 = VECTOR ( 'NONE', #12630, 1000.000000000000000 ) ;
#18955 = ORIENTED_EDGE ( 'NONE', *, *, #227, .F. ) ;
#18956 =( BOUNDED_CURVE ( )  B_SPLINE_CURVE ( 3, ( #39023, #41764, #5303, #46180 ),
 .UNSPECIFIED., .F., .F. ) 
 B_SPLINE_CURVE_WITH_KNOTS ( ( 4, 4 ),
 ( 0.4074455897393652881, 0.5000000000000000000 ),
 .UNSPECIFIED. ) 
 CURVE ( )  GEOMETRIC_REPRESENTATION_ITEM ( )  RATIONAL_B_SPLINE_CURVE ( ( 0.6983129098261153800, 0.7760317562607275121, 0.8765941196520252721, 1.000000000000015765 ) ) 
 REPRESENTATION_ITEM ( '' )  );
#18957 = EDGE_CURVE ( 'NONE', #33529, #18814, #7903, .T. ) ;
#18958 = ORIENTED_EDGE ( 'NONE', *, *, #45705, .T. ) ;
#18959 = FACE_OUTER_BOUND ( 'NONE', #20012, .T. ) ;
#18960 = CARTESIAN_POINT ( 'NONE',  ( -44.72480688026392670, -12.91120565595568692, 70.13000000000000966 ) ) ;
#18961 = CARTESIAN_POINT ( 'NONE',  ( -13.87255710869803593, -21.35819254899724484, 72.12596476508147703 ) ) ;
#18962 = CIRCLE ( 'NONE', #26034, 1.999999999999999778 ) ;
#18963 = EDGE_CURVE ( 'NONE', #1317, #20165, #12627, .T. ) ;
#18964 = ORIENTED_EDGE ( 'NONE', *, *, #96, .F. ) ;
#18965 = CARTESIAN_POINT ( 'NONE',  ( -11.29219319990544079, -18.28864530752396433, 57.82186711835544912 ) ) ;
#18966 = CARTESIAN_POINT ( 'NONE',  ( -13.33011785382929304, -9.069340661520646663, 63.92418669539090814 ) ) ;
#18967 = VECTOR ( 'NONE', #27218, 1000.000000000000000 ) ;
#18968 = ORIENTED_EDGE ( 'NONE', *, *, #22427, .F. ) ;
#18969 = CARTESIAN_POINT ( 'NONE',  ( -21.89130958583942288, -9.354787850460871468, 63.20625856529903075 ) ) ;
#18970 = CARTESIAN_POINT ( 'NONE',  ( -17.78823904182716120, -7.818684512505932993, 60.38060768393231825 ) ) ;
#18971 = CARTESIAN_POINT ( 'NONE',  ( -14.03512939856252295, -8.627013252941546639, 74.49394897105099744 ) ) ;
#18972 = ORIENTED_EDGE ( 'NONE', *, *, #42402, .F. ) ;
#18973 = LINE ( 'NONE', #8150, #42472 ) ;
#18974 = VERTEX_POINT ( 'NONE', #7574 ) ;
#18975 = CARTESIAN_POINT ( 'NONE',  ( -19.36683724782897897, -21.58655468785150688, 62.00975759738177118 ) ) ;
#18977 = LINE ( 'NONE', #37925, #25030 ) ;
#18976 = CIRCLE ( 'NONE', #26865, 1.250000000000001110 ) ;
#18978 = ORIENTED_EDGE ( 'NONE', *, *, #25778, .T. ) ;
#18979 = CARTESIAN_POINT ( 'NONE',  ( -13.41559392277415341, -8.529421005230245711, 57.08472474434080368 ) ) ;
#18980 = FACE_OUTER_BOUND ( 'NONE', #28470, .T. ) ;
#18981 = CARTESIAN_POINT ( 'NONE',  ( -19.96784385650551386, -6.428312510596451368, 51.20221977374900035 ) ) ;
#18982 = AXIS2_PLACEMENT_3D ( 'NONE', #6279, #13876, #9504 ) ;
#18983 = DIRECTION ( 'NONE',  ( -3.071710424422018668E-17, 6.404604876783312462E-16, 1.000000000000000000 ) ) ;
#18984 = EDGE_CURVE ( 'NONE', #44873, #11500, #79, .T. ) ;
#18985 = PLANE ( 'NONE',  #34523 ) ;
#18986 = CARTESIAN_POINT ( 'NONE',  ( -10.52155775835627161, -17.61265482900956414, 68.27534675147255427 ) ) ;
#18987 = CARTESIAN_POINT ( 'NONE',  ( -17.20779274827556904, -21.85960060673416194, 72.16543130510109449 ) ) ;
#18988 = EDGE_LOOP ( 'NONE', ( #29311, #1054, #9068, #33741 ) ) ;
#18989 = AXIS2_PLACEMENT_3D ( 'NONE', #27208, #30918, #20566 ) ;
#18990 = CARTESIAN_POINT ( 'NONE',  ( -22.29909385541301958, -8.105421454601382081, 49.25000573077637256 ) ) ;
#18991 = CARTESIAN_POINT ( 'NONE',  ( -20.56282673992903653, -8.552218612421922828, 63.31121530278369391 ) ) ;
#18992 = CARTESIAN_POINT ( 'NONE',  ( -22.38923928277987940, -20.36363336896080867, 62.35626408838342627 ) ) ;
#18993 = CARTESIAN_POINT ( 'NONE',  ( -18.44104399304328012, -21.73500248025376536, 68.88802706434297818 ) ) ;
#18994 = CARTESIAN_POINT ( 'NONE',  ( -23.76579110128109207, -18.71917648078158791, 72.92514783281183099 ) ) ;
#18995 = VERTEX_POINT ( 'NONE', #39042 ) ;
#18996 = ORIENTED_EDGE ( 'NONE', *, *, #10961, .F. ) ;
#18997 = CARTESIAN_POINT ( 'NONE',  ( -23.99312320239454976, -11.29471777418100231, 66.60709819448160829 ) ) ;
#18998 = CARTESIAN_POINT ( 'NONE',  ( -10.35393594074381163, -12.46056753982151122, 60.99191868369305780 ) ) ;
#18999 = VERTEX_POINT ( 'NONE', #28215 ) ;
#19000 = CARTESIAN_POINT ( 'NONE',  ( -10.00761937521931522, -15.51608998476985946, 57.75288115419267854 ) ) ;
#19001 = AXIS2_PLACEMENT_3D ( 'NONE', #44707, #3565, #14131 ) ;
#19002 = CARTESIAN_POINT ( 'NONE',  ( -33.42409385541304800, -8.109206544743658540, 50.50000000000030553 ) ) ;
#19003 = CARTESIAN_POINT ( 'NONE',  ( -10.45256745270239307, -15.43993597667916795, 57.86792809192976961 ) ) ;
#19004 = CARTESIAN_POINT ( 'NONE',  ( -21.57861252614732095, -20.99326887020048460, 72.62422790022243646 ) ) ;
#19005 = CARTESIAN_POINT ( 'NONE',  ( -11.41497376296057098, -19.21309731666858411, 71.80190493362104576 ) ) ;
#19006 = CARTESIAN_POINT ( 'NONE',  ( -20.54979551517892489, -8.489990701729437816, 63.31121512946744190 ) ) ;
#19007 = CARTESIAN_POINT ( 'NONE',  ( -50.42409385541305511, -14.80920654474410547, 56.99999999999998579 ) ) ;
#19008 = CARTESIAN_POINT ( 'NONE',  ( -10.03117811545256366, -15.73068522104555100, 61.15976275176203103 ) ) ;
#19009 = AXIS2_PLACEMENT_3D ( 'NONE', #47340, #2511, #16786 ) ;
#19010 = PLANE ( 'NONE',  #10131 ) ;
#19011 = DIRECTION ( 'NONE',  ( -0.9687793358424822143, 0.2479245821708672415, 0.000000000000000000 ) ) ;
#19012 = ADVANCED_FACE ( 'NONE', ( #1867 ), #27726, .T. ) ;
#19013 = CARTESIAN_POINT ( 'NONE',  ( -12.11584165285342074, -20.03677265438916422, 61.53532148967806137 ) ) ;
#19014 = CARTESIAN_POINT ( 'NONE',  ( -13.76849323099554567, -20.83774554052356009, 65.27156739751333703 ) ) ;
#19015 = CARTESIAN_POINT ( 'NONE',  ( -21.51159385541298263, -8.990409506049271471, 49.61344411288067846 ) ) ;
#19016 = CARTESIAN_POINT ( 'NONE',  ( -23.49605051889219709, -11.22618518380361330, 73.37665428612797314 ) ) ;
#19017 = ORIENTED_EDGE ( 'NONE', *, *, #10152, .T. ) ;
#19018 = VERTEX_POINT ( 'NONE', #5326 ) ;
#19019 = CARTESIAN_POINT ( 'NONE',  ( -15.38034385541304161, -9.360768649639302552, 51.01397948905922419 ) ) ;
#19020 = EDGE_CURVE ( 'NONE', #12407, #31776, #45625, .T. ) ;
#19021 = VERTEX_POINT ( 'NONE', #12936 ) ;
#19022 = CARTESIAN_POINT ( 'NONE',  ( -17.36015840614627592, -7.359395087992972151, 67.20535029649403214 ) ) ;
#19023 = AXIS2_PLACEMENT_3D ( 'NONE', #39595, #46984, #9090 ) ;
#19024 = ADVANCED_FACE ( 'NONE', ( #16137 ), #5580, .T. ) ;
#19025 = CARTESIAN_POINT ( 'NONE',  ( -13.67313190561211478, -20.71991002637085089, 65.00245577047650158 ) ) ;
#19026 = CARTESIAN_POINT ( 'NONE',  ( -17.77594409791816688, -7.367433943401969998, 60.26556080592736464 ) ) ;
#19027 = ORIENTED_EDGE ( 'NONE', *, *, #29043, .T. ) ;
#19028 = CARTESIAN_POINT ( 'NONE',  ( -24.36490017465187208, -15.72991749304959441, 73.19230876869042390 ) ) ;
#19029 = DIRECTION ( 'NONE',  ( 1.927470528863119542E-16, 0.000000000000000000, -1.000000000000000000 ) ) ;
#19030 = VERTEX_POINT ( 'NONE', #9514 ) ;
#19031 = CARTESIAN_POINT ( 'NONE',  ( -22.34946685659131305, -20.39877785696383228, 62.43450362657586084 ) ) ;
#19032 = EDGE_CURVE ( 'NONE', #19706, #32553, #35354, .T. ) ;
#19033 = CARTESIAN_POINT ( 'NONE',  ( -23.74619265052512418, -11.68934008440960426, 62.95218278636776432 ) ) ;
#19034 = EDGE_CURVE ( 'NONE', #5705, #43753, #2565, .T. ) ;
#19035 = VERTEX_POINT ( 'NONE', #19614 ) ;
#19036 = CARTESIAN_POINT ( 'NONE',  ( -11.14880203912577983, -10.79352180864503552, 57.34869885996136674 ) ) ;
#19037 = CARTESIAN_POINT ( 'NONE',  ( -20.31649657898477912, -7.943510300654241796, 70.43595776394847974 ) ) ;
#19038 = CARTESIAN_POINT ( 'NONE',  ( -18.59601872632196518, -7.856991649524070809, 73.85536540707786912 ) ) ;
#19039 = EDGE_CURVE ( 'NONE', #12740, #11221, #36410, .T. ) ;
#19040 = ORIENTED_EDGE ( 'NONE', *, *, #45360, .F. ) ;
#19041 = CARTESIAN_POINT ( 'NONE',  ( -23.21820299084679817, -10.12609468326883722, 63.17847675013702258 ) ) ;
#19042 = DIRECTION ( 'NONE',  ( 2.575747226434838513E-06, -1.267954838932485449E-05, -0.9999999999162972886 ) ) ;
#19043 = CARTESIAN_POINT ( 'NONE',  ( -19.97164353606484255, -21.81018995992316079, 69.11977899231902711 ) ) ;
#19044 = CARTESIAN_POINT ( 'NONE',  ( -23.99887651489391871, -12.24265264118830387, 73.39792675737896843 ) ) ;
#19045 = ORIENTED_EDGE ( 'NONE', *, *, #12866, .T. ) ;
#19046 = CARTESIAN_POINT ( 'NONE',  ( -24.72409385541305582, -14.80920654474412679, 59.91176470588234793 ) ) ;
#19047 = DIRECTION ( 'NONE',  ( 0.7506333037770493988, -0.6607190350373991494, 0.000000000000000000 ) ) ;
#19048 = CARTESIAN_POINT ( 'NONE',  ( -14.47983227664519212, -7.965588925009814858, 63.90483403727078837 ) ) ;
#19049 = FACE_OUTER_BOUND ( 'NONE', #3027, .T. ) ;
#19050 = CYLINDRICAL_SURFACE ( 'NONE', #21931, 0.1500000000000034084 ) ;
#19051 = CARTESIAN_POINT ( 'NONE',  ( -21.20819684703883468, -20.76197102398859329, 65.58453721533290093 ) ) ;
#19052 = CARTESIAN_POINT ( 'NONE',  ( -20.33034385650552167, -9.794322478646142471, 51.19202720610083190 ) ) ;
#19053 = VERTEX_POINT ( 'NONE', #46925 ) ;
#19054 = CARTESIAN_POINT ( 'NONE',  ( -24.28579947082789303, -13.18942387424446494, 62.84736316175410309 ) ) ;
#19055 = CARTESIAN_POINT ( 'NONE',  ( -24.71334354870178274, -13.26952572216105075, 59.47772645308575790 ) ) ;
#19056 = EDGE_LOOP ( 'NONE', ( #2369, #21355, #45458, #44933, #48690 ) ) ;
#19057 = CARTESIAN_POINT ( 'NONE',  ( -24.43774544639958179, -15.55896182022801177, 69.74127236015951325 ) ) ;
#19058 = CARTESIAN_POINT ( 'NONE',  ( -24.47509194515568964, -14.61357797254947677, 59.24300266175899310 ) ) ;
#19059 = CARTESIAN_POINT ( 'NONE',  ( -10.67632725396948956, -12.73975884439864359, 57.48424594490033002 ) ) ;
#19060 = ORIENTED_EDGE ( 'NONE', *, *, #22365, .F. ) ;
#19061 = CARTESIAN_POINT ( 'NONE',  ( -16.18447094455866164, -9.965309865531997602, 53.27966884056655061 ) ) ;
#19062 = FACE_OUTER_BOUND ( 'NONE', #11816, .T. ) ;
#19063 = CARTESIAN_POINT ( 'NONE',  ( -27.42409385541305511, -10.60920654474410618, 81.49999999999998579 ) ) ;
#19064 = ORIENTED_EDGE ( 'NONE', *, *, #19964, .F. ) ;
#19065 = CARTESIAN_POINT ( 'NONE',  ( -15.21159385650551776, -6.922745924619793101, 51.69366785382590024 ) ) ;
#19066 = CARTESIAN_POINT ( 'NONE',  ( -24.17966087195022595, -11.66819065304315117, 59.52589827039258097 ) ) ;
#19067 = LINE ( 'NONE', #29663, #21387 ) ;
#19068 = CARTESIAN_POINT ( 'NONE',  ( -15.36003256934816719, -8.059790721335600594, 70.76556701434653007 ) ) ;
#19069 = CARTESIAN_POINT ( 'NONE',  ( -44.62409385541305795, -12.70920654474410760, 70.13000000000000966 ) ) ;
#19070 = ORIENTED_EDGE ( 'NONE', *, *, #12961, .F. ) ;
#19071 = ORIENTED_EDGE ( 'NONE', *, *, #31718, .F. ) ;
#19072 = CARTESIAN_POINT ( 'NONE',  ( -14.68034385650551599, -6.424090610841176385, 49.80797279389977916 ) ) ;
#19073 = EDGE_CURVE ( 'NONE', #23878, #15180, #26729, .T. ) ;
#19074 = EDGE_CURVE ( 'NONE', #24536, #12328, #28837, .T. ) ;
#19075 = DIRECTION ( 'NONE',  ( -3.071710424422018668E-17, 6.404604876783312462E-16, 1.000000000000000000 ) ) ;
#19076 = CARTESIAN_POINT ( 'NONE',  ( -11.97490362423377164, -10.33561459433851404, 67.78424783647008667 ) ) ;
#19077 =( BOUNDED_SURFACE ( )  B_SPLINE_SURFACE ( 3, 1, ( 
 ( #7808, #175 ),
 ( #11477, #33616 ),
 ( #15153, #40782 ),
 ( #7067, #41773 ),
 ( #10744, #4341 ),
 ( #30453, #26019 ),
 ( #11727, #37311 ) ),
 .UNSPECIFIED., .T., .F., .F. ) 
 B_SPLINE_SURFACE_WITH_KNOTS ( ( 4, 3, 4 ),
 ( 2, 2 ),
 ( 0.000000000000000000, 0.5000000000000000000, 1.000000000000000000 ),
 ( 0.000000000000000000, 1.000000000000000000 ),
 .UNSPECIFIED. ) 
 GEOMETRIC_REPRESENTATION_ITEM ( )  RATIONAL_B_SPLINE_SURFACE ( (
 ( 1.000000000000000000, 1.000000000000000000),
 ( 0.3333333333333335369, 0.3333333333333330373),
 ( 0.3333333333333335369, 0.3333333333333330373),
 ( 1.000000000000000000, 1.000000000000000000),
 ( 0.3333333333333333703, 0.3333333333333333703),
 ( 0.3333333333333333703, 0.3333333333333333703),
 ( 1.000000000000000000, 1.000000000000000000) ) ) 
 REPRESENTATION_ITEM ( '' )  SURFACE ( )  );
#19078 = CARTESIAN_POINT ( 'NONE',  ( -16.87409385650551386, -9.792211528768504536, 50.49490371617623197 ) ) ;
#19079 = DIRECTION ( 'NONE',  ( -2.866981220435666553E-17, 1.000000000000000000, 1.190614954331866791E-16 ) ) ;
#19080 = CARTESIAN_POINT ( 'NONE',  ( -20.35208330028754631, -8.450993137587310855, 66.78104082230152017 ) ) ;
#19081 = CARTESIAN_POINT ( 'NONE',  ( -18.90996479553717791, -7.968725069611966916, 66.90071784165556323 ) ) ;
#19082 = ORIENTED_EDGE ( 'NONE', *, *, #6756, .T. ) ;
#19083 = B_SPLINE_CURVE_WITH_KNOTS ( 'NONE', 3,
 ( #45104, #41144, #11351, #8388, #7425, #23412, #31043, #41885, #19225, #22430 ),
 .UNSPECIFIED., .F., .F.,
 ( 4, 2, 2, 2, 4 ),
 ( 0.1272669073658535543, 0.2522669073463322809, 0.3772669073268109519, 0.5022669073072896229, 0.6272669072877683494 ),
 .UNSPECIFIED. ) ;
#19084 = CARTESIAN_POINT ( 'NONE',  ( -27.42409385541305511, -27.10920654474410796, 63.99999999999998579 ) ) ;
#19085 =( BOUNDED_CURVE ( )  B_SPLINE_CURVE ( 3, ( #7185, #13146, #33000, #43467 ),
 .UNSPECIFIED., .F., .F. ) 
 B_SPLINE_CURVE_WITH_KNOTS ( ( 4, 4 ),
 ( 0.9074455897393627346, 1.000000000000000000 ),
 .UNSPECIFIED. ) 
 CURVE ( )  GEOMETRIC_REPRESENTATION_ITEM ( )  RATIONAL_B_SPLINE_CURVE ( ( 0.6983129098260820733, 0.7760317562606887654, 0.8765941196519947409, 1.000000000000000000 ) ) 
 REPRESENTATION_ITEM ( '' )  );
#19086 = EDGE_CURVE ( 'NONE', #21615, #26298, #5911, .T. ) ;
#19087 = VERTEX_POINT ( 'NONE', #14366 ) ;
#19088 = DIRECTION ( 'NONE',  ( 0.8565259173193582320, -0.5161040137028850561, 6.301967848571305848E-08 ) ) ;
#19089 = LINE ( 'NONE', #15370, #39930 ) ;
#19090 = ADVANCED_FACE ( 'NONE', ( #18075 ), #33085, .T. ) ;
#19092 = ADVANCED_FACE ( 'NONE', ( #36538 ), #40271, .T. ) ;
#19091 = CYLINDRICAL_SURFACE ( 'NONE', #10299, 0.1500000000000020206 ) ;
#19093 = PLANE ( 'NONE',  #26213 ) ;
#19094 = EDGE_CURVE ( 'NONE', #11362, #24536, #1818, .T. ) ;
#19095 = EDGE_LOOP ( 'NONE', ( #25354, #9693, #3097, #1675, #27144, #643, #38186, #18448, #27078, #34299, #21985, #17642, #4790, #28464, #36441, #33655, #21872, #4881, #46053, #38297, #45814, #15685, #7400, #8270, #23208, #8317, #903, #15752, #36097, #13563, #26031, #13025, #21602, #17550 ) ) ;
#19096 = FACE_OUTER_BOUND ( 'NONE', #31768, .T. ) ;
#19097 = CARTESIAN_POINT ( 'NONE',  ( -24.08517543038346531, -12.49907855475201579, 73.52753481283211556 ) ) ;
#19098 = CARTESIAN_POINT ( 'NONE',  ( -33.95962776134579286, -8.109206544744111511, 51.75000000000000711 ) ) ;
#19099 = FACE_OUTER_BOUND ( 'NONE', #30055, .T. ) ;
#19100 = ORIENTED_EDGE ( 'NONE', *, *, #34694, .T. ) ;
#19101 = CARTESIAN_POINT ( 'NONE',  ( -19.57699614054808634, -21.94144247634149281, 62.17999043330664222 ) ) ;
#19102 = CARTESIAN_POINT ( 'NONE',  ( -14.64884435835704757, -8.328266481489457362, 63.79538598111422942 ) ) ;
#19103 = DIRECTION ( 'NONE',  ( 0.9687793358424821033, -0.2479245821708677133, 0.000000000000000000 ) ) ;
#19104 = FACE_BOUND ( 'NONE', #38118, .T. ) ;
#19105 = SHAPE_DEFINITION_REPRESENTATION ( #29509, #34550 ) ;
#19106 = VERTEX_POINT ( 'NONE', #6773 ) ;
#19107 = B_SPLINE_CURVE_WITH_KNOTS ( 'NONE', 3,
 ( #35654, #20421, #39112, #46991, #1933, #28033, #32226, #43316, #16457, #8857 ),
 .UNSPECIFIED., .F., .F.,
 ( 4, 2, 2, 2, 4 ),
 ( 0.000000000000000000, 0.2500000000000000000, 0.5000000000000000000, 0.7500000000000000000, 1.000000000000000000 ),
 .UNSPECIFIED. ) ;
#19108 = CARTESIAN_POINT ( 'NONE',  ( -22.11681431073945703, -20.00335822171163258, 62.24941606537704786 ) ) ;
#19109 = CARTESIAN_POINT ( 'NONE',  ( -16.06050865347321732, -9.480920197610746669, 53.49999999999995026 ) ) ;
#19110 = AXIS2_PLACEMENT_3D ( 'NONE', #9726, #24744, #21037 ) ;
#19111 = CARTESIAN_POINT ( 'NONE',  ( -23.42597896001542424, -18.52301023162717897, 65.97956265853692059 ) ) ;
#19112 = CARTESIAN_POINT ( 'NONE',  ( -14.42409385541304090, -9.359200813967568422, 50.49621490985801842 ) ) ;
#19113 = ORIENTED_EDGE ( 'NONE', *, *, #31418, .F. ) ;
#19114 = DIRECTION ( 'NONE',  ( -0.2189141945955536961, 0.9757441136919967617, 0.000000000000000000 ) ) ;
#19115 = ORIENTED_EDGE ( 'NONE', *, *, #6779, .T. ) ;
#19116 = DIRECTION ( 'NONE',  ( -0.9629498065864410261, -0.2696806815386222911, 2.751890642837218776E-17 ) ) ;
#19117 = CARTESIAN_POINT ( 'NONE',  ( -17.42409385541299471, -14.80920654474435771, 49.52966884056655772 ) ) ;
#19118 = DIRECTION ( 'NONE',  ( 1.000000000000000000, 0.000000000000000000, 0.000000000000000000 ) ) ;
#19119 = ORIENTED_EDGE ( 'NONE', *, *, #17576, .F. ) ;
#19120 = CARTESIAN_POINT ( 'NONE',  ( -24.72409385541305582, -14.90920654474425255, 71.08235294117645253 ) ) ;
#19121 = EDGE_LOOP ( 'NONE', ( #34994, #28494, #12312, #23842, #21835 ) ) ;
#19122 = EDGE_CURVE ( 'NONE', #14238, #8811, #44072, .T. ) ;
#19123 = ORIENTED_EDGE ( 'NONE', *, *, #4644, .F. ) ;
#19124 = ORIENTED_EDGE ( 'NONE', *, *, #42475, .T. ) ;
#19125 = CYLINDRICAL_SURFACE ( 'NONE', #15464, 1.250000000000001110 ) ;
#19126 = CARTESIAN_POINT ( 'NONE',  ( -22.58065782673598676, -12.89613362149922438, 54.07175714974875547 ) ) ;
#19127 = CARTESIAN_POINT ( 'NONE',  ( -23.19948571119275726, -18.85291137746750323, 65.83861571032234394 ) ) ;
#19128 = CARTESIAN_POINT ( 'NONE',  ( -10.66703338591908690, -12.79807911521252883, 64.41836111017862265 ) ) ;
#19129 = CARTESIAN_POINT ( 'NONE',  ( -4.424093855413056886, -8.109206544744111511, 50.49999999999999289 ) ) ;
#19130 = CARTESIAN_POINT ( 'NONE',  ( -14.19282086353638839, -8.542981675383003903, 71.01485553001869278 ) ) ;
#19131 = CARTESIAN_POINT ( 'NONE',  ( -11.79630000206883977, -19.05592701419838519, 71.97213747039440079 ) ) ;
#19132 = EDGE_LOOP ( 'NONE', ( #8765, #7197 ) ) ;
#19133 = ORIENTED_EDGE ( 'NONE', *, *, #24085, .F. ) ;
#19134 = CARTESIAN_POINT ( 'NONE',  ( -17.56877512014188625, -7.360533253644350182, 63.59411120999686062 ) ) ;
#19135 = ADVANCED_FACE ( 'NONE', ( #35825 ), #17359, .T. ) ;
#19136 = CARTESIAN_POINT ( 'NONE',  ( -9.985622318910028383, -14.38165043598653980, 64.50148546807987771 ) ) ;
#19137 = CYLINDRICAL_SURFACE ( 'NONE', #37005, 0.1499999999999954148 ) ;
#19138 = LINE ( 'NONE', #30725, #19726 ) ;
#19139 = VERTEX_POINT ( 'NONE', #40494 ) ;
#19140 = CARTESIAN_POINT ( 'NONE',  ( -16.95534385650551812, -7.417179338643134834, 52.18511593390279302 ) ) ;
#19141 = ORIENTED_EDGE ( 'NONE', *, *, #11053, .F. ) ;
#19142 = CARTESIAN_POINT ( 'NONE',  ( -16.12972974591750486, -21.68894147889758273, 58.30202270284849675 ) ) ;
#19143 = CARTESIAN_POINT ( 'NONE',  ( -14.38502091232239621, -11.22596901536237013, 52.02966884056656482 ) ) ;
#19144 = CIRCLE ( 'NONE', #12082, 5.249999999999998224 ) ;
#19145 = CARTESIAN_POINT ( 'NONE',  ( -10.04792990808071984, -13.75760301026566523, 57.63480408467697913 ) ) ;
#19146 = ORIENTED_EDGE ( 'NONE', *, *, #24903, .T. ) ;
#19147 = CARTESIAN_POINT ( 'NONE',  ( -23.46734565652671378, -18.44686360299153804, 69.50191697180839867 ) ) ;
#19148 = CARTESIAN_POINT ( 'NONE',  ( -24.72409385541305582, -14.80920654474421028, 67.05882352941175384 ) ) ;
#19149 = EDGE_CURVE ( 'NONE', #27520, #1919, #2823, .T. ) ;
#19150 = ADVANCED_FACE ( 'NONE', ( #5815, #32401, #14124 ), #36069, .T. ) ;
#19151 = CARTESIAN_POINT ( 'NONE',  ( -22.83623332803211881, -19.92908237830355134, 72.82117468064575405 ) ) ;
#19152 = ORIENTED_EDGE ( 'NONE', *, *, #38199, .T. ) ;
#19153 = CARTESIAN_POINT ( 'NONE',  ( -10.38649001812422057, -14.33425944237064442, 61.12641118716408783 ) ) ;
#19154 = CARTESIAN_POINT ( 'NONE',  ( -19.37616851487812752, -21.99900361761337919, 58.71002773933979313 ) ) ;
#19155 = CARTESIAN_POINT ( 'NONE',  ( -10.72552546848295485, -12.61109793159036663, 61.09853568372136579 ) ) ;
#19156 = ORIENTED_EDGE ( 'NONE', *, *, #29262, .T. ) ;
#19157 = CARTESIAN_POINT ( 'NONE',  ( -11.18894283504542564, -11.62402331817657775, 71.19933931412334971 ) ) ;
#19158 = ORIENTED_EDGE ( 'NONE', *, *, #36525, .T. ) ;
#19159 = CARTESIAN_POINT ( 'NONE',  ( -10.51737753838112610, -13.38018574993044219, 71.09339731095114701 ) ) ;
#19160 = EDGE_CURVE ( 'NONE', #27520, #12228, #24771, .T. ) ;
#19161 = EDGE_CURVE ( 'NONE', #36429, #33207, #13889, .T. ) ;
#19162 = DIRECTION ( 'NONE',  ( 1.000000000000000000, 0.000000000000000000, 0.000000000000000000 ) ) ;
#19163 = B_SPLINE_CURVE_WITH_KNOTS ( 'NONE', 1,
 ( #10581, #35940 ),
 .UNSPECIFIED., .F., .F.,
 ( 2, 2 ),
 ( 0.000000000000000000, 1.000000000000000000 ),
 .UNSPECIFIED. ) ;
#19164 = VERTEX_POINT ( 'NONE', #39775 ) ;
#19165 = CARTESIAN_POINT ( 'NONE',  ( 18.57132275349405148, 1.802465958033905302, 51.78855248148219204 ) ) ;
#19166 = CARTESIAN_POINT ( 'NONE',  ( -24.55871690389112061, -12.66422819002857558, 69.88747705124970366 ) ) ;
#19167 = ADVANCED_FACE ( 'NONE', ( #43981 ), #2107, .T. ) ;
#19168 = CARTESIAN_POINT ( 'NONE',  ( -10.39241571269986331, -17.41794234916963191, 53.49999999999994316 ) ) ;
#19169 = ORIENTED_EDGE ( 'NONE', *, *, #21755, .T. ) ;
#19170 = CARTESIAN_POINT ( 'NONE',  ( -22.08245549401321028, -8.995232178987802030, 63.39142531933751457 ) ) ;
#19171 = CARTESIAN_POINT ( 'NONE',  ( -21.62409385541304374, -9.359200813967568422, 50.49621490985803263 ) ) ;
#19172 = CARTESIAN_POINT ( 'NONE',  ( -11.97682588793020386, -9.726891629870488387, 60.65894467978176863 ) ) ;
#19173 = ORIENTED_EDGE ( 'NONE', *, *, #2591, .T. ) ;
#19174 = CARTESIAN_POINT ( 'NONE',  ( -19.13762013005870699, -8.022059148145649132, 63.43089277029390161 ) ) ;
#19175 = CARTESIAN_POINT ( 'NONE',  ( -21.67414471755420635, -8.689506427787394571, 70.24477150985708818 ) ) ;
#19176 = EDGE_CURVE ( 'NONE', #38907, #36780, #2924, .T. ) ;
#19177 = AXIS2_PLACEMENT_3D ( 'NONE', #13091, #5243, #6208 ) ;
#19178 = ORIENTED_EDGE ( 'NONE', *, *, #38282, .F. ) ;
#19179 = ORIENTED_EDGE ( 'NONE', *, *, #40106, .T. ) ;
#19180 = DIRECTION ( 'NONE',  ( -3.071710424422018668E-17, 6.404604876783312462E-16, 1.000000000000000000 ) ) ;
#19181 = CARTESIAN_POINT ( 'NONE',  ( -19.19606018965890115, -19.75113282002397597, 50.77966884056656482 ) ) ;
#19182 = CARTESIAN_POINT ( 'NONE',  ( -18.50517187854146783, -19.38160480531894692, 49.52966884056656482 ) ) ;
#19183 = ORIENTED_EDGE ( 'NONE', *, *, #11450, .T. ) ;
#19184 = CARTESIAN_POINT ( 'NONE',  ( -21.68034385650551599, -6.424090610841174609, 49.80797279389977916 ) ) ;
#19185 = CARTESIAN_POINT ( 'NONE',  ( -20.38154718419116662, -8.406214666052791884, 70.66588945595221105 ) ) ;
#19186 = B_SPLINE_CURVE_WITH_KNOTS ( 'NONE', 3,
 ( #38470, #45164, #34285, #41694, #34532, #19041, #15818, #30869, #45883, #34045 ),
 .UNSPECIFIED., .F., .F.,
 ( 4, 2, 2, 2, 4 ),
 ( 0.6272669072979214500, 0.7522669073149003127, 0.8772669073318792865, 1.002266907348858149, 1.127266907365837012 ),
 .UNSPECIFIED. ) ;
#19187 = CARTESIAN_POINT ( 'NONE',  ( -24.03160980685186843, -17.26750534774173929, 69.41339792588560442 ) ) ;
#19188 = CARTESIAN_POINT ( 'NONE',  ( -10.71289789653228830, -16.96858549093376212, 57.98760533367797620 ) ) ;
#19189 = CYLINDRICAL_SURFACE ( 'NONE', #21345, 2.000000000000001332 ) ;
#19190 = ORIENTED_EDGE ( 'NONE', *, *, #8679, .F. ) ;
#19191 = CARTESIAN_POINT ( 'NONE',  ( -16.26183941974026581, -7.855670460422400581, 60.35028478908645155 ) ) ;
#19192 = DIRECTION ( 'NONE',  ( 5.410999918679618404E-17, 0.000000000000000000, 1.000000000000000000 ) ) ;
#19193 = LINE ( 'NONE', #732, #29173 ) ;
#19194 = EDGE_LOOP ( 'NONE', ( #46568, #16570, #18530, #28759, #4777 ) ) ;
#19195 = ORIENTED_EDGE ( 'NONE', *, *, #46372, .F. ) ;
#19196 = CARTESIAN_POINT ( 'NONE',  ( -19.86902678349231621, -21.36835431182334233, 69.20703478714260370 ) ) ;
#19197 = FACE_OUTER_BOUND ( 'NONE', #33497, .T. ) ;
#19198 = CARTESIAN_POINT ( 'NONE',  ( -11.67751508479469358, -10.06770433361378991, 67.65930235469357967 ) ) ;
#19199 = CARTESIAN_POINT ( 'NONE',  ( -11.46043843694620179, -11.04924462883820802, 57.50903212149483323 ) ) ;
#19200 = EDGE_CURVE ( 'NONE', #18139, #42076, #10705, .T. ) ;
#19201 = B_SPLINE_CURVE_WITH_KNOTS ( 'NONE', 1,
 ( #33184, #10076 ),
 .UNSPECIFIED., .F., .F.,
 ( 2, 2 ),
 ( 0.000000000000000000, 1.000000000000000000 ),
 .UNSPECIFIED. ) ;
#19202 = ORIENTED_EDGE ( 'NONE', *, *, #38766, .F. ) ;
#19203 = FACE_OUTER_BOUND ( 'NONE', #2319, .T. ) ;
#19204 = AXIS2_PLACEMENT_3D ( 'NONE', #31544, #38685, #1248 ) ;
#19205 = CARTESIAN_POINT ( 'NONE',  ( -14.22586362203780652, -8.080537296073694975, 67.30329176109222544 ) ) ;
#19206 = ADVANCED_FACE ( 'NONE', ( #9984 ), #25005, .T. ) ;
#19207 = CIRCLE ( 'NONE', #24745, 5.249999999999998224 ) ;
#19208 = EDGE_LOOP ( 'NONE', ( #23404, #10577, #46346, #31721 ) ) ;
#19209 = CARTESIAN_POINT ( 'NONE',  ( -22.84776207900630851, -9.701615188675109636, 73.73807001133110361 ) ) ;
#19210 = LINE ( 'NONE', #44843, #43038 ) ;
#19211 =( BOUNDED_CURVE ( )  B_SPLINE_CURVE ( 3, ( #6382, #36157, #20917, #10326 ),
 .UNSPECIFIED., .F., .F. ) 
 B_SPLINE_CURVE_WITH_KNOTS ( ( 4, 4 ),
 ( 0.9074455897393687298, 1.000000000000000000 ),
 .UNSPECIFIED. ) 
 CURVE ( )  GEOMETRIC_REPRESENTATION_ITEM ( )  RATIONAL_B_SPLINE_CURVE ( ( 0.6983129098261068313, 0.7760317562607100816, 0.8765941196520078416, 1.000000000000000000 ) ) 
 REPRESENTATION_ITEM ( '' )  );
#19212 = CARTESIAN_POINT ( 'NONE',  ( -23.63484821195902441, -11.47287264873313184, 66.71654728383106203 ) ) ;
#19213 = B_SPLINE_CURVE_WITH_KNOTS ( 'NONE', 3,
 ( #12449, #35091, #4346, #8522, #42505, #8779, #45731, #38798, #34608, #46442 ),
 .UNSPECIFIED., .F., .F.,
 ( 4, 2, 2, 2, 4 ),
 ( 0.000000000000000000, 0.2500000000000000000, 0.5000000000000000000, 0.7500000000000000000, 1.000000000000000000 ),
 .UNSPECIFIED. ) ;
#19214 = ORIENTED_EDGE ( 'NONE', *, *, #20799, .T. ) ;
#19215 = CARTESIAN_POINT ( 'NONE',  ( -12.15299190543910512, -20.07505386821981119, 65.05330132703942070 ) ) ;
#19216 = EDGE_LOOP ( 'NONE', ( #7405, #29982, #45245, #42906, #276 ) ) ;
#19217 = EDGE_CURVE ( 'NONE', #41525, #44500, #14602, .T. ) ;
#19218 = DIRECTION ( 'NONE',  ( -2.866981220435666553E-17, 1.000000000000000000, 1.190614954331866791E-16 ) ) ;
#19219 = DIRECTION ( 'NONE',  ( -2.866981220435666553E-17, 1.000000000000000000, 1.190614954331866791E-16 ) ) ;
#19220 = VERTEX_POINT ( 'NONE', #34078 ) ;
#19221 = CARTESIAN_POINT ( 'NONE',  ( -23.23616624490289340, -18.79948399208958776, 66.12389430041484673 ) ) ;
#19222 = CARTESIAN_POINT ( 'NONE',  ( -13.35819042472069107, -21.05197888995676436, 61.70141705377209007 ) ) ;
#19223 = EDGE_CURVE ( 'NONE', #28760, #28899, #29664, .T. ) ;
#19224 = CARTESIAN_POINT ( 'NONE',  ( -22.72409385650551528, -6.426201560718813433, 50.50509628382439331 ) ) ;
#19225 = CARTESIAN_POINT ( 'NONE',  ( -21.41690965305989991, -21.09893724392033576, 69.24724315047997436 ) ) ;
#19226 = EDGE_CURVE ( 'NONE', #9317, #8500, #26437, .T. ) ;
#19227 = CARTESIAN_POINT ( 'NONE',  ( -19.04853579327176760, -7.948602568230340282, 63.71617106789811658 ) ) ;
#19228 = CARTESIAN_POINT ( 'NONE',  ( -21.68499601416157674, -9.192516039336663169, 66.66149992327366647 ) ) ;
#19229 = VERTEX_POINT ( 'NONE', #4302 ) ;
#19231 = CARTESIAN_POINT ( 'NONE',  ( -24.86242983737997747, -14.39095285025967286, 66.36788159907001727 ) ) ;
#19230 =( BOUNDED_CURVE ( )  B_SPLINE_CURVE ( 3, ( #9515, #44634, #39776, #13167 ),
 .UNSPECIFIED., .F., .F. ) 
 B_SPLINE_CURVE_WITH_KNOTS ( ( 4, 4 ),
 ( 6.081827386389250911, 6.283185307179578238 ),
 .UNSPECIFIED. ) 
 CURVE ( )  GEOMETRIC_REPRESENTATION_ITEM ( )  RATIONAL_B_SPLINE_CURVE ( ( 1.000000000000000000, 0.9966241020034157794, 0.9966241020034157794, 1.000000000000000000 ) ) 
 REPRESENTATION_ITEM ( '' )  );
#19232 = CARTESIAN_POINT ( 'NONE',  ( -17.42409385541300892, -14.80920654474439502, 75.49999999999994316 ) ) ;
#19233 = CARTESIAN_POINT ( 'NONE',  ( -22.33613286903973716, -20.41056029178123055, 62.34165005762706357 ) ) ;
#19234 = CARTESIAN_POINT ( 'NONE',  ( -24.76828060908045614, -13.20045483505886352, 53.76227901944320564 ) ) ;
#19235 = CARTESIAN_POINT ( 'NONE',  ( -22.78986551909422786, -9.640697744553680337, 73.62014601573351058 ) ) ;
#19236 = VERTEX_POINT ( 'NONE', #37515 ) ;
#19237 = EDGE_LOOP ( 'NONE', ( #2175, #36853, #42653, #29008, #11123 ) ) ;
#19238 = CARTESIAN_POINT ( 'NONE',  ( -18.73521446872676322, -7.879141670414848697, 74.25553277440172906 ) ) ;
#19239 = CARTESIAN_POINT ( 'NONE',  ( -14.47651980493331081, -8.396190447208750740, 60.47563573450432273 ) ) ;
#19240 = ORIENTED_EDGE ( 'NONE', *, *, #1970, .F. ) ;
#19241 = CARTESIAN_POINT ( 'NONE',  ( -12.79725882921341373, -20.12850138265567068, 72.10653676770067477 ) ) ;
#19242 = CARTESIAN_POINT ( 'NONE',  ( -15.34465393633500696, -21.54586957516256263, 68.86120835375241711 ) ) ;
#19243 = CARTESIAN_POINT ( 'NONE',  ( -21.20534385759799179, -7.595227055684746986, 51.75156210489594599 ) ) ;
#19244 = CARTESIAN_POINT ( 'NONE',  ( -16.26184114368905043, -7.855670183028919062, 60.20028478909661374 ) ) ;
#19245 = EDGE_CURVE ( 'NONE', #28015, #26442, #7516, .T. ) ;
#19246 = CARTESIAN_POINT ( 'NONE',  ( -24.39996007374347542, -14.20938048761671446, 73.23344610889544981 ) ) ;
#19247 = DIRECTION ( 'NONE',  ( -0.5510797171261976324, 0.8280216580999243403, 0.1033986416233888955 ) ) ;
#19248 = CARTESIAN_POINT ( 'NONE',  ( -20.60788153932096023, -8.518722016582882972, 63.32593600985608617 ) ) ;
#19249 =( BOUNDED_SURFACE ( )  B_SPLINE_SURFACE ( 3, 1, ( 
 ( #9225, #5284 ),
 ( #24249, #30670 ),
 ( #11953, #26963 ),
 ( #30912, #12183 ),
 ( #8490, #38519 ),
 ( #34822, #43202 ),
 ( #20558, #21522 ) ),
 .UNSPECIFIED., .T., .F., .F. ) 
 B_SPLINE_SURFACE_WITH_KNOTS ( ( 4, 3, 4 ),
 ( 2, 2 ),
 ( 0.000000000000000000, 0.5000000000000000000, 1.000000000000000000 ),
 ( 0.000000000000000000, 1.000000000000000000 ),
 .UNSPECIFIED. ) 
 GEOMETRIC_REPRESENTATION_ITEM ( )  RATIONAL_B_SPLINE_SURFACE ( (
 ( 1.000000000000000000, 1.000000000000000000),
 ( 0.3333333333333335369, 0.3333333333333330373),
 ( 0.3333333333333335369, 0.3333333333333330373),
 ( 1.000000000000000000, 1.000000000000000000),
 ( 0.3333333333333333703, 0.3333333333333333703),
 ( 0.3333333333333333703, 0.3333333333333333703),
 ( 1.000000000000000000, 1.000000000000000000) ) ) 
 REPRESENTATION_ITEM ( '' )  SURFACE ( )  );
#19250 = AXIS2_PLACEMENT_3D ( 'NONE', #15535, #45621, #19489 ) ;
#19251 = CARTESIAN_POINT ( 'NONE',  ( -24.72409385541305582, -14.80920654474410547, 56.99999999999998579 ) ) ;
#19252 = CIRCLE ( 'NONE', #379, 4.686499999999998778 ) ;
#19253 = CARTESIAN_POINT ( 'NONE',  ( -14.95535764022100977, -18.80681796222810576, 52.02966884056656482 ) ) ;
#19254 = CARTESIAN_POINT ( 'NONE',  ( -24.17783940236180840, -12.77441742776904299, 73.33405665229432202 ) ) ;
#19255 = DIRECTION ( 'NONE',  ( -2.866981220435666553E-17, 1.000000000000000000, 1.190614954331866791E-16 ) ) ;
#19256 = CARTESIAN_POINT ( 'NONE',  ( -11.82205746763155041, -9.897907871467767293, 64.07268414109491061 ) ) ;
#19257 = DIRECTION ( 'NONE',  ( 1.000000000000000000, -0.000000000000000000, -2.406186529621654511E-16 ) ) ;
#19258 = ORIENTED_EDGE ( 'NONE', *, *, #11798, .F. ) ;
#19259 = ORIENTED_EDGE ( 'NONE', *, *, #8291, .T. ) ;
#19260 = CARTESIAN_POINT ( 'NONE',  ( -22.80534385650551599, -8.801233750844183135, 48.81488406609782515 ) ) ;
#19261 = EDGE_LOOP ( 'NONE', ( #22150, #26122, #26183, #14190 ) ) ;
#19262 = DIRECTION ( 'NONE',  ( 0.9687793358424821033, -0.2479245821708679909, 0.000000000000000000 ) ) ;
#19263 = CARTESIAN_POINT ( 'NONE',  ( -16.43985614576752852, -21.73979035755244382, 61.75568083065761016 ) ) ;
#19264 = EDGE_CURVE ( 'NONE', #8282, #25938, #2332, .T. ) ;
#19265 = CARTESIAN_POINT ( 'NONE',  ( -13.37515154783066862, -8.555510161798645541, 57.06944116666958422 ) ) ;
#19266 = CARTESIAN_POINT ( 'NONE',  ( -16.84878425383806189, -22.23771130781744532, 72.35198525528087998 ) ) ;
#19267 = ORIENTED_EDGE ( 'NONE', *, *, #31459, .F. ) ;
#19268 = CARTESIAN_POINT ( 'NONE',  ( -20.95734383732741080, -8.250155102951309161, 59.98091898960346668 ) ) ;
#19269 = DIRECTION ( 'NONE',  ( -0.3506977235573949248, 0.2775087506578152174, 0.8944271909999157444 ) ) ;
#19270 = ORIENTED_EDGE ( 'NONE', *, *, #5122, .F. ) ;
#19271 = CARTESIAN_POINT ( 'NONE',  ( -12.26752988409003287, -16.72227946798956921, 53.49999999999995026 ) ) ;
#19272 = PLANE ( 'NONE',  #40871 ) ;
#19273 = VERTEX_POINT ( 'NONE', #45679 ) ;
#19274 = DIRECTION ( 'NONE',  ( -3.071710424422018668E-17, 6.404604876783312462E-16, 1.000000000000000000 ) ) ;
#19275 = CYLINDRICAL_SURFACE ( 'NONE', #9475, 0.1500000000000048794 ) ;
#19276 = LINE ( 'NONE', #34283, #29704 ) ;
#19277 = ORIENTED_EDGE ( 'NONE', *, *, #33297, .F. ) ;
#19278 = DIRECTION ( 'NONE',  ( 0.9997277805376392212, -0.02333162706040292633, -9.101776391673708383E-09 ) ) ;
#19279 = CIRCLE ( 'NONE', #1101, 1.250000000000001110 ) ;
#19280 = EDGE_CURVE ( 'NONE', #36826, #9358, #6303, .T. ) ;
#19281 = CARTESIAN_POINT ( 'NONE',  ( -14.98927377128279126, -8.246306944878790901, 56.84999999999994458 ) ) ;
#19282 = EDGE_CURVE ( 'NONE', #36314, #42245, #12591, .T. ) ;
#19283 = CARTESIAN_POINT ( 'NONE',  ( -11.56105952661339487, -10.21267894317357516, 71.07554790443391823 ) ) ;
#19284 = DIRECTION ( 'NONE',  ( 0.06357898915123476324, -0.9979768094191905359, 0.000000000000000000 ) ) ;
#19285 = VERTEX_POINT ( 'NONE', #22782 ) ;
#19286 = CARTESIAN_POINT ( 'NONE',  ( -47.17409385541305511, -15.80920654474410725, 70.50000000000000000 ) ) ;
#19287 = CARTESIAN_POINT ( 'NONE',  ( -20.19231657184298356, -8.325423463105360966, 70.25100341277898508 ) ) ;
#19288 = LINE ( 'NONE', #15573, #34441 ) ;
#19289 = DIRECTION ( 'NONE',  ( 0.000000000000000000, 0.000000000000000000, 1.000000000000000000 ) ) ;
#19290 = EDGE_CURVE ( 'NONE', #38378, #19901, #48726, .T. ) ;
#19291 = CARTESIAN_POINT ( 'NONE',  ( -21.94239175829699207, -20.22099772874085488, 59.06442899522711087 ) ) ;
#19292 = CARTESIAN_POINT ( 'NONE',  ( -20.55534385650551599, -7.417179338643134834, 52.18511593390279302 ) ) ;
#19293 = VERTEX_POINT ( 'NONE', #22277 ) ;
#19294 = B_SPLINE_CURVE_WITH_KNOTS ( 'NONE', 1,
 ( #45692, #19570 ),
 .UNSPECIFIED., .F., .F.,
 ( 2, 2 ),
 ( 0.000000000000000000, 1.000000000000000000 ),
 .UNSPECIFIED. ) ;
#19295 = CARTESIAN_POINT ( 'NONE',  ( -14.01352161170464861, -20.97950563691217241, 71.93167508253637266 ) ) ;
#19296 = CARTESIAN_POINT ( 'NONE',  ( -8.424093855413053333, -15.80920654474410725, 47.99999999999998579 ) ) ;
#19297 = VERTEX_POINT ( 'NONE', #37271 ) ;
#19298 = CARTESIAN_POINT ( 'NONE',  ( -15.64068491485237367, -7.988352816650894361, 70.90430021208057099 ) ) ;
#19299 = CARTESIAN_POINT ( 'NONE',  ( -50.42609385541305755, -14.90920654474410512, 56.99999999999998579 ) ) ;
#19300 = EDGE_CURVE ( 'NONE', #24671, #16341, #34626, .T. ) ;
#19301 = ORIENTED_EDGE ( 'NONE', *, *, #24021, .T. ) ;
#19302 = EDGE_CURVE ( 'NONE', #11292, #33252, #3448, .T. ) ;
#19303 = CARTESIAN_POINT ( 'NONE',  ( -18.39792479006713677, -22.19536379348757293, 68.85868763382491409 ) ) ;
#19304 = CARTESIAN_POINT ( 'NONE',  ( -16.87480544004084493, -7.378732441012598287, 74.07362965403005717 ) ) ;
#19305 = CARTESIAN_POINT ( 'NONE',  ( -14.61488608402547129, -21.70940465152681398, 58.34334805677458746 ) ) ;
#19306 = ORIENTED_EDGE ( 'NONE', *, *, #27149, .F. ) ;
#19307 = CARTESIAN_POINT ( 'NONE',  ( -16.22409385650551883, -6.426201560718813433, 50.50509628382439331 ) ) ;
#19308 = CARTESIAN_POINT ( 'NONE',  ( -12.88615340579958790, -8.900756115988826878, 67.47968544571848781 ) ) ;
#19309 = DIRECTION ( 'NONE',  ( 1.000000000000000000, 1.669677910507523057E-21, 6.493791346278465266E-22 ) ) ;
#19310 = CARTESIAN_POINT ( 'NONE',  ( -22.53429319464570924, -9.952421322533329118, 73.48161091678163359 ) ) ;
#19311 = ORIENTED_EDGE ( 'NONE', *, *, #19393, .T. ) ;
#19312 = VERTEX_POINT ( 'NONE', #29917 ) ;
#19313 = AXIS2_PLACEMENT_3D ( 'NONE', #16321, #30412, #31364 ) ;
#19314 = CARTESIAN_POINT ( 'NONE',  ( -14.62409385650551386, -6.426201560718813433, 50.50509628382439331 ) ) ;
#19315 = CARTESIAN_POINT ( 'NONE',  ( -22.95709159497877394, -9.820362260273858723, 70.21167301517006365 ) ) ;
#19316 = FACE_OUTER_BOUND ( 'NONE', #5657, .T. ) ;
#19317 = DIRECTION ( 'NONE',  ( -3.071710424422018668E-17, 6.404604876783312462E-16, 1.000000000000000000 ) ) ;
#19318 = ADVANCED_FACE ( 'NONE', ( #4071 ), #16059, .T. ) ;
#19319 = CARTESIAN_POINT ( 'NONE',  ( -16.64909385650551599, -8.104110260919579645, 48.81699501597546487 ) ) ;
#19320 = DIRECTION ( 'NONE',  ( 0.000000000000000000, 0.000000000000000000, 1.000000000000000000 ) ) ;
#19321 = CARTESIAN_POINT ( 'NONE',  ( -20.42320230239022294, -8.483743783821255491, 67.06487496235745027 ) ) ;
#19322 = CARTESIAN_POINT ( 'NONE',  ( -20.83700022493355775, -19.12221826660256951, 54.07175714974878389 ) ) ;
#19323 = DIRECTION ( 'NONE',  ( 0.000000000000000000, 0.000000000000000000, 1.000000000000000000 ) ) ;
#19324 = VERTEX_POINT ( 'NONE', #19555 ) ;
#19325 = CARTESIAN_POINT ( 'NONE',  ( -17.80887632446114921, -10.12652590253629725, 52.02966884056656482 ) ) ;
#19326 = EDGE_CURVE ( 'NONE', #40825, #13202, #13380, .T. ) ;
#19327 = ORIENTED_EDGE ( 'NONE', *, *, #3435, .T. ) ;
#19328 = DIRECTION ( 'NONE',  ( -0.7029450532227031756, -0.7112441579020041260, 7.405715380709763191E-09 ) ) ;
#19329 = CARTESIAN_POINT ( 'NONE',  ( -17.42409385541299471, -14.80920654474435594, 52.02966884056656482 ) ) ;
#19330 = CARTESIAN_POINT ( 'NONE',  ( -12.54360673743864574, -9.180396906553989211, 74.41899371332708313 ) ) ;
#19331 = PLANE ( 'NONE',  #44294 ) ;
#19332 = VERTEX_POINT ( 'NONE', #27428 ) ;
#19333 = CARTESIAN_POINT ( 'NONE',  ( -10.33481637538221243, -12.51883299443452202, 60.84207650303104487 ) ) ;
#19334 = PLANE ( 'NONE',  #3774 ) ;
#19335 = CARTESIAN_POINT ( 'NONE',  ( -10.33193864190904421, -12.52760266535700318, 60.97570470297297618 ) ) ;
#19336 = CARTESIAN_POINT ( 'NONE',  ( -24.47066272824306665, -14.57993217219608972, 62.99824437345091610 ) ) ;
#19337 = VERTEX_POINT ( 'NONE', #39240 ) ;
#19338 = CARTESIAN_POINT ( 'NONE',  ( -14.78754730678460660, -8.270772302057270764, 60.46996282000571199 ) ) ;
#19339 = CARTESIAN_POINT ( 'NONE',  ( -20.88270815654435353, -21.40782497263450068, 58.82970582236164603 ) ) ;
#19340 = CYLINDRICAL_SURFACE ( 'NONE', #26282, 5.249999999999998224 ) ;
#19341 = FACE_BOUND ( 'NONE', #15981, .T. ) ;
#19342 = SHAPE_DEFINITION_REPRESENTATION ( #4797, #34837 ) ;
#19344 = ORIENTED_EDGE ( 'NONE', *, *, #3137, .F. ) ;
#19343 = EDGE_CURVE ( 'NONE', #33991, #27147, #46289, .T. ) ;
#19345 = CARTESIAN_POINT ( 'NONE',  ( -13.60238447927381777, -8.884931327198675177, 57.11967755504965538 ) ) ;
#19346 = CARTESIAN_POINT ( 'NONE',  ( -14.31159385541286433, -8.990409506049420685, 49.61344411288053635 ) ) ;
#19347 = CARTESIAN_POINT ( 'NONE',  ( -23.58525830889974984, -18.99772868593042219, 65.86743475655129032 ) ) ;
#19348 = EDGE_CURVE ( 'NONE', #21537, #24440, #5521, .T. ) ;
#19349 = CARTESIAN_POINT ( 'NONE',  ( -14.64909385541304765, -8.112991634885936776, 51.74999426922421009 ) ) ;
#19350 = ORIENTED_EDGE ( 'NONE', *, *, #37408, .T. ) ;
#19351 = LINE ( 'NONE', #30455, #11109 ) ;
#19352 = ADVANCED_FACE ( 'NONE', ( #19814 ), #16576, .T. ) ;
#19353 = VERTEX_POINT ( 'NONE', #38752 ) ;
#19354 = DIRECTION ( 'NONE',  ( -3.071710424422018668E-17, 6.404604876783312462E-16, 1.000000000000000000 ) ) ;
#19355 = DIRECTION ( 'NONE',  ( -0.2465957053274583366, -0.9635866743705473469, 0.1033986416233890621 ) ) ;
#19356 = EDGE_LOOP ( 'NONE', ( #35569, #21337, #37116, #30234, #34080 ) ) ;
#19357 = CARTESIAN_POINT ( 'NONE',  ( -23.04367560227575140, -10.55211830211007218, 59.60203429193362012 ) ) ;
#19358 = VERTEX_POINT ( 'NONE', #23761 ) ;
#19359 = ORIENTED_EDGE ( 'NONE', *, *, #7835, .F. ) ;
#19360 = ORIENTED_EDGE ( 'NONE', *, *, #36660, .T. ) ;
#19361 = CARTESIAN_POINT ( 'NONE',  ( -22.23802311999876480, -19.89335690450594996, 69.28490980393287657 ) ) ;
#19362 = CARTESIAN_POINT ( 'NONE',  ( -17.28496127917699710, -14.43418371046636217, 54.49999999999994316 ) ) ;
#19363 = CARTESIAN_POINT ( 'NONE',  ( -16.25534385759799250, -8.623186033802570094, 49.24843789510467218 ) ) ;
#19364 =( BOUNDED_CURVE ( )  B_SPLINE_CURVE ( 3, ( #37555, #3596, #18362, #7316 ),
 .UNSPECIFIED., .F., .F. ) 
 B_SPLINE_CURVE_WITH_KNOTS ( ( 4, 4 ),
 ( 0.4074455897393651216, 0.5000000000000000000 ),
 .UNSPECIFIED. ) 
 CURVE ( )  GEOMETRIC_REPRESENTATION_ITEM ( )  RATIONAL_B_SPLINE_CURVE ( ( 0.6983129098260971723, 0.7760317562607096376, 0.8765941196520130596, 1.000000000000012657 ) ) 
 REPRESENTATION_ITEM ( '' )  );
#19365 = CARTESIAN_POINT ( 'NONE',  ( -24.13566541640272334, -12.82032643073200440, 66.37534717750864388 ) ) ;
#19366 = EDGE_CURVE ( 'NONE', #3652, #17695, #12904, .T. ) ;
#19367 = DIRECTION ( 'NONE',  ( -3.071710424422018668E-17, 6.404604876783312462E-16, 1.000000000000000000 ) ) ;
#19368 = LINE ( 'NONE', #37579, #42529 ) ;
#19369 = EDGE_CURVE ( 'NONE', #33919, #38352, #11149, .T. ) ;
#19370 = ORIENTED_EDGE ( 'NONE', *, *, #33689, .T. ) ;
#19371 = VERTEX_POINT ( 'NONE', #12405 ) ;
#19372 = B_SPLINE_CURVE_WITH_KNOTS ( 'NONE', 3,
 ( #21368, #36356, #44028, #2634, #17641, #32672, #25299, #41524, #7561, #33621 ),
 .UNSPECIFIED., .F., .F.,
 ( 4, 2, 2, 2, 4 ),
 ( 0.6272669072877536944, 0.7522669073072811852, 0.8772669073268085649, 1.002266907346335945, 1.127266907365863435 ),
 .UNSPECIFIED. ) ;
#19373 = CARTESIAN_POINT ( 'NONE',  ( -15.32518304399999387, -21.95751765168108349, 72.16080051677664642 ) ) ;
#19374 = ADVANCED_FACE ( 'NONE', ( #8244 ), #24234, .T. ) ;
#19375 = ADVANCED_FACE ( 'NONE', ( #20043 ), #12169, .T. ) ;
#19376 = CARTESIAN_POINT ( 'NONE',  ( -13.18148061888732414, -8.602323747283376676, 54.02312124697527906 ) ) ;
#19377 = DIRECTION ( 'NONE',  ( 1.927470528863119542E-16, 0.000000000000000000, -1.000000000000000000 ) ) ;
#19378 = CARTESIAN_POINT ( 'NONE',  ( -23.23311957587295495, -18.80921362937865382, 69.70860875969677295 ) ) ;
#19379 = VERTEX_POINT ( 'NONE', #35050 ) ;
#19380 = CARTESIAN_POINT ( 'NONE',  ( -16.33659385650551599, -6.915538690918074494, 49.31353937987644542 ) ) ;
#19381 =( BOUNDED_CURVE ( )  B_SPLINE_CURVE ( 3, ( #15292, #25661, #21977, #11144 ),
 .UNSPECIFIED., .F., .F. ) 
 B_SPLINE_CURVE_WITH_KNOTS ( ( 4, 4 ),
 ( 0.000000000000000000, 0.4074455897393662873 ),
 .UNSPECIFIED. ) 
 CURVE ( )  GEOMETRIC_REPRESENTATION_ITEM ( )  RATIONAL_B_SPLINE_CURVE ( ( 1.000000000000000000, 0.4567392136813295256, 0.3561768502900293787, 0.6983129098260995038 ) ) 
 REPRESENTATION_ITEM ( '' )  );
#19382 = VECTOR ( 'NONE', #25949, 1000.000000000000114 ) ;
#19383 = CIRCLE ( 'NONE', #27257, 0.5000000000000004441 ) ;
#19384 = B_SPLINE_CURVE_WITH_KNOTS ( 'NONE', 3,
 ( #1743, #35937, #47290, #42864, #13762, #32017, #36177, #9858, #28073, #17472 ),
 .UNSPECIFIED., .F., .F.,
 ( 4, 2, 2, 2, 4 ),
 ( 0.6272669072878153118, 0.7522669073073335877, 0.8772669073268517526, 1.002266907346370139, 1.127266907365888304 ),
 .UNSPECIFIED. ) ;
#19385 = ORIENTED_EDGE ( 'NONE', *, *, #36266, .T. ) ;
#19386 = CARTESIAN_POINT ( 'NONE',  ( -16.16816302088245649, -21.69572814894516100, 58.28585623287596462 ) ) ;
#19387 = CARTESIAN_POINT ( 'NONE',  ( -23.25757785049868787, -10.17517560731475967, 63.18690593950643120 ) ) ;
#19388 = B_SPLINE_CURVE_WITH_KNOTS ( 'NONE', 1,
 ( #25325, #36142 ),
 .UNSPECIFIED., .F., .F.,
 ( 2, 2 ),
 ( 0.000000000000000000, 1.000000000000000000 ),
 .UNSPECIFIED. ) ;
#19389 = CARTESIAN_POINT ( 'NONE',  ( -15.26068241199881648, -21.46662293872147842, 68.87592932306560556 ) ) ;
#19390 = VERTEX_POINT ( 'NONE', #8476 ) ;
#19391 = CARTESIAN_POINT ( 'NONE',  ( -41.30484860654427592, -14.90920654474427565, 71.95396199095020506 ) ) ;
#19392 = CARTESIAN_POINT ( 'NONE',  ( -22.05233278088557825, -8.971020610563387621, 63.35187109495049640 ) ) ;
#19393 = EDGE_CURVE ( 'NONE', #12430, #22085, #29371, .T. ) ;
#19394 = CARTESIAN_POINT ( 'NONE',  ( -12.15399223456666178, -9.543296633619027247, 57.20440205305690995 ) ) ;
#19395 = ORIENTED_EDGE ( 'NONE', *, *, #19714, .T. ) ;
#19396 = CARTESIAN_POINT ( 'NONE',  ( -23.61204096558246235, -11.53669824655086451, 66.72214514747398084 ) ) ;
#19397 = DIRECTION ( 'NONE',  ( 0.000000000000000000, 0.000000000000000000, 1.000000000000000000 ) ) ;
#19398 = ORIENTED_EDGE ( 'NONE', *, *, #46255, .F. ) ;
#19399 = CARTESIAN_POINT ( 'NONE',  ( -11.12358220677134035, -11.75903396576748605, 71.08860871065073184 ) ) ;
#19400 = EDGE_LOOP ( 'NONE', ( #2248, #15710, #6857, #32991 ) ) ;
#19401 = CARTESIAN_POINT ( 'NONE',  ( -10.31152747832866545, -17.02635028487499724, 57.86573311178444357 ) ) ;
#19402 = CARTESIAN_POINT ( 'NONE',  ( -24.40614610099494541, -15.84163519271677956, 62.74895499471147531 ) ) ;
#19403 = ORIENTED_EDGE ( 'NONE', *, *, #11661, .T. ) ;
#19404 = DIRECTION ( 'NONE',  ( 0.1922068328301544116, 0.9813544382196450755, -7.804899501647045773E-08 ) ) ;
#19405 = LINE ( 'NONE', #42310, #38349 ) ;
#19406 = EDGE_CURVE ( 'NONE', #15202, #48304, #38156, .T. ) ;
#19407 = EDGE_LOOP ( 'NONE', ( #410, #36724, #21326, #44353 ) ) ;
#19408 = CARTESIAN_POINT ( 'NONE',  ( -21.35242735686129478, -20.60316130439240112, 72.52446376371732129 ) ) ;
#19409 = PRODUCT_DEFINITION_CONTEXT ( 'detailed design', #42294, 'design' ) ;
#19410 = CARTESIAN_POINT ( 'NONE',  ( -11.10681587527927938, -11.67891925637714401, 71.10332952723315714 ) ) ;
#19411 = ORIENTED_EDGE ( 'NONE', *, *, #30253, .T. ) ;
#19412 = CARTESIAN_POINT ( 'NONE',  ( -12.55788482626217650, -9.703832430577184809, 57.50424130074089391 ) ) ;
#19413 = VECTOR ( 'NONE', #9321, 1000.000000000000000 ) ;
#19414 = VECTOR ( 'NONE', #24500, 1000.000000000000000 ) ;
#19415 = CARTESIAN_POINT ( 'NONE',  ( -23.31471867911119489, -19.37025309988949573, 59.08421845897321845 ) ) ;
#19416 = ORIENTED_EDGE ( 'NONE', *, *, #20252, .F. ) ;
#19417 = ORIENTED_EDGE ( 'NONE', *, *, #10488, .T. ) ;
#19418 = CARTESIAN_POINT ( 'NONE',  ( -24.84738384818810175, -14.17746907932909295, 69.77462523386947169 ) ) ;
#19419 = CARTESIAN_POINT ( 'NONE',  ( -46.33910710821349710, -14.20920654474410760, 70.87000000000000455 ) ) ;
#19420 = LINE ( 'NONE', #7876, #20182 ) ;
#19421 = CIRCLE ( 'NONE', #4520, 1.999999999999994893 ) ;
#19422 = CARTESIAN_POINT ( 'NONE',  ( -20.61159385650551812, -6.922745924619793101, 51.69366785382590024 ) ) ;
#19423 = CARTESIAN_POINT ( 'NONE',  ( -14.05371270701021480, -21.00138147690670820, 71.92607703580544865 ) ) ;
#19424 = CARTESIAN_POINT ( 'NONE',  ( -24.11031341057265465, -17.05596264031881759, 69.62159819203986899 ) ) ;
#19425 = CARTESIAN_POINT ( 'NONE',  ( -17.52853272358826686, -7.759682304905023642, 63.83584969886392457 ) ) ;
#19426 = CARTESIAN_POINT ( 'NONE',  ( -10.79646186035629540, -11.40653701787342200, 67.66218675276181216 ) ) ;
#19427 = ORIENTED_EDGE ( 'NONE', *, *, #45921, .F. ) ;
#19428 = B_SPLINE_CURVE_WITH_KNOTS ( 'NONE', 3,
 ( #15171, #45015, #45490, #4596, #34136, #7825, #11992, #37332, #11748, #29978 ),
 .UNSPECIFIED., .F., .F.,
 ( 4, 2, 2, 2, 4 ),
 ( 0.1272669073658183880, 0.2522669073463058576, 0.3772669073267932438, 0.5022669073072807411, 0.6272669072877681273 ),
 .UNSPECIFIED. ) ;
#19429 = CARTESIAN_POINT ( 'NONE',  ( -22.94085508618206859, -9.802298960702817254, 70.19673832247809742 ) ) ;
#19430 = EDGE_CURVE ( 'NONE', #14105, #20348, #22296, .T. ) ;
#19431 = EDGE_CURVE ( 'NONE', #25847, #47981, #21264, .T. ) ;
#19432 =( NAMED_UNIT ( * ) PLANE_ANGLE_UNIT ( ) SI_UNIT ( $, .RADIAN. ) );
#19433 = CARTESIAN_POINT ( 'NONE',  ( -24.53366638517183773, -12.58233285770469578, 69.91096473585081128 ) ) ;
#19434 = CARTESIAN_POINT ( 'NONE',  ( -12.46122051107220230, -19.81685944811288635, 64.88146935704573082 ) ) ;
#19435 = VERTEX_POINT ( 'NONE', #35773 ) ;
#19436 = EDGE_CURVE ( 'NONE', #5003, #18340, #7117, .T. ) ;
#19437 = ADVANCED_FACE ( 'NONE', ( #36260 ), #11044, .T. ) ;
#19438 = VERTEX_POINT ( 'NONE', #13363 ) ;
#19439 = CARTESIAN_POINT ( 'NONE',  ( -4.924093855413050669, -6.859206544744110623, 52.99999999999998579 ) ) ;
#19440 = CARTESIAN_POINT ( 'NONE',  ( -23.82366728017863622, -10.99486018697619372, 73.47698013610775547 ) ) ;
#19441 = CARTESIAN_POINT ( 'NONE',  ( -15.34627850953772743, -21.96360194435002455, 72.14601215069538398 ) ) ;
#19442 = CARTESIAN_POINT ( 'NONE',  ( -24.72409385541305582, -14.80920654474425291, 71.98235294117645822 ) ) ;
#19443 = ORIENTED_EDGE ( 'NONE', *, *, #45204, .T. ) ;
#19444 = CARTESIAN_POINT ( 'NONE',  ( -13.02800281770400659, -9.361645100181775092, 71.14925385330717234 ) ) ;
#19445 = VECTOR ( 'NONE', #12458, 1000.000000000000227 ) ;
#19446 = VECTOR ( 'NONE', #38590, 1000.000000000000114 ) ;
#19447 = CYLINDRICAL_SURFACE ( 'NONE', #32755, 0.1500000000000054345 ) ;
#19448 = EDGE_CURVE ( 'NONE', #10107, #13759, #24951, .T. ) ;
#19449 = ORIENTED_EDGE ( 'NONE', *, *, #7236, .T. ) ;
#19450 = AXIS2_PLACEMENT_3D ( 'NONE', #35495, #15808, #23465 ) ;
#19451 = CARTESIAN_POINT ( 'NONE',  ( -11.10300763040008398, -10.86615618544839457, 57.39398486019972268 ) ) ;
#19452 = CARTESIAN_POINT ( 'NONE',  ( -13.78028125966771178, -8.764572710043150749, 74.35521961121672518 ) ) ;
#19453 = ORIENTED_EDGE ( 'NONE', *, *, #36771, .T. ) ;
#19454 = CARTESIAN_POINT ( 'NONE',  ( -21.76140116446488193, -9.313237301066212837, 66.73320317296904136 ) ) ;
#19455 = ORIENTED_EDGE ( 'NONE', *, *, #29887, .F. ) ;
#19456 = DIRECTION ( 'NONE',  ( 0.1453014101478983799, 0.9893874368562763921, 1.082933083898391864E-18 ) ) ;
#19457 = CARTESIAN_POINT ( 'NONE',  ( -11.57017261513264117, -10.87519553945718620, 57.62392099249677102 ) ) ;
#19458 = VERTEX_POINT ( 'NONE', #17547 ) ;
#19459 = CARTESIAN_POINT ( 'NONE',  ( -11.98528268197933322, -9.717857698500944608, 60.70918086974133843 ) ) ;
#19460 = CARTESIAN_POINT ( 'NONE',  ( -24.43113015230203544, -15.58634353390661964, 73.15303748141660378 ) ) ;
#19461 = CARTESIAN_POINT ( 'NONE',  ( -17.21159385650551599, -6.922745924619793101, 51.69366785382590024 ) ) ;
#19462 = CARTESIAN_POINT ( 'NONE',  ( -10.74573065459234478, -12.54952415110468422, 60.81325645027152405 ) ) ;
#19463 = CARTESIAN_POINT ( 'NONE',  ( -22.21838695824825294, -9.106656223178038800, 59.84358462373373300 ) ) ;
#19464 = ORIENTED_EDGE ( 'NONE', *, *, #16524, .T. ) ;
#19465 = CARTESIAN_POINT ( 'NONE',  ( -46.29409385541305966, -16.70920654474410938, 70.50000000000000000 ) ) ;
#19466 = CARTESIAN_POINT ( 'NONE',  ( -16.56159385541304019, -7.228003583438115776, 51.38655588711986155 ) ) ;
#19467 = CARTESIAN_POINT ( 'NONE',  ( -12.50766578132126305, -19.86205079821699115, 65.16674886870754335 ) ) ;
#19468 = CYLINDRICAL_SURFACE ( 'NONE', #16409, 2.000000000000001776 ) ;
#19469 = CARTESIAN_POINT ( 'NONE',  ( -24.76306277605930717, -16.09159651786607625, 66.22471475759273574 ) ) ;
#19470 = ORIENTED_EDGE ( 'NONE', *, *, #11172, .T. ) ;
#19471 = ORIENTED_EDGE ( 'NONE', *, *, #3199, .F. ) ;
#19472 = CARTESIAN_POINT ( 'NONE',  ( -18.20082364030551503, -7.794104720362528660, 73.99631248270939921 ) ) ;
#19473 = CARTESIAN_POINT ( 'NONE',  ( -10.35899127153216881, -12.44516180055180143, 60.92136665175527099 ) ) ;
#19474 = ORIENTED_EDGE ( 'NONE', *, *, #14401, .F. ) ;
#19476 = LINE ( 'NONE', #30585, #24129 ) ;
#19475 = AXIS2_PLACEMENT_3D ( 'NONE', #12191, #42483, #1334 ) ;
#19477 = CARTESIAN_POINT ( 'NONE',  ( -14.57480141982250998, -21.69281262657844067, 58.31617885369491461 ) ) ;
#19478 = CARTESIAN_POINT ( 'NONE',  ( -22.10534385759799036, -7.595227055684746986, 51.75156210489594599 ) ) ;
#19479 = DIRECTION ( 'NONE',  ( -0.3667195576449454042, 0.9303315355510073381, 1.591455084066143578E-08 ) ) ;
#19480 = CARTESIAN_POINT ( 'NONE',  ( -12.07387405703792460, -19.99358258471635708, 61.59689830162205482 ) ) ;
#19481 = CARTESIAN_POINT ( 'NONE',  ( -11.40643119260009364, -19.20155754982889817, 71.82652555106689363 ) ) ;
#19482 = AXIS2_PLACEMENT_3D ( 'NONE', #44160, #47985, #47737 ) ;
#19483 = CARTESIAN_POINT ( 'NONE',  ( -24.25068033110073173, -17.79252971020026663, 62.62360985091944343 ) ) ;
#19484 = AXIS2_PLACEMENT_3D ( 'NONE', #46947, #10261, #16891 ) ;
#19485 = ORIENTED_EDGE ( 'NONE', *, *, #47663, .F. ) ;
#19486 = DIRECTION ( 'NONE',  ( -2.866981220435666553E-17, 1.000000000000000000, 1.190614954331866791E-16 ) ) ;
#19487 = EDGE_CURVE ( 'NONE', #13527, #33162, #44047, .T. ) ;
#19488 = FILL_AREA_STYLE ('',( #16257 ) ) ;
#19489 = DIRECTION ( 'NONE',  ( -0.9687793358424822143, 0.2479245821708672415, 0.000000000000000000 ) ) ;
#19490 = CARTESIAN_POINT ( 'NONE',  ( -13.90792234543431327, -20.92405545593893379, 64.98628592218737765 ) ) ;
#19491 = CARTESIAN_POINT ( 'NONE',  ( -12.83007281553047108, -20.09077549419061626, 71.80653676829817300 ) ) ;
#19492 = CARTESIAN_POINT ( 'NONE',  ( -18.12273512012592747, -22.22646200727865917, 65.46036854067777710 ) ) ;
#19493 = VECTOR ( 'NONE', #41592, 1000.000000000000000 ) ;
#19494 = ORIENTED_EDGE ( 'NONE', *, *, #30819, .F. ) ;
#19495 = EDGE_LOOP ( 'NONE', ( #32516, #34149, #18805, #18489, #23148, #14092 ) ) ;
#19496 = ADVANCED_FACE ( 'NONE', ( #17052 ), #13599, .T. ) ;
#19497 = B_SPLINE_CURVE_WITH_KNOTS ( 'NONE', 3,
 ( #28656, #13370, #27686, #9470, #47381, #24495, #39734, #28420, #1577, #31378 ),
 .UNSPECIFIED., .F., .F.,
 ( 4, 2, 2, 2, 4 ),
 ( 0.000000000000000000, 0.2500000000000000000, 0.5000000000000000000, 0.7500000000000000000, 1.000000000000000000 ),
 .UNSPECIFIED. ) ;
#19498 = ORIENTED_EDGE ( 'NONE', *, *, #4971, .T. ) ;
#19499 = CARTESIAN_POINT ( 'NONE',  ( -11.96084830514426400, -9.743959610980004626, 60.74413522332266524 ) ) ;
#19500 = EDGE_CURVE ( 'NONE', #32337, #8240, #21119, .T. ) ;
#19501 = CARTESIAN_POINT ( 'NONE',  ( -16.47491545697456061, -21.74461699364392686, 62.04102722053536212 ) ) ;
#19502 = EDGE_CURVE ( 'NONE', #40722, #5535, #5543, .T. ) ;
#19503 =( BOUNDED_CURVE ( )  B_SPLINE_CURVE ( 3, ( #21897, #25121, #21435, #40141 ),
 .UNSPECIFIED., .F., .F. ) 
 B_SPLINE_CURVE_WITH_KNOTS ( ( 4, 4 ),
 ( 0.4074455897393699511, 0.5000000000000000000 ),
 .UNSPECIFIED. ) 
 CURVE ( )  GEOMETRIC_REPRESENTATION_ITEM ( )  RATIONAL_B_SPLINE_CURVE ( ( 0.6983129098261027234, 0.7760317562607084163, 0.8765941196520080636, 1.000000000000002887 ) ) 
 REPRESENTATION_ITEM ( '' )  );
#19504 = DIRECTION ( 'NONE',  ( 1.000000000000000000, 2.866981220435666553E-17, 0.000000000000000000 ) ) ;
#19505 = CARTESIAN_POINT ( 'NONE',  ( -13.73970650151387751, -20.76112128469266693, 64.98628881673506896 ) ) ;
#19506 = FACE_OUTER_BOUND ( 'NONE', #33186, .T. ) ;
#19507 = ADVANCED_FACE ( 'NONE', ( #5989 ), #3009, .T. ) ;
#19508 = ORIENTED_EDGE ( 'NONE', *, *, #4504, .F. ) ;
#19509 = CARTESIAN_POINT ( 'NONE',  ( -23.80321451250838649, -17.81075939459467961, 59.00378417737415049 ) ) ;
#19510 = AXIS2_PLACEMENT_3D ( 'NONE', #24752, #42968, #32609 ) ;
#19511 = DIRECTION ( 'NONE',  ( 0.3109111061729914471, 0.9504389954427826526, 3.354176643444177759E-08 ) ) ;
#19512 = VECTOR ( 'NONE', #30100, 1000.000000000000114 ) ;
#19513 = EDGE_LOOP ( 'NONE', ( #45861, #22293, #42933, #14432, #34874, #12932, #15397, #14676 ) ) ;
#19514 =( BOUNDED_CURVE ( )  B_SPLINE_CURVE ( 3, ( #47038, #13281, #43362, #8815 ),
 .UNSPECIFIED., .F., .F. ) 
 B_SPLINE_CURVE_WITH_KNOTS ( ( 4, 4 ),
 ( 0.000000000000000000, 0.4074455897393678416 ),
 .UNSPECIFIED. ) 
 CURVE ( )  GEOMETRIC_REPRESENTATION_ITEM ( )  RATIONAL_B_SPLINE_CURVE ( ( 1.000000000000000000, 0.4567392136813320791, 0.3561768502900303779, 0.6983129098260949519 ) ) 
 REPRESENTATION_ITEM ( '' )  );
#19515 = CARTESIAN_POINT ( 'NONE',  ( -14.72744631621160494, -8.295007313424175521, 60.60524229057013201 ) ) ;
#19516 = VECTOR ( 'NONE', #9734, 1000.000000000000227 ) ;
#19517 = CIRCLE ( 'NONE', #47046, 4.686499999999997890 ) ;
#19518 = VERTEX_POINT ( 'NONE', #28411 ) ;
#19519 = LINE ( 'NONE', #8210, #27582 ) ;
#19520 = DIRECTION ( 'NONE',  ( 1.000000000000000000, 0.000000000000000000, 0.000000000000000000 ) ) ;
#19521 = CARTESIAN_POINT ( 'NONE',  ( -24.05845762361657947, -12.57644656616312773, 73.24225570276865938 ) ) ;
#19522 = ORIENTED_EDGE ( 'NONE', *, *, #1154, .F. ) ;
#19523 = CARTESIAN_POINT ( 'NONE',  ( -12.74836358285320159, -20.08597126951521261, 71.82125749157572159 ) ) ;
#19524 = CARTESIAN_POINT ( 'NONE',  ( -50.42609385541305755, -14.80920654474411613, 58.90588235294116970 ) ) ;
#19525 = AXIS2_PLACEMENT_3D ( 'NONE', #46316, #20453, #35453 ) ;
#19526 = CARTESIAN_POINT ( 'NONE',  ( -18.31357888663955080, -21.80286911112441217, 69.11514702303101387 ) ) ;
#19527 = CARTESIAN_POINT ( 'NONE',  ( -24.72409385541305582, -14.80920654474422271, 68.06470588235292496 ) ) ;
#19528 = CARTESIAN_POINT ( 'NONE',  ( -17.66159385759798894, -7.228003583438117552, 51.38655588711986155 ) ) ;
#19529 = CARTESIAN_POINT ( 'NONE',  ( -20.54979434103954006, -8.489990112051950533, 63.61121512946457557 ) ) ;
#19530 =( BOUNDED_CURVE ( )  B_SPLINE_CURVE ( 3, ( #31135, #8257, #42720, #27689 ),
 .UNSPECIFIED., .F., .F. ) 
 B_SPLINE_CURVE_WITH_KNOTS ( ( 4, 4 ),
 ( 0.000000000000000000, 0.4074455897393666204 ),
 .UNSPECIFIED. ) 
 CURVE ( )  GEOMETRIC_REPRESENTATION_ITEM ( )  RATIONAL_B_SPLINE_CURVE ( ( 1.000000000000000000, 0.4567392136813317460, 0.3561768502900302114, 0.6983129098260953960 ) ) 
 REPRESENTATION_ITEM ( '' )  );
#19531 = DIRECTION ( 'NONE',  ( -9.880513536971593873E-06, -1.241746728590076822E-06, 0.9999999999504166626 ) ) ;
#19532 = CARTESIAN_POINT ( 'NONE',  ( -23.93063274373519178, -11.18025648668110783, 70.07023518370729676 ) ) ;
#19533 = FACE_OUTER_BOUND ( 'NONE', #27738, .T. ) ;
#19534 = CARTESIAN_POINT ( 'NONE',  ( -20.78034385650551386, -6.424090610841176385, 49.80797279389978627 ) ) ;
#19535 = ORIENTED_EDGE ( 'NONE', *, *, #4783, .T. ) ;
#19536 = CARTESIAN_POINT ( 'NONE',  ( -15.64104502085146642, -10.46221995643221270, 49.52966884056655772 ) ) ;
#19537 = CARTESIAN_POINT ( 'NONE',  ( -21.84079884060555088, -9.314189094968263305, 63.34153755726884327 ) ) ;
#19538 = VERTEX_POINT ( 'NONE', #21016 ) ;
#19539 = DIRECTION ( 'NONE',  ( -0.000000000000000000, -1.000000000000000000, -0.000000000000000000 ) ) ;
#19540 = CARTESIAN_POINT ( 'NONE',  ( -24.46601827249642014, -14.47102098010720006, 66.18292729753066794 ) ) ;
#19541 = CARTESIAN_POINT ( 'NONE',  ( -18.73521446872676322, -7.879141670414848697, 74.25553277440172906 ) ) ;
#19542 = B_SPLINE_CURVE_WITH_KNOTS ( 'NONE', 3,
 ( #26265, #15161, #44755, #29968, #45006, #7817, #11252, #22832, #38062, #11738 ),
 .UNSPECIFIED., .F., .F.,
 ( 4, 2, 2, 2, 4 ),
 ( 0.000000000000000000, 0.2500000000000000000, 0.5000000000000000000, 0.7500000000000000000, 1.000000000000000000 ),
 .UNSPECIFIED. ) ;
#19543 = EDGE_CURVE ( 'NONE', #21555, #46504, #7609, .T. ) ;
#19544 = ORIENTED_EDGE ( 'NONE', *, *, #5345, .F. ) ;
#19545 = CARTESIAN_POINT ( 'NONE',  ( -18.37786432726835883, -21.79469297182707521, 69.10042588711679912 ) ) ;
#19546 = LINE ( 'NONE', #34556, #21004 ) ;
#19547 = CARTESIAN_POINT ( 'NONE',  ( -12.04811195874215812, -10.23604714248314629, 60.71485379904431312 ) ) ;
#19548 = ADVANCED_FACE ( 'NONE', ( #2295 ), #17644, .T. ) ;
#19549 = ORIENTED_EDGE ( 'NONE', *, *, #36273, .F. ) ;
#19550 = CARTESIAN_POINT ( 'NONE',  ( -11.32469144785209103, -18.34471071427194389, 57.80714594245691273 ) ) ;
#19551 = CIRCLE ( 'NONE', #31362, 2.000000000000001332 ) ;
#19552 = DIRECTION ( 'NONE',  ( 1.000000000000000000, -4.164305804376849172E-17, 1.614929280266638808E-16 ) ) ;
#19553 = CIRCLE ( 'NONE', #35291, 1.999999999999999112 ) ;
#19554 = CARTESIAN_POINT ( 'NONE',  ( -10.00037608677762258, -14.17511115329010707, 61.03165943758897782 ) ) ;
#19555 = CARTESIAN_POINT ( 'NONE',  ( -19.86569447268031041, -19.73755174630646891, 53.49999999999995026 ) ) ;
#19556 = CARTESIAN_POINT ( 'NONE',  ( -23.16129546718040189, -18.81986427065789158, 62.58080139315423907 ) ) ;
#19557 = AXIS2_PLACEMENT_3D ( 'NONE', #35580, #12211, #20333 ) ;
#19558 = VECTOR ( 'NONE', #44119, 999.9999999999998863 ) ;
#19559 = ORIENTED_EDGE ( 'NONE', *, *, #31239, .F. ) ;
#19560 = EDGE_LOOP ( 'NONE', ( #22820, #47582, #40553, #15255, #18236 ) ) ;
#19561 = CARTESIAN_POINT ( 'NONE',  ( -22.13034385541304161, -6.857644439848013640, 49.98602051094139398 ) ) ;
#19562 = CARTESIAN_POINT ( 'NONE',  ( -20.92409385541305511, -10.10920654474410618, 80.49999999999998579 ) ) ;
#19563 = EDGE_CURVE ( 'NONE', #15772, #39638, #44642, .T. ) ;
#19564 = CARTESIAN_POINT ( 'NONE',  ( -41.15852941833841783, -25.10920654474410441, 54.99999999999997868 ) ) ;
#19565 = CIRCLE ( 'NONE', #6173, 2.000000000000001776 ) ;
#19566 = CARTESIAN_POINT ( 'NONE',  ( -17.73224099643095286, -22.30287356026373047, 53.49999999999994316 ) ) ;
#19567 = EDGE_CURVE ( 'NONE', #43051, #20660, #22712, .T. ) ;
#19568 = ADVANCED_FACE ( 'NONE', ( #33513 ), #23633, .T. ) ;
#19569 = CARTESIAN_POINT ( 'NONE',  ( -11.81042834955647258, -10.54382735031610174, 74.45357240259568243 ) ) ;
#19570 = CARTESIAN_POINT ( 'NONE',  ( -17.98584164848810474, -22.23808382151284491, 62.06031347038508983 ) ) ;
#19571 = CARTESIAN_POINT ( 'NONE',  ( -12.26752988409003287, -16.72227946798956921, 53.49999999999995026 ) ) ;
#19572 = DIRECTION ( 'NONE',  ( 0.9687793358424822143, -0.2479245821708672415, 0.000000000000000000 ) ) ;
#19573 = ADVANCED_FACE ( 'NONE', ( #11380 ), #26403, .T. ) ;
#19574 = ORIENTED_EDGE ( 'NONE', *, *, #1678, .T. ) ;
#19575 = CARTESIAN_POINT ( 'NONE',  ( -21.20678976440764885, -20.70065158789174475, 72.59616802899515164 ) ) ;
#19576 = CARTESIAN_POINT ( 'NONE',  ( -22.06352374043166265, -8.980015506435984562, 63.37649162950052784 ) ) ;
#19577 = ORIENTED_EDGE ( 'NONE', *, *, #41809, .T. ) ;
#19578 = CARTESIAN_POINT ( 'NONE',  ( -11.06712629860931152, -18.69414434431124761, 61.39215439313597500 ) ) ;
#19579 = CARTESIAN_POINT ( 'NONE',  ( -9.974215857974789046, -14.86484893678357544, 74.91283499353951925 ) ) ;
#19580 = CARTESIAN_POINT ( 'NONE',  ( -10.55151165865014384, -17.68520938540437371, 68.28217272534745064 ) ) ;
#19581 = CARTESIAN_POINT ( 'NONE',  ( -13.22529448846758982, -9.145569705956512863, 64.19474388871357462 ) ) ;
#19582 = ORIENTED_EDGE ( 'NONE', *, *, #46518, .F. ) ;
#19583 = CARTESIAN_POINT ( 'NONE',  ( -10.78898398081525301, -17.19290454168847404, 61.44271037915215317 ) ) ;
#19584 = AXIS2_PLACEMENT_3D ( 'NONE', #39709, #10159, #5506 ) ;
#19585 = FACE_OUTER_BOUND ( 'NONE', #21476, .T. ) ;
#19586 = CYLINDRICAL_SURFACE ( 'NONE', #33908, 1.250000000000001110 ) ;
#19587 = ORIENTED_EDGE ( 'NONE', *, *, #759, .F. ) ;
#19588 = CARTESIAN_POINT ( 'NONE',  ( -10.33960071559749494, -17.11462300555371030, 57.82614026527284778 ) ) ;
#19589 = DIRECTION ( 'NONE',  ( 1.000000000000000000, -4.164305804376849172E-17, 1.614929280266638808E-16 ) ) ;
#19591 = CARTESIAN_POINT ( 'NONE',  ( -23.77312829587014420, -18.70709569252041859, 72.87872954713984086 ) ) ;
#19590 = VECTOR ( 'NONE', #31168, 1000.000000000000000 ) ;
#19592 = CARTESIAN_POINT ( 'NONE',  ( -18.78767905735283605, -20.13749289187802916, 53.49999999999995026 ) ) ;
#19593 = DIRECTION ( 'NONE',  ( 0.000000000000000000, 0.000000000000000000, 1.000000000000000000 ) ) ;
#19594 = DIRECTION ( 'NONE',  ( -0.9999247414263406908, 0.01226831216845469807, 5.367905339378914507E-08 ) ) ;
#19595 = CARTESIAN_POINT ( 'NONE',  ( -22.57893663749957369, -9.999394138389961384, 73.49633153340955971 ) ) ;
#19596 = DIRECTION ( 'NONE',  ( -3.071710424422018668E-17, 6.404604876783312462E-16, 1.000000000000000000 ) ) ;
#19597 = EDGE_LOOP ( 'NONE', ( #6724, #20046, #1957, #29863 ) ) ;
#19598 = CARTESIAN_POINT ( 'NONE',  ( -20.66696756681432134, -21.06910030335248507, 58.64475164910060556 ) ) ;
#19599 = VECTOR ( 'NONE', #15890, 1000.000000000000114 ) ;
#19600 = EDGE_LOOP ( 'NONE', ( #43400, #29550, #5819, #33050 ) ) ;
#19601 = CARTESIAN_POINT ( 'NONE',  ( -17.42409385541299471, -14.80920654474435594, 52.02966884056656482 ) ) ;
#19602 = CARTESIAN_POINT ( 'NONE',  ( -24.72409385541305582, -14.80920654474417830, 64.94117647058821774 ) ) ;
#19603 = ADVANCED_FACE ( 'NONE', ( #14544 ), #3499, .T. ) ;
#19604 = VERTEX_POINT ( 'NONE', #18511 ) ;
#19605 = DIRECTION ( 'NONE',  ( 0.2479245821708712938, 0.9687793358424811041, 0.000000000000000000 ) ) ;
#19606 = FACE_BOUND ( 'NONE', #3079, .T. ) ;
#19607 = ORIENTED_EDGE ( 'NONE', *, *, #43642, .F. ) ;
#19608 = ORIENTED_EDGE ( 'NONE', *, *, #31988, .F. ) ;
#19609 = ORIENTED_EDGE ( 'NONE', *, *, #33045, .T. ) ;
#19610 = CARTESIAN_POINT ( 'NONE',  ( -18.05557233295238362, -22.23314744338585669, 61.98880637900742130 ) ) ;
#19611 = CARTESIAN_POINT ( 'NONE',  ( -12.61446418420489124, -20.49964817803554595, 71.91998392462126333 ) ) ;
#19612 = CARTESIAN_POINT ( 'NONE',  ( -33.95962776134579286, -8.109206544744111511, 49.25000000000000000 ) ) ;
#19613 = B_SPLINE_CURVE_WITH_KNOTS ( 'NONE', 3,
 ( #35813, #47880, #36055, #17346, #46914, #13154, #13402, #2093, #36300, #28202 ),
 .UNSPECIFIED., .F., .F.,
 ( 4, 2, 2, 2, 4 ),
 ( 0.6272669072877499197, 0.7522669073072704160, 0.8772669073267909123, 1.002266907346311520, 1.127266907365831905 ),
 .UNSPECIFIED. ) ;
#19614 = CARTESIAN_POINT ( 'NONE',  ( -23.83043763270304538, -11.86620476845630101, 59.48235732590899261 ) ) ;
#19615 = DIRECTION ( 'NONE',  ( 0.000000000000000000, 0.000000000000000000, 1.000000000000000000 ) ) ;
#19616 = ADVANCED_FACE ( 'NONE', ( #48081 ), #4425, .T. ) ;
#19617 = CARTESIAN_POINT ( 'NONE',  ( -19.36486374868428584, -8.083171814817379897, 59.97709656101385889 ) ) ;
#19618 = ORIENTED_EDGE ( 'NONE', *, *, #46783, .T. ) ;
#19619 = ORIENTED_EDGE ( 'NONE', *, *, #13070, .F. ) ;
#19620 = FACE_OUTER_BOUND ( 'NONE', #35633, .T. ) ;
#19621 = EDGE_CURVE ( 'NONE', #3056, #36780, #6960, .T. ) ;
#19622 = CARTESIAN_POINT ( 'NONE',  ( -13.71339271347209987, -20.80363700974685059, 65.28628881287177421 ) ) ;
#19623 = VECTOR ( 'NONE', #41778, 1000.000000000000227 ) ;
#19624 = CARTESIAN_POINT ( 'NONE',  ( -19.30272045617997634, -8.014115550771089502, 59.96092997145631642 ) ) ;
#19625 = CARTESIAN_POINT ( 'NONE',  ( -20.75210801675527605, -8.590061315918145368, 63.40301605188658129 ) ) ;
#19626 = EDGE_LOOP ( 'NONE', ( #2566, #44566, #5292, #40750 ) ) ;
#19627 = CARTESIAN_POINT ( 'NONE',  ( -15.77409385650551954, -9.792211528768504536, 50.49490371617623197 ) ) ;
#19628 = VECTOR ( 'NONE', #34677, 1000.000000000000000 ) ;
#19629 = VECTOR ( 'NONE', #29849, 1000.000000000000000 ) ;
#19630 = ORIENTED_EDGE ( 'NONE', *, *, #24665, .F. ) ;
#19631 = EDGE_CURVE ( 'NONE', #14637, #10419, #24353, .T. ) ;
#19632 = B_SPLINE_CURVE_WITH_KNOTS ( 'NONE', 1,
 ( #20957, #25137 ),
 .UNSPECIFIED., .F., .F.,
 ( 2, 2 ),
 ( 0.000000000000000000, 1.000000000000000000 ),
 .UNSPECIFIED. ) ;
#19633 = CARTESIAN_POINT ( 'NONE',  ( -8.424093855413071097, -25.10920654474410441, 52.99999999999997868 ) ) ;
#19634 = CARTESIAN_POINT ( 'NONE',  ( -15.44116676862596549, -21.52247700621390436, 68.68478959089048885 ) ) ;
#19635 = CARTESIAN_POINT ( 'NONE',  ( -24.46783000807617370, -17.23593667955698905, 73.07674329114531986 ) ) ;
#19636 = AXIS2_PLACEMENT_3D ( 'NONE', #43418, #13580, #43658 ) ;
#19637 = EDGE_CURVE ( 'NONE', #18422, #47966, #35888, .T. ) ;
#19638 = B_SPLINE_CURVE_WITH_KNOTS ( 'NONE', 1,
 ( #33075, #26207 ),
 .UNSPECIFIED., .F., .F.,
 ( 2, 2 ),
 ( 0.000000000000000000, 1.000000000000000000 ),
 .UNSPECIFIED. ) ;
#19639 = ORIENTED_EDGE ( 'NONE', *, *, #33783, .T. ) ;
#19640 = DIRECTION ( 'NONE',  ( 0.9687793358424819923, -0.2479245821708678243, 0.000000000000000000 ) ) ;
#19641 = CARTESIAN_POINT ( 'NONE',  ( -10.44938425464750331, -17.42781160170326871, 64.88385290183622089 ) ) ;
#19642 = CARTESIAN_POINT ( 'NONE',  ( -16.17583575424048092, -10.27959207348368764, 49.52966884056655772 ) ) ;
#19643 =( REPRESENTATION_RELATIONSHIP ('NONE','NONE', #2768, #46513 ) REPRESENTATION_RELATIONSHIP_WITH_TRANSFORMATION ( #37811 )SHAPE_REPRESENTATION_RELATIONSHIP( ) );
#19644 = ORIENTED_EDGE ( 'NONE', *, *, #41324, .F. ) ;
#19645 = DIRECTION ( 'NONE',  ( -3.071710424422018668E-17, 6.404604876783312462E-16, 1.000000000000000000 ) ) ;
#19646 =( BOUNDED_SURFACE ( )  B_SPLINE_SURFACE ( 3, 1, ( 
 ( #10584, #2470 ),
 ( #29052, #17709 ),
 ( #47762, #18197 ),
 ( #21664, #2935 ),
 ( #44099, #13768 ),
 ( #29534, #3186 ),
 ( #37142, #17479 ) ),
 .UNSPECIFIED., .T., .F., .F. ) 
 B_SPLINE_SURFACE_WITH_KNOTS ( ( 4, 3, 4 ),
 ( 2, 2 ),
 ( 0.000000000000000000, 0.5000000000000000000, 1.000000000000000000 ),
 ( 0.000000000000000000, 1.000000000000000000 ),
 .UNSPECIFIED. ) 
 GEOMETRIC_REPRESENTATION_ITEM ( )  RATIONAL_B_SPLINE_SURFACE ( (
 ( 1.000000000000000000, 1.000000000000000000),
 ( 0.3333333333333335369, 0.3333333333333330373),
 ( 0.3333333333333335369, 0.3333333333333330373),
 ( 1.000000000000000000, 1.000000000000000000),
 ( 0.3333333333333333703, 0.3333333333333333703),
 ( 0.3333333333333333703, 0.3333333333333333703),
 ( 1.000000000000000000, 1.000000000000000000) ) ) 
 REPRESENTATION_ITEM ( '' )  SURFACE ( )  );
#19647 = EDGE_CURVE ( 'NONE', #3179, #8795, #4089, .T. ) ;
#19648 = B_SPLINE_CURVE_WITH_KNOTS ( 'NONE', 1,
 ( #30874, #30146 ),
 .UNSPECIFIED., .F., .F.,
 ( 2, 2 ),
 ( 0.000000000000000000, 1.000000000000000000 ),
 .UNSPECIFIED. ) ;
#19649 = CARTESIAN_POINT ( 'NONE',  ( -22.94084456310974574, -19.11815116408422810, 59.18410675569454327 ) ) ;
#19650 = CARTESIAN_POINT ( 'NONE',  ( -12.41053161536432725, -20.31997060906338248, 68.45844704426498595 ) ) ;
#19651 = ORIENTED_EDGE ( 'NONE', *, *, #14379, .F. ) ;
#19652 = CARTESIAN_POINT ( 'NONE',  ( -45.37196614242555626, -14.20920654474410760, 70.87000000000000455 ) ) ;
#19653 = EDGE_CURVE ( 'NONE', #14295, #37829, #42820, .T. ) ;
#19654 = ORIENTED_EDGE ( 'NONE', *, *, #41324, .T. ) ;
#19655 = DIRECTION ( 'NONE',  ( -0.000000000000000000, -1.000000000000000000, 9.912705577010318647E-16 ) ) ;
#19656 = CARTESIAN_POINT ( 'NONE',  ( -46.92409385541305511, -15.80920654474410725, 61.49999999999999289 ) ) ;
#19657 = ORIENTED_EDGE ( 'NONE', *, *, #6171, .F. ) ;
#19658 = EDGE_CURVE ( 'NONE', #17957, #41560, #29112, .T. ) ;
#19659 = CARTESIAN_POINT ( 'NONE',  ( -22.16593877863229878, -20.55544301355402581, 58.94255664220460744 ) ) ;
#19660 = FACE_OUTER_BOUND ( 'NONE', #17038, .T. ) ;
#19661 = DIRECTION ( 'NONE',  ( -0.1738928961406289164, 0.9847645711904029486, 7.871847295470929299E-08 ) ) ;
#19662 = AXIS2_PLACEMENT_3D ( 'NONE', #13500, #2434, #24847 ) ;
#19663 = ORIENTED_EDGE ( 'NONE', *, *, #13629, .F. ) ;
#19664 = DIRECTION ( 'NONE',  ( 0.9687793358424817702, -0.2479245821708686570, 0.000000000000000000 ) ) ;
#19665 = CARTESIAN_POINT ( 'NONE',  ( -13.26872317195175199, -21.05283485551296607, 54.27966884056655061 ) ) ;
#19666 =( BOUNDED_CURVE ( )  B_SPLINE_CURVE ( 3, ( #7078, #28988, #28750, #48182 ),
 .UNSPECIFIED., .F., .F. ) 
 B_SPLINE_CURVE_WITH_KNOTS ( ( 4, 4 ),
 ( 0.5000000000000000000, 0.9074455897393729487 ),
 .UNSPECIFIED. ) 
 CURVE ( )  GEOMETRIC_REPRESENTATION_ITEM ( )  RATIONAL_B_SPLINE_CURVE ( ( 1.000000000000021538, 0.4567392136813241410, 0.3561768502900121702, 0.6983129098261091627 ) ) 
 REPRESENTATION_ITEM ( '' )  );
#19667 = CARTESIAN_POINT ( 'NONE',  ( -22.48964968825576705, -9.905448439006629968, 73.76689030015370463 ) ) ;
#19668 = VERTEX_POINT ( 'NONE', #9333 ) ;
#19669 = CARTESIAN_POINT ( 'NONE',  ( -12.10481839165579565, -9.592984239578061789, 57.13289628414671739 ) ) ;
#19670 = AXIS2_PLACEMENT_3D ( 'NONE', #24342, #46264, #39355 ) ;
#19671 = DIRECTION ( 'NONE',  ( 0.000000000000000000, 0.9999954153791273948, 0.003028072113820366902 ) ) ;
#19672 = VERTEX_POINT ( 'NONE', #20162 ) ;
#19673 = VERTEX_POINT ( 'NONE', #28531 ) ;
#19674 = CARTESIAN_POINT ( 'NONE',  ( -22.75923480142028055, -10.27751027444597653, 66.84182257657300852 ) ) ;
#19675 = CARTESIAN_POINT ( 'NONE',  ( -10.69681097496852473, -11.60785472431778942, 71.22714364629104011 ) ) ;
#19676 = DIRECTION ( 'NONE',  ( -3.071710424422018668E-17, 6.404604876783312462E-16, 1.000000000000000000 ) ) ;
#19677 = VECTOR ( 'NONE', #36966, 1000.000000000000114 ) ;
#19678 = CARTESIAN_POINT ( 'NONE',  ( -22.86159385650551457, -9.295667164867525756, 49.30633214617472504 ) ) ;
#19679 = CARTESIAN_POINT ( 'NONE',  ( -10.43125892716163960, -13.91323834088958122, 57.44825034920751960 ) ) ;
#19680 = CARTESIAN_POINT ( 'NONE',  ( -12.15890832635194485, -9.538329179646957812, 57.26748263554841856 ) ) ;
#19681 = CARTESIAN_POINT ( 'NONE',  ( -18.60508437019847960, -7.453401506293143797, 74.04075608594855851 ) ) ;
#19682 =( BOUNDED_CURVE ( )  B_SPLINE_CURVE ( 3, ( #7600, #18645, #25806, #41074 ),
 .UNSPECIFIED., .F., .F. ) 
 B_SPLINE_CURVE_WITH_KNOTS ( ( 4, 4 ),
 ( 0.9074455897393630677, 1.000000000000000000 ),
 .UNSPECIFIED. ) 
 CURVE ( )  GEOMETRIC_REPRESENTATION_ITEM ( )  RATIONAL_B_SPLINE_CURVE ( ( 0.6983129098260782985, 0.7760317562606855457, 0.8765941196519927425, 1.000000000000000000 ) ) 
 REPRESENTATION_ITEM ( '' )  );
#19683 = EDGE_LOOP ( 'NONE', ( #48060, #44946, #9612, #8459, #397 ) ) ;
#19684 = ORIENTED_EDGE ( 'NONE', *, *, #40027, .F. ) ;
#19685 = CARTESIAN_POINT ( 'NONE',  ( -41.42864951152165531, -14.90920654474426499, 70.96355475113121258 ) ) ;
#19686 = CARTESIAN_POINT ( 'NONE',  ( -13.77338061488629073, -21.30427811955188844, 68.56969753575143045 ) ) ;
#19687 = CARTESIAN_POINT ( 'NONE',  ( -12.41310947992116098, -19.76871611099698001, 61.68206578716802113 ) ) ;
#19688 = CARTESIAN_POINT ( 'NONE',  ( -18.39722185058254311, -7.818642594244027855, 70.52634850392742294 ) ) ;
#19689 = VERTEX_POINT ( 'NONE', #9587 ) ;
#19690 = VERTEX_POINT ( 'NONE', #39111 ) ;
#19691 = EDGE_CURVE ( 'NONE', #28180, #44222, #31118, .T. ) ;
#19692 = CARTESIAN_POINT ( 'NONE',  ( -11.75774308769439003, -19.00384223356172697, 71.98685884781659183 ) ) ;
#19693 = CARTESIAN_POINT ( 'NONE',  ( -23.82284107231174630, -10.99348899561931781, 73.61839243124092036 ) ) ;
#19694 = VECTOR ( 'NONE', #7417, 1000.000000000000000 ) ;
#19695 = CARTESIAN_POINT ( 'NONE',  ( -22.11801181964649388, -9.023811091936513762, 63.44799684341401047 ) ) ;
#19696 = CARTESIAN_POINT ( 'NONE',  ( -11.06311696324566007, -18.68765404749363768, 61.39993965581383151 ) ) ;
#19697 = AXIS2_PLACEMENT_3D ( 'NONE', #39449, #31816, #13561 ) ;
#19698 = EDGE_LOOP ( 'NONE', ( #43356, #27450, #31264, #44955, #22699 ) ) ;
#19699 = AXIS2_PLACEMENT_3D ( 'NONE', #10425, #9458, #18018 ) ;
#19700 = CARTESIAN_POINT ( 'NONE',  ( -10.54364274917572963, -16.09770547908457061, 67.99270210874573195 ) ) ;
#19701 = DIRECTION ( 'NONE',  ( 1.000000000000000000, 2.866981220435666553E-17, 0.000000000000000000 ) ) ;
#19702 = EDGE_LOOP ( 'NONE', ( #5135, #42785 ) ) ;
#19703 = B_SPLINE_CURVE_WITH_KNOTS ( 'NONE', 3,
 ( #6172, #31790, #35469, #39168, #43610, #20214, #1990, #24656, #13536, #17482 ),
 .UNSPECIFIED., .F., .F.,
 ( 4, 2, 2, 2, 4 ),
 ( 0.6272669072782244282, 0.7522669073001253537, 0.8772669073220261682, 1.002266907343926983, 1.127266907365827908 ),
 .UNSPECIFIED. ) ;
#19704 = CARTESIAN_POINT ( 'NONE',  ( -11.14114413899577904, -10.80566798617789459, 57.32407932063995304 ) ) ;
#19705 = CARTESIAN_POINT ( 'NONE',  ( -14.25645962476006368, -8.507545769726087670, 74.61443249008125633 ) ) ;
#19706 = VERTEX_POINT ( 'NONE', #2169 ) ;
#19707 = CARTESIAN_POINT ( 'NONE',  ( -17.42409385541300892, -14.80920654474439324, 54.49999999999995026 ) ) ;
#19708 = EDGE_CURVE ( 'NONE', #36678, #9620, #1627, .T. ) ;
#19709 = VERTEX_POINT ( 'NONE', #34932 ) ;
#19710 = DIRECTION ( 'NONE',  ( -3.071710424422018668E-17, 6.404604876783312462E-16, 1.000000000000000000 ) ) ;
#19711 = CARTESIAN_POINT ( 'NONE',  ( -17.78823985852933731, -7.818684566706888717, 60.08060768393342954 ) ) ;
#19712 = VERTEX_POINT ( 'NONE', #28285 ) ;
#19713 = DIRECTION ( 'NONE',  ( -0.3926557917762825700, 0.9196855055857631189, 5.808111630006007955E-09 ) ) ;
#19714 = EDGE_CURVE ( 'NONE', #39071, #45281, #39341, .T. ) ;
#19715 = EDGE_CURVE ( 'NONE', #16810, #1692, #44711, .T. ) ;
#19716 = CARTESIAN_POINT ( 'NONE',  ( -24.76540221579651302, -16.07765826482591365, 66.17829537637275905 ) ) ;
#19717 = VECTOR ( 'NONE', #20910, 1000.000000000000227 ) ;
#19718 = CARTESIAN_POINT ( 'NONE',  ( -16.53659385650551528, -6.915538690918075382, 49.31353937987644542 ) ) ;
#19719 = CARTESIAN_POINT ( 'NONE',  ( -17.57433505571471599, -21.80920136837260159, 58.59480362143565202 ) ) ;
#19720 = CARTESIAN_POINT ( 'NONE',  ( -22.21789835343034269, -9.106240630544798265, 59.89888112549417798 ) ) ;
#19721 = CARTESIAN_POINT ( 'NONE',  ( -13.42747132184446990, -8.521758955768165222, 57.13114303280060824 ) ) ;
#19722 = ORIENTED_EDGE ( 'NONE', *, *, #38747, .F. ) ;
#19723 = CARTESIAN_POINT ( 'NONE',  ( -24.47401588439613818, -14.84236418521736134, 59.54300237059216983 ) ) ;
#19724 = CARTESIAN_POINT ( 'NONE',  ( -16.28034385541300111, -9.360768649639558348, 51.01397948905896840 ) ) ;
#19725 = CYLINDRICAL_SURFACE ( 'NONE', #36086, 0.1500000000000000777 ) ;
#19726 = VECTOR ( 'NONE', #45751, 1000.000000000000227 ) ;
#19727 = FACE_OUTER_BOUND ( 'NONE', #4959, .T. ) ;
#19728 = ORIENTED_EDGE ( 'NONE', *, *, #9237, .F. ) ;
#19729 = ORIENTED_EDGE ( 'NONE', *, *, #30967, .T. ) ;
#19730 = B_SPLINE_CURVE_WITH_KNOTS ( 'NONE', 3,
 ( #42137, #8402, #32271, #21184, #39888, #28334, #31537, #39646, #6159, #1489 ),
 .UNSPECIFIED., .F., .F.,
 ( 4, 2, 2, 2, 4 ),
 ( 0.000000000000000000, 0.2500000000000000000, 0.5000000000000000000, 0.7500000000000000000, 1.000000000000000000 ),
 .UNSPECIFIED. ) ;
#19731 = AXIS2_PLACEMENT_3D ( 'NONE', #15143, #29453, #15380 ) ;
#19732 = CARTESIAN_POINT ( 'NONE',  ( -24.50086468078332658, -12.48019312587592999, 73.40372080011530898 ) ) ;
#19733 = VERTEX_POINT ( 'NONE', #20893 ) ;
#19734 = CARTESIAN_POINT ( 'NONE',  ( -24.02536259471169444, -17.13930990111214925, 73.16719446933997517 ) ) ;
#19735 = CARTESIAN_POINT ( 'NONE',  ( -23.42915847708036736, -11.11517115755410146, 73.64721174900437006 ) ) ;
#19736 = CYLINDRICAL_SURFACE ( 'NONE', #725, 1.999999999999999112 ) ;
#19737 = CARTESIAN_POINT ( 'NONE',  ( -24.74210650470650918, -16.20599442878457452, 62.71515881785720836 ) ) ;
#19738 = B_SPLINE_CURVE_WITH_KNOTS ( 'NONE', 3,
 ( #9560, #33993, #46009, #27771, #27529, #12263, #23606, #38611, #23849, #4893 ),
 .UNSPECIFIED., .F., .F.,
 ( 4, 2, 2, 2, 4 ),
 ( 0.1272669073658014571, 0.2522669073462826539, 0.3772669073267638229, 0.5022669073072449919, 0.6272669072877261609 ),
 .UNSPECIFIED. ) ;
#19739 = CARTESIAN_POINT ( 'NONE',  ( -14.16114181629738589, -8.110937519819053421, 67.37319822901852717 ) ) ;
#19740 = CARTESIAN_POINT ( 'NONE',  ( -11.29219319990544079, -18.28864530752396433, 57.82186711835544912 ) ) ;
#19741 = CIRCLE ( 'NONE', #44913, 1.249999999999999334 ) ;
#19742 = PLANE ( 'NONE',  #23225 ) ;
#19743 = ORIENTED_EDGE ( 'NONE', *, *, #45577, .F. ) ;
#19744 = PRODUCT_DEFINITION_SHAPE ( 'NONE', 'NONE',  #48742 ) ;
#19745 = CARTESIAN_POINT ( 'NONE',  ( -16.12858474313192048, -22.14570131352578741, 58.43585568879253600 ) ) ;
#19746 = EDGE_CURVE ( 'NONE', #30416, #28807, #5395, .T. ) ;
#19747 = LINE ( 'NONE', #15784, #10907 ) ;
#19748 = VECTOR ( 'NONE', #41179, 1000.000000000000000 ) ;
#19749 = CARTESIAN_POINT ( 'NONE',  ( -15.63656890543763112, -8.039962338392246721, 74.15155978326677655 ) ) ;
#19750 = CARTESIAN_POINT ( 'NONE',  ( -13.87409341786790762, -20.84236815287593103, 68.75625181053004553 ) ) ;
#19751 = CARTESIAN_POINT ( 'NONE',  ( -11.91470689456726717, -9.793200236000155101, 64.21569601040394559 ) ) ;
#19752 = CARTESIAN_POINT ( 'NONE',  ( -14.89095713150699218, -21.33490654319496116, 61.63600435359662555 ) ) ;
#19753 = ORIENTED_EDGE ( 'NONE', *, *, #14348, .T. ) ;
#19754 = VERTEX_POINT ( 'NONE', #32223 ) ;
#19755 = FACE_OUTER_BOUND ( 'NONE', #48494, .T. ) ;
#19756 = ORIENTED_EDGE ( 'NONE', *, *, #41804, .F. ) ;
#19757 = B_SPLINE_CURVE_WITH_KNOTS ( 'NONE', 3,
 ( #40059, #16667, #47207, #9787, #46727, #27761, #16425, #35858, #13200, #5364 ),
 .UNSPECIFIED., .F., .F.,
 ( 4, 2, 2, 2, 4 ),
 ( 0.6272669072877503638, 0.7522669073072690837, 0.8772669073267878037, 1.002266907346306635, 1.127266907365825244 ),
 .UNSPECIFIED. ) ;
#19758 = LINE ( 'NONE', #15793, #46878 ) ;
#19759 = VECTOR ( 'NONE', #31883, 1000.000000000000227 ) ;
#19760 = EDGE_CURVE ( 'NONE', #10364, #18524, #7901, .T. ) ;
#19761 = CARTESIAN_POINT ( 'NONE',  ( -24.07714866641017792, -12.63257625550829033, 69.99916305551172968 ) ) ;
#19762 =( BOUNDED_CURVE ( )  B_SPLINE_CURVE ( 2, ( #41889, #4451, #19466, #34479, #767, #15762, #30817, #19724, #31048 ),
 .UNSPECIFIED., .F., .F. ) 
 B_SPLINE_CURVE_WITH_KNOTS ( ( 3, 2, 2, 2, 3 ),
 ( 0.05901120358171226682, 0.05999458517735227481, 0.06097796677299228973, 0.06196134836863229772, 0.06294472996427230571 ),
 .UNSPECIFIED. ) 
 CURVE ( )  GEOMETRIC_REPRESENTATION_ITEM ( )  RATIONAL_B_SPLINE_CURVE ( ( 0.9999999999998986366, 0.9238795325113881018, 1.000000000000000000, 0.9238795325112867385, 1.000000000000000000, 0.9238795325112867385, 1.000000000000000000, 0.9238795325112381107, 1.000000000000048628 ) ) 
 REPRESENTATION_ITEM ( '' )  );
#19763 = ORIENTED_EDGE ( 'NONE', *, *, #4860, .T. ) ;
#19764 = CARTESIAN_POINT ( 'NONE',  ( -45.92409385541306222, -17.80920654474411435, 70.50000000000000000 ) ) ;
#19765 = VECTOR ( 'NONE', #23151, 1000.000000000000000 ) ;
#19766 = CARTESIAN_POINT ( 'NONE',  ( -13.73970969606274473, -20.76112332560825990, 65.28628881671112083 ) ) ;
#19767 = ORIENTED_EDGE ( 'NONE', *, *, #13951, .T. ) ;
#19768 = CARTESIAN_POINT ( 'NONE',  ( -10.46334769751556593, -14.06892751230320826, 57.63928137823284459 ) ) ;
#19769 = ORIENTED_EDGE ( 'NONE', *, *, #29798, .T. ) ;
#19770 = CARTESIAN_POINT ( 'NONE',  ( -11.34161041692636651, -11.34373020466420279, 64.16498710548324880 ) ) ;
#19771 = AXIS2_PLACEMENT_3D ( 'NONE', #36990, #29622, #30128 ) ;
#19772 = CARTESIAN_POINT ( 'NONE',  ( -12.26447506468708681, -20.18352723774274793, 65.00528407122952501 ) ) ;
#19773 = VERTEX_POINT ( 'NONE', #3380 ) ;
#19774 = CARTESIAN_POINT ( 'NONE',  ( -23.70015292207183322, -18.82353835121273988, 69.47867366044893345 ) ) ;
#19775 = CYLINDRICAL_SURFACE ( 'NONE', #3950, 0.5000000000000004441 ) ;
#19776 = DIRECTION ( 'NONE',  ( -3.071710424422018668E-17, 6.404604876783312462E-16, 1.000000000000000000 ) ) ;
#19777 = ORIENTED_EDGE ( 'NONE', *, *, #36660, .F. ) ;
#19778 = CARTESIAN_POINT ( 'NONE',  ( -19.66015618626893868, -21.44380804025676923, 69.16312308005014131 ) ) ;
#19779 = EDGE_CURVE ( 'NONE', #467, #38954, #10537, .T. ) ;
#19780 = CARTESIAN_POINT ( 'NONE',  ( -24.12071557656922494, -11.54438865435207795, 63.06722852297808402 ) ) ;
#19781 = AXIS2_PLACEMENT_3D ( 'NONE', #30420, #19075, #373 ) ;
#19782 = CARTESIAN_POINT ( 'NONE',  ( -11.58645319427940024, -10.18053053143523279, 71.06918860465941634 ) ) ;
#19783 = CARTESIAN_POINT ( 'NONE',  ( -24.47354813883760016, -12.39902559715248032, 73.42720875634239519 ) ) ;
#19784 = CARTESIAN_POINT ( 'NONE',  ( -17.94839601134439633, -19.47832453368858197, 52.02966884056656482 ) ) ;
#19785 = DIRECTION ( 'NONE',  ( 0.3667195576449454042, -0.9303315355510073381, -1.591455084066186922E-08 ) ) ;
#19786 = DIRECTION ( 'NONE',  ( 0.000000000000000000, 0.000000000000000000, 1.000000000000000000 ) ) ;
#19787 = CARTESIAN_POINT ( 'NONE',  ( -17.82203991332369597, -7.766729491495081739, 63.85057028805255186 ) ) ;
#19788 = EDGE_CURVE ( 'NONE', #37220, #30787, #6435, .T. ) ;
#19789 = ADVANCED_FACE ( 'NONE', ( #36847 ), #17431, .T. ) ;
#19790 = CARTESIAN_POINT ( 'NONE',  ( -10.47679702054951534, -15.67959025947600971, 64.69698733612924002 ) ) ;
#19791 = CARTESIAN_POINT ( 'NONE',  ( -15.21159385650551776, -6.922745924619793101, 51.69366785382590024 ) ) ;
#19792 = AXIS2_PLACEMENT_3D ( 'NONE', #42054, #45993, #19397 ) ;
#19794 = EDGE_CURVE ( 'NONE', #42912, #12909, #18144, .T. ) ;
#19793 = ORIENTED_EDGE ( 'NONE', *, *, #27405, .F. ) ;
#19795 = CYLINDRICAL_SURFACE ( 'NONE', #13310, 0.1499999999999963585 ) ;
#19796 = CARTESIAN_POINT ( 'NONE',  ( -24.28330220718811105, -16.20608195347976022, 59.31435516383907469 ) ) ;
#19797 = ORIENTED_EDGE ( 'NONE', *, *, #26740, .T. ) ;
#19798 = CARTESIAN_POINT ( 'NONE',  ( -21.39967327233876659, -20.63170314183283693, 72.80974286114339122 ) ) ;
#19799 = EDGE_CURVE ( 'NONE', #41453, #47915, #6600, .T. ) ;
#19800 = CARTESIAN_POINT ( 'NONE',  ( -23.26656235495780578, -10.18637482697468677, 63.21152651401433786 ) ) ;
#19801 = LINE ( 'NONE', #19299, #46276 ) ;
#19802 = ORIENTED_EDGE ( 'NONE', *, *, #27758, .F. ) ;
#19803 = CARTESIAN_POINT ( 'NONE',  ( -24.40557713429137365, -14.30039287845891671, 66.29178820325090271 ) ) ;
#19804 = CARTESIAN_POINT ( 'NONE',  ( -17.24553756445192221, -7.761319519027048308, 70.49595599234443455 ) ) ;
#19805 = CIRCLE ( 'NONE', #38657, 1.999999999999999556 ) ;
#19806 = CARTESIAN_POINT ( 'NONE',  ( -12.00971629994662493, -9.691756596678954949, 60.67422760384662439 ) ) ;
#19807 = EDGE_CURVE ( 'NONE', #43020, #45257, #26044, .T. ) ;
#19808 = ORIENTED_EDGE ( 'NONE', *, *, #21495, .F. ) ;
#19809 = CARTESIAN_POINT ( 'NONE',  ( -11.35719102664687874, -18.40077844947705188, 58.09242476654641507 ) ) ;
#19810 = AXIS2_PLACEMENT_3D ( 'NONE', #17817, #25239, #32143 ) ;
#19811 = FACE_OUTER_BOUND ( 'NONE', #32900, .T. ) ;
#19812 = CARTESIAN_POINT ( 'NONE',  ( -10.42930205768512941, -13.90492575851057211, 61.33310083575204885 ) ) ;
#19813 =( BOUNDED_CURVE ( )  B_SPLINE_CURVE ( 3, ( #5886, #25556, #2430, #28773 ),
 .UNSPECIFIED., .F., .F. ) 
 B_SPLINE_CURVE_WITH_KNOTS ( ( 4, 4 ),
 ( 0.9074455897393592929, 1.000000000000000000 ),
 .UNSPECIFIED. ) 
 CURVE ( )  GEOMETRIC_REPRESENTATION_ITEM ( )  RATIONAL_B_SPLINE_CURVE ( ( 0.6983129098260664191, 0.7760317562606752206, 0.8765941196519864143, 1.000000000000000000 ) ) 
 REPRESENTATION_ITEM ( '' )  );
#19814 = FACE_OUTER_BOUND ( 'NONE', #10652, .T. ) ;
#19815 = DIRECTION ( 'NONE',  ( 0.000000000000000000, 1.000000000000000000, 0.000000000000000000 ) ) ;
#19816 = ORIENTED_EDGE ( 'NONE', *, *, #6785, .F. ) ;
#19817 = ORIENTED_EDGE ( 'NONE', *, *, #24304, .F. ) ;
#19818 = CARTESIAN_POINT ( 'NONE',  ( -20.89284385541304445, -8.630756214087126565, 51.74842643355248129 ) ) ;
#19819 = CARTESIAN_POINT ( 'NONE',  ( -10.72552571836178181, -12.61109718544098790, 60.79853568372240602 ) ) ;
#19820 = LINE ( 'NONE', #22526, #37039 ) ;
#19821 = VECTOR ( 'NONE', #47615, 1000.000000000000000 ) ;
#19822 =( BOUNDED_SURFACE ( )  B_SPLINE_SURFACE ( 3, 1, ( 
 ( #21723, #17539 ),
 ( #32565, #8180 ),
 ( #7208, #37202 ),
 ( #782, #12104 ),
 ( #30834, #34496 ),
 ( #11866, #41404 ),
 ( #11370, #7696 ) ),
 .UNSPECIFIED., .T., .F., .F. ) 
 B_SPLINE_SURFACE_WITH_KNOTS ( ( 4, 3, 4 ),
 ( 2, 2 ),
 ( 0.000000000000000000, 0.5000000000000000000, 1.000000000000000000 ),
 ( 0.000000000000000000, 1.000000000000000000 ),
 .UNSPECIFIED. ) 
 GEOMETRIC_REPRESENTATION_ITEM ( )  RATIONAL_B_SPLINE_SURFACE ( (
 ( 1.000000000000000000, 1.000000000000000000),
 ( 0.3333333333333335369, 0.3333333333333330373),
 ( 0.3333333333333335369, 0.3333333333333330373),
 ( 1.000000000000000000, 1.000000000000000000),
 ( 0.3333333333333333703, 0.3333333333333333703),
 ( 0.3333333333333333703, 0.3333333333333333703),
 ( 1.000000000000000000, 1.000000000000000000) ) ) 
 REPRESENTATION_ITEM ( '' )  SURFACE ( )  );
#19823 = CARTESIAN_POINT ( 'NONE',  ( -17.79108452803360763, -21.84994637594637723, 58.69081321602850920 ) ) ;
#19824 = CARTESIAN_POINT ( 'NONE',  ( -20.66848101912799862, -8.549761622307151754, 60.12653141481577990 ) ) ;
#19825 = CARTESIAN_POINT ( 'NONE',  ( -10.41631042766677417, -15.61196327047340304, 64.59951812971527829 ) ) ;
#19826 = CARTESIAN_POINT ( 'NONE',  ( -18.12273512012592747, -22.22646200727865917, 65.46036854067777710 ) ) ;
#19827 = ADVANCED_FACE ( 'NONE', ( #40557 ), #17893, .T. ) ;
#19828 = ORIENTED_EDGE ( 'NONE', *, *, #7889, .T. ) ;
#19829 = CARTESIAN_POINT ( 'NONE',  ( -21.31800492490012999, -20.62620369199774117, 72.52446429884872714 ) ) ;
#19830 = CARTESIAN_POINT ( 'NONE',  ( -10.09291391017891115, -16.13494330055838333, 68.16263215882007387 ) ) ;
#19831 = VERTEX_POINT ( 'NONE', #44516 ) ;
#19832 = DIRECTION ( 'NONE',  ( -0.000000000000000000, -1.000000000000000000, -0.000000000000000000 ) ) ;
#19833 = CARTESIAN_POINT ( 'NONE',  ( -17.81160558974999830, -14.71003671187606088, 53.27966884056655061 ) ) ;
#19834 = ORIENTED_EDGE ( 'NONE', *, *, #18209, .T. ) ;
#19835 = LINE ( 'NONE', #4095, #38758 ) ;
#19836 = EDGE_CURVE ( 'NONE', #44310, #40803, #39308, .T. ) ;
#19837 = TOROIDAL_SURFACE ( 'NONE', #30853, 1.750000000000000000, 0.2500000000000000000 ) ;
#19838 = CYLINDRICAL_SURFACE ( 'NONE', #48507, 0.1500000000000022427 ) ;
#19839 = CARTESIAN_POINT ( 'NONE',  ( -20.03442169439229303, -8.314116961584396392, 70.35986449788516950 ) ) ;
#19840 = LINE ( 'NONE', #12197, #18967 ) ;
#19841 = ORIENTED_EDGE ( 'NONE', *, *, #17731, .F. ) ;
#19842 = CARTESIAN_POINT ( 'NONE',  ( -13.83108299072750391, -21.33561835983412891, 72.04112301026525245 ) ) ;
#19843 = CARTESIAN_POINT ( 'NONE',  ( -17.79355539233428374, -22.25020845511654954, 58.56586767823151263 ) ) ;
#19844 = LINE ( 'NONE', #45942, #36413 ) ;
#19845 = FACE_BOUND ( 'NONE', #8247, .T. ) ;
#19846 = SHAPE_DEFINITION_REPRESENTATION ( #26805, #2768 ) ;
#19847 = DIRECTION ( 'NONE',  ( -1.000000000000000000, 0.000000000000000000, -2.181982678098338148E-16 ) ) ;
#19848 = CARTESIAN_POINT ( 'NONE',  ( -23.42915847708036736, -11.11517115755410146, 73.64721174900437006 ) ) ;
#19849 = ADVANCED_FACE ( 'NONE', ( #2657 ), #28999, .T. ) ;
#19850 = DIRECTION ( 'NONE',  ( -0.2189141945955538626, 0.9757441136919966507, 0.000000000000000000 ) ) ;
#19851 = VERTEX_POINT ( 'NONE', #25792 ) ;
#19852 = CARTESIAN_POINT ( 'NONE',  ( -13.75179125342063458, -11.87837916245159775, 52.02966884056656482 ) ) ;
#19853 = EDGE_CURVE ( 'NONE', #26529, #40716, #34583, .T. ) ;
#19854 = EDGE_LOOP ( 'NONE', ( #41348, #35706, #18001, #36162, #14955, #40301, #27692, #1102 ) ) ;
#19855 = CARTESIAN_POINT ( 'NONE',  ( -27.42409385541305511, -25.10920654474410441, 48.99999999999997868 ) ) ;
#19856 = CARTESIAN_POINT ( 'NONE',  ( -20.64377408635552769, -21.08512125173600893, 62.20651549696969340 ) ) ;
#19857 = ORIENTED_EDGE ( 'NONE', *, *, #23751, .T. ) ;
#19858 = CARTESIAN_POINT ( 'NONE',  ( -23.71751471349159601, -11.63122711669449494, 63.23746208799618529 ) ) ;
#19859 = FACE_BOUND ( 'NONE', #14774, .T. ) ;
#19860 = ORIENTED_EDGE ( 'NONE', *, *, #10359, .F. ) ;
#19861 = ORIENTED_EDGE ( 'NONE', *, *, #10356, .F. ) ;
#19862 = ORIENTED_EDGE ( 'NONE', *, *, #8873, .T. ) ;
#19863 = DIRECTION ( 'NONE',  ( -0.9796876409582463419, 0.2005296141562636081, 7.890952370353029293E-08 ) ) ;
#19864 = CARTESIAN_POINT ( 'NONE',  ( -19.45281838860202228, -9.697037067072804106, 53.49899999999994549 ) ) ;
#19866 = EDGE_CURVE ( 'NONE', #2243, #10578, #9481, .T. ) ;
#19865 = CARTESIAN_POINT ( 'NONE',  ( -16.38321341446914658, -21.78497919871296062, 65.64053219190310529 ) ) ;
#19867 = CARTESIAN_POINT ( 'NONE',  ( -14.58386023763418926, -8.409552415680012771, 67.37048090121328414 ) ) ;
#19868 = CARTESIAN_POINT ( 'NONE',  ( -10.76270079184834749, -12.47665168726528506, 64.41269048358307714 ) ) ;
#19869 = CARTESIAN_POINT ( 'NONE',  ( -12.56172001024846452, -20.45377019276184427, 71.99149100736865137 ) ) ;
#19870 = ORIENTED_EDGE ( 'NONE', *, *, #15478, .T. ) ;
#19871 = EDGE_LOOP ( 'NONE', ( #17682, #21813, #16185, #7179, #16965 ) ) ;
#19872 = B_SPLINE_CURVE_WITH_KNOTS ( 'NONE', 3,
 ( #20903, #32473, #13727, #44296, #39612, #10063, #14436, #25557, #25086, #44062 ),
 .UNSPECIFIED., .F., .F.,
 ( 4, 2, 2, 2, 4 ),
 ( 0.1272669073658340144, 0.2522669073463233991, 0.3772669073268128392, 0.5022669073073022794, 0.6272669072877916641 ),
 .UNSPECIFIED. ) ;
#19873 = CARTESIAN_POINT ( 'NONE',  ( -21.48659385650551457, -9.302874398569244363, 51.68646062012417985 ) ) ;
#19874 = DIRECTION ( 'NONE',  ( -0.9990515194385544140, -0.04354378839186318073, 1.103613758316041049E-08 ) ) ;
#19875 = CARTESIAN_POINT ( 'NONE',  ( -21.05884094699671039, -21.31242506687340210, 62.22133086525234091 ) ) ;
#19876 = CARTESIAN_POINT ( 'NONE',  ( -19.72874733844480488, -21.41900457955616588, 65.69159546287741591 ) ) ;
#19877 = ORIENTED_EDGE ( 'NONE', *, *, #17680, .T. ) ;
#19878 = CARTESIAN_POINT ( 'NONE',  ( -13.07409385650551847, -9.792211528768506312, 50.49490371617623197 ) ) ;
#19879 = VERTEX_POINT ( 'NONE', #44285 ) ;
#19880 = CARTESIAN_POINT ( 'NONE',  ( -12.10599122619147749, -20.02663529450013513, 61.58173959111590534 ) ) ;
#19881 = CARTESIAN_POINT ( 'NONE',  ( -17.24727489946581116, -7.811440102727049251, 67.21142879207842213 ) ) ;
#19882 = EDGE_CURVE ( 'NONE', #32982, #15059, #25545, .T. ) ;
#19883 = VERTEX_POINT ( 'NONE', #18389 ) ;
#19884 = DIRECTION ( 'NONE',  ( -3.071710424422018668E-17, 6.404604876783312462E-16, 1.000000000000000000 ) ) ;
#19885 = CARTESIAN_POINT ( 'NONE',  ( -21.13745558015973103, -11.09794736473739896, 49.52966884056655772 ) ) ;
#19886 = CARTESIAN_POINT ( 'NONE',  ( -17.42409385541305511, -14.80920654474410725, 48.99999999999997868 ) ) ;
#19887 = ORIENTED_EDGE ( 'NONE', *, *, #13952, .T. ) ;
#19888 = CARTESIAN_POINT ( 'NONE',  ( -10.44551245922705185, -15.36195639909390742, 57.85176246259045740 ) ) ;
#19889 = LINE ( 'NONE', #34893, #20487 ) ;
#19890 = CARTESIAN_POINT ( 'NONE',  ( -12.41578987685235980, -20.32480987677443807, 68.47510952779386173 ) ) ;
#19891 = ORIENTED_EDGE ( 'NONE', *, *, #1705, .F. ) ;
#19892 = EDGE_LOOP ( 'NONE', ( #40313, #34996 ) ) ;
#19893 = CARTESIAN_POINT ( 'NONE',  ( -15.41198273355754900, -21.57429164360176799, 65.26163917071316689 ) ) ;
#19894 = CARTESIAN_POINT ( 'NONE',  ( -14.86627003481517839, -7.811970263561289762, 56.96504677300865893 ) ) ;
#19895 = ORIENTED_EDGE ( 'NONE', *, *, #22750, .F. ) ;
#19896 = CARTESIAN_POINT ( 'NONE',  ( -13.33011785382929304, -9.069340661520646663, 63.92418669539090814 ) ) ;
#19897 = CARTESIAN_POINT ( 'NONE',  ( -23.78500266573477262, -11.88707733699690827, 59.78235732566622573 ) ) ;
#19898 = CARTESIAN_POINT ( 'NONE',  ( -14.24557640779922352, -8.071278081433945317, 67.35951463815518991 ) ) ;
#19899 = EDGE_CURVE ( 'NONE', #3049, #31720, #26157, .T. ) ;
#19900 = CARTESIAN_POINT ( 'NONE',  ( -14.25068826455714621, -8.513811653308138716, 70.87957628655816222 ) ) ;
#19901 = VERTEX_POINT ( 'NONE', #8080 ) ;
#19902 = CARTESIAN_POINT ( 'NONE',  ( -9.995738443926455830, -14.24059931954510816, 64.50308448303212572 ) ) ;
#19903 = PRODUCT_DEFINITION_CONTEXT ( 'detailed design', #28121, 'design' ) ;
#19904 = EDGE_CURVE ( 'NONE', #27633, #2092, #48144, .T. ) ;
#19905 = CARTESIAN_POINT ( 'NONE',  ( -20.59780922738080378, -8.569522135318988987, 63.32738143816840903 ) ) ;
#19906 = DIRECTION ( 'NONE',  ( -3.071710424422018668E-17, 6.404604876783312462E-16, 1.000000000000000000 ) ) ;
#19907 = CARTESIAN_POINT ( 'NONE',  ( -23.46293004877725252, -19.17220411032675997, 62.54681013563286029 ) ) ;
#19908 = ORIENTED_EDGE ( 'NONE', *, *, #41539, .F. ) ;
#19909 = CARTESIAN_POINT ( 'NONE',  ( -23.96075626263749214, -17.45014286185010377, 66.24357239682278475 ) ) ;
#19910 = ADVANCED_FACE ( 'NONE', ( #23319 ), #29986, .F. ) ;
#19911 = CARTESIAN_POINT ( 'NONE',  ( -21.47456293661849713, -9.038556783377254433, 70.41660404402310292 ) ) ;
#19912 = ORIENTED_EDGE ( 'NONE', *, *, #813, .T. ) ;
#19913 = ORIENTED_EDGE ( 'NONE', *, *, #4529, .F. ) ;
#19914 = CARTESIAN_POINT ( 'NONE',  ( -21.73853604213786639, -16.63919858500264937, 49.52966884056655772 ) ) ;
#19915 = CARTESIAN_POINT ( 'NONE',  ( -10.18364478422453345, -13.05433800282328960, 71.46474530336836040 ) ) ;
#19916 = B_SPLINE_CURVE_WITH_KNOTS ( 'NONE', 3,
 ( #36275, #16340, #46407, #31629, #12661, #2065, #46655, #5283, #1826, #16825 ),
 .UNSPECIFIED., .F., .F.,
 ( 4, 2, 2, 2, 4 ),
 ( 0.1272669073658204419, 0.2522669073439322562, 0.3772669073220440428, 0.5022669073001558848, 0.6272669072782677269 ),
 .UNSPECIFIED. ) ;
#19917 = EDGE_CURVE ( 'NONE', #4870, #18548, #23447, .T. ) ;
#19918 = CARTESIAN_POINT ( 'NONE',  ( -22.91784385650551670, -9.790100578890868377, 49.79778022625162492 ) ) ;
#19919 = CARTESIAN_POINT ( 'NONE',  ( -11.64235137327199610, -18.84330536064715034, 68.36689631560025759 ) ) ;
#19920 = CARTESIAN_POINT ( 'NONE',  ( -12.26902398874117495, -19.54473763108856943, 58.22682373989366766 ) ) ;
#19921 = CARTESIAN_POINT ( 'NONE',  ( -19.78100189160110389, -21.87668917967754112, 65.58673452452636354 ) ) ;
#19922 = FACE_OUTER_BOUND ( 'NONE', #11427, .T. ) ;
#19923 = VERTEX_POINT ( 'NONE', #37846 ) ;
#19924 = ORIENTED_EDGE ( 'NONE', *, *, #28360, .T. ) ;
#19925 = CARTESIAN_POINT ( 'NONE',  ( -11.02242957576233273, -11.85532881267382166, 74.57312195644870201 ) ) ;
#19926 = VECTOR ( 'NONE', #18523, 1000.000000000000000 ) ;
#19927 = DIRECTION ( 'NONE',  ( -3.413470714839332458E-33, 1.190614954331866791E-16, -1.000000000000000000 ) ) ;
#19928 = DIRECTION ( 'NONE',  ( -0.3566357048164924270, 0.9342435303763380050, -8.054691247152028744E-09 ) ) ;
#19929 = CYLINDRICAL_SURFACE ( 'NONE', #4017, 0.1500000000000004385 ) ;
#19930 = ADVANCED_FACE ( 'NONE', ( #38081 ), #2833, .T. ) ;
#19931 = EDGE_CURVE ( 'NONE', #11159, #6741, #21283, .T. ) ;
#19932 = ORIENTED_EDGE ( 'NONE', *, *, #25791, .F. ) ;
#19933 = DIRECTION ( 'NONE',  ( -3.071710424422018668E-17, 6.404604876783312462E-16, 1.000000000000000000 ) ) ;
#19934 = CARTESIAN_POINT ( 'NONE',  ( -23.35641471936834535, -10.99444570894131168, 73.24704464419542660 ) ) ;
#19935 = CARTESIAN_POINT ( 'NONE',  ( -15.62847675160137406, -21.57498509099777095, 72.15461454263183327 ) ) ;
#19936 = DIRECTION ( 'NONE',  ( -3.071710424422018668E-17, 6.404604876783312462E-16, 1.000000000000000000 ) ) ;
#19937 =( BOUNDED_SURFACE ( )  B_SPLINE_SURFACE ( 3, 1, ( 
 ( #20140, #31466 ),
 ( #28742, #21600 ),
 ( #3113, #32671 ),
 ( #2145, #18120 ),
 ( #10519, #14407 ),
 ( #13931, #17872 ),
 ( #10748, #6335 ) ),
 .UNSPECIFIED., .T., .F., .F. ) 
 B_SPLINE_SURFACE_WITH_KNOTS ( ( 4, 3, 4 ),
 ( 2, 2 ),
 ( 0.000000000000000000, 0.5000000000000000000, 1.000000000000000000 ),
 ( 0.000000000000000000, 1.000000000000000000 ),
 .UNSPECIFIED. ) 
 GEOMETRIC_REPRESENTATION_ITEM ( )  RATIONAL_B_SPLINE_SURFACE ( (
 ( 1.000000000000000000, 1.000000000000000000),
 ( 0.3333333333333335369, 0.3333333333333330373),
 ( 0.3333333333333335369, 0.3333333333333330373),
 ( 1.000000000000000000, 1.000000000000000000),
 ( 0.3333333333333333703, 0.3333333333333333703),
 ( 0.3333333333333333703, 0.3333333333333333703),
 ( 1.000000000000000000, 1.000000000000000000) ) ) 
 REPRESENTATION_ITEM ( '' )  SURFACE ( )  );
#19938 = EDGE_CURVE ( 'NONE', #42817, #18995, #31638, .T. ) ;
#19939 = EDGE_LOOP ( 'NONE', ( #31924, #25816, #7614, #11382 ) ) ;
#19940 = CARTESIAN_POINT ( 'NONE',  ( -24.85911909788007179, -14.32540520456757172, 69.83930567627945152 ) ) ;
#19941 = CARTESIAN_POINT ( 'NONE',  ( -22.11774618123879677, -15.02177039319221308, 49.52966884056655772 ) ) ;
#19942 = ORIENTED_EDGE ( 'NONE', *, *, #6264, .T. ) ;
#19943 = CARTESIAN_POINT ( 'NONE',  ( -11.28158159523816728, -11.33292898549803240, 57.36470039992773451 ) ) ;
#19944 = CARTESIAN_POINT ( 'NONE',  ( -10.42462062702805703, -14.89507852762941198, 74.79778901763455679 ) ) ;
#19945 =( BOUNDED_CURVE ( )  B_SPLINE_CURVE ( 3, ( #44214, #27530, #35811, #10222 ),
 .UNSPECIFIED., .F., .F. ) 
 B_SPLINE_CURVE_WITH_KNOTS ( ( 4, 4 ),
 ( 0.5000000000000000000, 0.9074455897393709503 ),
 .UNSPECIFIED. ) 
 CURVE ( )  GEOMETRIC_REPRESENTATION_ITEM ( )  RATIONAL_B_SPLINE_CURVE ( ( 1.000000000000007327, 0.4567392136813255288, 0.3561768502900227173, 0.6983129098261068313 ) ) 
 REPRESENTATION_ITEM ( '' )  );
#19946 = ORIENTED_EDGE ( 'NONE', *, *, #30019, .F. ) ;
#19947 =( BOUNDED_CURVE ( )  B_SPLINE_CURVE ( 3, ( #26856, #18464, #41871, #3706 ),
 .UNSPECIFIED., .F., .F. ) 
 B_SPLINE_CURVE_WITH_KNOTS ( ( 4, 4 ),
 ( 0.000000000000000000, 0.4074455897393629566 ),
 .UNSPECIFIED. ) 
 CURVE ( )  GEOMETRIC_REPRESENTATION_ITEM ( )  RATIONAL_B_SPLINE_CURVE ( ( 1.000000000000000000, 0.4567392136813387959, 0.3561768502900328204, 0.6983129098260820733 ) ) 
 REPRESENTATION_ITEM ( '' )  );
#19948 = DIRECTION ( 'NONE',  ( -3.071710424422018668E-17, 6.404604876783312462E-16, 1.000000000000000000 ) ) ;
#19949 = ORIENTED_EDGE ( 'NONE', *, *, #11598, .F. ) ;
#19950 = CARTESIAN_POINT ( 'NONE',  ( -17.22281210278579167, -7.361840297529252730, 70.60540404266352255 ) ) ;
#19951 = CARTESIAN_POINT ( 'NONE',  ( -21.31115985637654120, -8.927249709250721921, 73.88656608925673197 ) ) ;
#19952 = EDGE_LOOP ( 'NONE', ( #42612, #47325, #42126, #31995 ) ) ;
#19953 = LINE ( 'NONE', #17626, #40369 ) ;
#19954 = FACE_OUTER_BOUND ( 'NONE', #8781, .T. ) ;
#19955 = AXIS2_PLACEMENT_3D ( 'NONE', #45824, #12080, #29824 ) ;
#19956 = CARTESIAN_POINT ( 'NONE',  ( -16.81784385650551528, -9.790100578890868377, 49.79778022625163203 ) ) ;
#19957 = CARTESIAN_POINT ( 'NONE',  ( -17.78823904182716120, -7.818684512505932993, 60.38060768393231825 ) ) ;
#19958 = FACE_OUTER_BOUND ( 'NONE', #30836, .T. ) ;
#19959 = ORIENTED_EDGE ( 'NONE', *, *, #12679, .T. ) ;
#19960 = DIRECTION ( 'NONE',  ( -3.071710424422018668E-17, 6.404604876783312462E-16, 1.000000000000000000 ) ) ;
#19961 =( BOUNDED_CURVE ( )  B_SPLINE_CURVE ( 3, ( #18353, #29695, #23054, #7546 ),
 .UNSPECIFIED., .F., .F. ) 
 B_SPLINE_CURVE_WITH_KNOTS ( ( 4, 4 ),
 ( 0.4074455897393651771, 0.5000000000000000000 ),
 .UNSPECIFIED. ) 
 CURVE ( )  GEOMETRIC_REPRESENTATION_ITEM ( )  RATIONAL_B_SPLINE_CURVE ( ( 0.6983129098260844048, 0.7760317562606871000, 0.8765941196519911882, 0.9999999999999941158 ) ) 
 REPRESENTATION_ITEM ( '' )  );
#19962 = CARTESIAN_POINT ( 'NONE',  ( -30.42409385541305156, -6.359206544744109735, 47.99999999999997868 ) ) ;
#19963 = CYLINDRICAL_SURFACE ( 'NONE', #20302, 5.249999999999998224 ) ;
#19964 = EDGE_CURVE ( 'NONE', #30264, #47790, #32747, .T. ) ;
#19965 = CARTESIAN_POINT ( 'NONE',  ( -23.68074301380292823, -18.85356566062577599, 69.44371981100314883 ) ) ;
#19966 = FACE_OUTER_BOUND ( 'NONE', #28352, .T. ) ;
#19967 = ORIENTED_EDGE ( 'NONE', *, *, #46588, .T. ) ;
#19968 = ORIENTED_EDGE ( 'NONE', *, *, #26539, .F. ) ;
#19969 = EDGE_CURVE ( 'NONE', #24011, #15202, #8544, .T. ) ;
#19970 = CARTESIAN_POINT ( 'NONE',  ( -21.44791825677726038, -9.079743230750363381, 73.82958728338842036 ) ) ;
#19971 = CARTESIAN_POINT ( 'NONE',  ( -14.59672178607931414, -8.347720424474937673, 60.20507679337548979 ) ) ;
#19972 = VERTEX_POINT ( 'NONE', #12717 ) ;
#19973 = CARTESIAN_POINT ( 'NONE',  ( -22.53655392111809164, -20.22829597721307948, 65.88917050827579658 ) ) ;
#19974 = CARTESIAN_POINT ( 'NONE',  ( -15.60243201887541709, -21.62804181911354817, 68.73160055118694345 ) ) ;
#19975 = CARTESIAN_POINT ( 'NONE',  ( -22.16159385759798894, -7.228003583438117552, 51.38655588711986155 ) ) ;
#19976 = CARTESIAN_POINT ( 'NONE',  ( -13.08297840233603182, -8.754478813416307403, 64.04913201435263659 ) ) ;
#19977 = CARTESIAN_POINT ( 'NONE',  ( -10.66331429883175019, -17.94058386735023802, 71.68062945273115361 ) ) ;
#19978 = LINE ( 'NONE', #8661, #12905 ) ;
#19979 = ORIENTED_EDGE ( 'NONE', *, *, #16105, .T. ) ;
#19980 = CARTESIAN_POINT ( 'NONE',  ( -22.64922984081423252, -10.07076843310239589, 66.54182118905438870 ) ) ;
#19981 = CYLINDRICAL_SURFACE ( 'NONE', #5399, 5.249999999999998224 ) ;
#19982 = CARTESIAN_POINT ( 'NONE',  ( -23.21383278545907558, -10.12064720979650190, 63.11540053722242050 ) ) ;
#19983 = CARTESIAN_POINT ( 'NONE',  ( -17.67039274234547364, -7.813102812368692085, 63.83440432737404535 ) ) ;
#19984 = CARTESIAN_POINT ( 'NONE',  ( -21.49816216734858898, -9.116934002111024782, 70.13132539266752019 ) ) ;
#19985 = EDGE_CURVE ( 'NONE', #20224, #6783, #14136, .T. ) ;
#19987 = VERTEX_POINT ( 'NONE', #27971 ) ;
#19986 = ADVANCED_FACE ( 'NONE', ( #5337 ), #27729, .T. ) ;
#19988 = ORIENTED_EDGE ( 'NONE', *, *, #2970, .T. ) ;
#19989 = CIRCLE ( 'NONE', #15243, 4.686499999999999666 ) ;
#19990 = CARTESIAN_POINT ( 'NONE',  ( -22.58034385650552167, -6.424090610841174609, 49.80797279389977916 ) ) ;
#19991 = B_SPLINE_CURVE_WITH_KNOTS ( 'NONE', 1,
 ( #1301, #30461 ),
 .UNSPECIFIED., .F., .F.,
 ( 2, 2 ),
 ( 0.000000000000000000, 1.000000000000000000 ),
 .UNSPECIFIED. ) ;
#19992 = ORIENTED_EDGE ( 'NONE', *, *, #34287, .T. ) ;
#19993 = EDGE_CURVE ( 'NONE', #41987, #37795, #39049, .T. ) ;
#19994 = ADVANCED_FACE ( 'NONE', ( #46699 ), #46931, .T. ) ;
#19995 = EDGE_CURVE ( 'NONE', #44029, #34579, #4601, .T. ) ;
#19996 = DIRECTION ( 'NONE',  ( 0.7800143876985550229, -0.6257615799833393666, 5.505484597913564244E-08 ) ) ;
#19997 = CIRCLE ( 'NONE', #28642, 2.000000000000000444 ) ;
#19998 = CARTESIAN_POINT ( 'NONE',  ( -10.96452110319877704, -18.52097308172938739, 57.91440450685169594 ) ) ;
#19999 = ORIENTED_EDGE ( 'NONE', *, *, #47720, .T. ) ;
#20000 = CARTESIAN_POINT ( 'NONE',  ( -10.43073328261085386, -14.50439875238632403, 67.85800126138448718 ) ) ;
#20001 = CARTESIAN_POINT ( 'NONE',  ( -10.89280251029460622, -11.22507333849785027, 64.33377325762776877 ) ) ;
#20002 = ORIENTED_EDGE ( 'NONE', *, *, #2986, .T. ) ;
#20003 = CARTESIAN_POINT ( 'NONE',  ( -18.05440415122280839, -21.83127237841607027, 65.36004252941745563 ) ) ;
#20004 = CARTESIAN_POINT ( 'NONE',  ( -41.53953503188365204, -14.90920654474424367, 70.07647058823528141 ) ) ;
#20005 = ORIENTED_EDGE ( 'NONE', *, *, #11737, .F. ) ;
#20006 = CARTESIAN_POINT ( 'NONE',  ( -19.48731947536727915, -21.55887828695198039, 69.07915298548451233 ) ) ;
#20007 = CARTESIAN_POINT ( 'NONE',  ( -13.53325622885376944, -21.16256470055228789, 65.17124264509627096 ) ) ;
#20008 = ORIENTED_EDGE ( 'NONE', *, *, #44427, .T. ) ;
#20009 = CARTESIAN_POINT ( 'NONE',  ( -23.42626641412206823, -19.22254892098468204, 62.61052823878424078 ) ) ;
#20010 = CARTESIAN_POINT ( 'NONE',  ( -22.22619444978876757, -20.50513558618911958, 58.94938304221643222 ) ) ;
#20011 = CARTESIAN_POINT ( 'NONE',  ( -14.21171452256333012, -10.65672306833167760, 52.02966884056656482 ) ) ;
#20012 = EDGE_LOOP ( 'NONE', ( #229, #3806, #5993, #17627 ) ) ;
#20013 = CARTESIAN_POINT ( 'NONE',  ( -13.54792730259346456, -8.920061342218058797, 57.25495614889487683 ) ) ;
#20014 = EDGE_CURVE ( 'NONE', #15909, #18272, #17921, .T. ) ;
#20015 = CARTESIAN_POINT ( 'NONE',  ( -22.11764131551248269, -20.59576654024708731, 58.95098234965121264 ) ) ;
#20016 = DIRECTION ( 'NONE',  ( -5.731567514496413899E-31, -1.020425574103664789E-16, -1.000000000000000000 ) ) ;
#20017 = CARTESIAN_POINT ( 'NONE',  ( -10.82908108634309663, -17.30933488606310178, 68.51210539238705621 ) ) ;
#20018 = CARTESIAN_POINT ( 'NONE',  ( -12.79725860806972904, -20.12850118792689358, 71.95653676770096752 ) ) ;
#20019 = PLANE ( 'NONE',  #47513 ) ;
#20020 = PLANE ( 'NONE',  #36022 ) ;
#20021 = DIRECTION ( 'NONE',  ( -2.866981220435666553E-17, 1.000000000000000000, 1.190614954331866791E-16 ) ) ;
#20022 = VECTOR ( 'NONE', #24598, 999.9999999999998863 ) ;
#20023 = CARTESIAN_POINT ( 'NONE',  ( -21.35673258969864818, -10.96416394607318878, 53.49999999999995026 ) ) ;
#20024 = CARTESIAN_POINT ( 'NONE',  ( -17.06784385650551528, -6.428312510596451368, 51.20221977374900035 ) ) ;
#20025 = VERTEX_POINT ( 'NONE', #24297 ) ;
#20026 = CARTESIAN_POINT ( 'NONE',  ( -27.42409385541305511, -15.80920654474410725, 63.99999999999998579 ) ) ;
#20027 = DIRECTION ( 'NONE',  ( 1.000000000000000000, -0.000000000000000000, 0.000000000000000000 ) ) ;
#20028 = ORIENTED_EDGE ( 'NONE', *, *, #39444, .T. ) ;
#20029 = DIRECTION ( 'NONE',  ( 0.9687793358424822143, -0.2479245821708672415, 0.000000000000000000 ) ) ;
#20030 = CARTESIAN_POINT ( 'NONE',  ( -14.79551189520038967, -8.264331297124348552, 64.20467431377564083 ) ) ;
#20031 = DIRECTION ( 'NONE',  ( 0.3374354101627464186, 0.9413486835218386473, 1.423378189492272593E-08 ) ) ;
#20032 = CARTESIAN_POINT ( 'NONE',  ( -22.78003227265734765, -10.21913417830377036, 63.07185788080192879 ) ) ;
#20033 = CARTESIAN_POINT ( 'NONE',  ( -10.40127108354264429, -12.32249413655887871, 57.51352655450988749 ) ) ;
#20034 = ORIENTED_EDGE ( 'NONE', *, *, #10152, .F. ) ;
#20035 = CARTESIAN_POINT ( 'NONE',  ( -24.41485940220508510, -14.44976662329334616, 66.18292729254385165 ) ) ;
#20036 = CARTESIAN_POINT ( 'NONE',  ( -10.45859239952313224, -15.89938452881993847, 64.79299464097340433 ) ) ;
#20037 = CARTESIAN_POINT ( 'NONE',  ( -10.00761947527410634, -15.51609109068450465, 57.75288224187332276 ) ) ;
#20038 = VERTEX_POINT ( 'NONE', #42278 ) ;
#20039 = CARTESIAN_POINT ( 'NONE',  ( -12.64995486802317082, -19.99670083032576429, 68.33657438322859434 ) ) ;
#20040 =( BOUNDED_SURFACE ( )  B_SPLINE_SURFACE ( 3, 1, ( 
 ( #18872, #15158 ),
 ( #40132, #13755 ),
 ( #11482, #29039 ),
 ( #21178, #26506 ),
 ( #32725, #10339 ),
 ( #22829, #6394 ),
 ( #36409, #37316 ) ),
 .UNSPECIFIED., .T., .F., .F. ) 
 B_SPLINE_SURFACE_WITH_KNOTS ( ( 4, 3, 4 ),
 ( 2, 2 ),
 ( 0.000000000000000000, 0.5000000000000000000, 1.000000000000000000 ),
 ( 0.000000000000000000, 1.000000000000000000 ),
 .UNSPECIFIED. ) 
 GEOMETRIC_REPRESENTATION_ITEM ( )  RATIONAL_B_SPLINE_SURFACE ( (
 ( 1.000000000000000000, 1.000000000000000000),
 ( 0.3333333333333335369, 0.3333333333333330373),
 ( 0.3333333333333335369, 0.3333333333333330373),
 ( 1.000000000000000000, 1.000000000000000000),
 ( 0.3333333333333333703, 0.3333333333333333703),
 ( 0.3333333333333333703, 0.3333333333333333703),
 ( 1.000000000000000000, 1.000000000000000000) ) ) 
 REPRESENTATION_ITEM ( '' )  SURFACE ( )  );
#20041 = FACE_OUTER_BOUND ( 'NONE', #34604, .T. ) ;
#20042 = CARTESIAN_POINT ( 'NONE',  ( -17.58247036098680027, -9.298045829720972932, 53.88362224778186516 ) ) ;
#20043 = FACE_OUTER_BOUND ( 'NONE', #29659, .T. ) ;
#20044 = DIRECTION ( 'NONE',  ( 0.000000000000000000, 0.000000000000000000, -1.000000000000000000 ) ) ;
#20045 = ORIENTED_EDGE ( 'NONE', *, *, #14278, .F. ) ;
#20046 = ORIENTED_EDGE ( 'NONE', *, *, #9770, .T. ) ;
#20047 = CARTESIAN_POINT ( 'NONE',  ( -21.28659385541304161, -7.222650657624104298, 49.61879703869476543 ) ) ;
#20048 = EDGE_CURVE ( 'NONE', #10747, #43494, #12467, .T. ) ;
#20049 = ADVANCED_FACE ( 'NONE', ( #34871 ), #6009, .T. ) ;
#20050 = CARTESIAN_POINT ( 'NONE',  ( -19.96994574550859980, -21.32983827578761193, 72.40478737306770540 ) ) ;
#20051 = CARTESIAN_POINT ( 'NONE',  ( -15.35027142736847239, -7.653576728715946409, 74.26480947788739684 ) ) ;
#20052 = VECTOR ( 'NONE', #10476, 1000.000000000000000 ) ;
#20053 = ADVANCED_FACE ( 'NONE', ( #19533 ), #34295, .T. ) ;
#20054 = EDGE_CURVE ( 'NONE', #47542, #14105, #14449, .T. ) ;
#20055 = CARTESIAN_POINT ( 'NONE',  ( -19.30706890485013005, -22.01740903849647069, 58.64011989901568711 ) ) ;
#20056 = CARTESIAN_POINT ( 'NONE',  ( -20.88147674714181079, -8.209942860146695054, 60.02620543942160225 ) ) ;
#20057 = CIRCLE ( 'NONE', #17678, 5.249999999999998224 ) ;
#20058 = CARTESIAN_POINT ( 'NONE',  ( -9.982716906467198115, -14.44908523835941594, 67.97304809435139816 ) ) ;
#20059 = CARTESIAN_POINT ( 'NONE',  ( -24.23061318975584300, -17.83844832426134275, 62.61327595999730278 ) ) ;
#20060 = ORIENTED_EDGE ( 'NONE', *, *, #46088, .T. ) ;
#20061 = CARTESIAN_POINT ( 'NONE',  ( -23.66043351732632871, -18.11420823279021519, 59.14811234476497503 ) ) ;
#20062 = DIRECTION ( 'NONE',  ( -1.000000000000000000, 0.000000000000000000, 0.000000000000000000 ) ) ;
#20063 = ORIENTED_EDGE ( 'NONE', *, *, #10769, .F. ) ;
#20064 = CARTESIAN_POINT ( 'NONE',  ( -10.33483191699034265, -17.09962811228164270, 57.73114616685904110 ) ) ;
#20065 = DIRECTION ( 'NONE',  ( 0.9687793358424821033, -0.2479245821708677133, 0.000000000000000000 ) ) ;
#20066 = VERTEX_POINT ( 'NONE', #46124 ) ;
#20067 = DIRECTION ( 'NONE',  ( 2.866981220435666553E-17, -1.000000000000000000, -1.190614954331866791E-16 ) ) ;
#20068 = EDGE_CURVE ( 'NONE', #43006, #12881, #16351, .T. ) ;
#20069 = CARTESIAN_POINT ( 'NONE',  ( -10.00117625416208433, -15.44487358686203571, 57.68297391752145842 ) ) ;
#20070 = CARTESIAN_POINT ( 'NONE',  ( -21.84598475011588903, -8.812495317756813051, 70.31787921227815730 ) ) ;
#20071 = CARTESIAN_POINT ( 'NONE',  ( -24.32752865423570654, -15.96790753223159598, 66.36324927017490438 ) ) ;
#20072 = ORIENTED_EDGE ( 'NONE', *, *, #17610, .T. ) ;
#20073 = CARTESIAN_POINT ( 'NONE',  ( -24.72409385541305582, -14.90920654474412643, 59.01176470588234224 ) ) ;
#20074 = DIRECTION ( 'NONE',  ( 0.000000000000000000, -0.9999954153791273948, -0.003028072113819838245 ) ) ;
#20075 = CARTESIAN_POINT ( 'NONE',  ( -23.77395946432122997, -18.70572718374853594, 73.02014183918953449 ) ) ;
#20076 = FACE_BOUND ( 'NONE', #15235, .T. ) ;
#20077 = APPLICATION_PROTOCOL_DEFINITION ( 'draft international standard', 'automotive_design', 1998, #15516 ) ;
#20078 = FACE_OUTER_BOUND ( 'NONE', #31587, .T. ) ;
#20079 = CARTESIAN_POINT ( 'NONE',  ( -14.42683414290149813, -8.428067600363897682, 67.25975083869262505 ) ) ;
#20080 = CARTESIAN_POINT ( 'NONE',  ( 18.46573386768564973, 0.6667653706753842169, 50.27657325150214973 ) ) ;
#20081 = ORIENTED_EDGE ( 'NONE', *, *, #5847, .T. ) ;
#20082 = CARTESIAN_POINT ( 'NONE',  ( -10.70313947777602692, -12.85204326357734494, 64.26836087226253369 ) ) ;
#20083 = EDGE_LOOP ( 'NONE', ( #10280, #45481, #20483, #30027, #12253 ) ) ;
#20084 = CARTESIAN_POINT ( 'NONE',  ( -17.03931138636480824, -19.49188718695241462, 49.52966884056656482 ) ) ;
#20085 = CARTESIAN_POINT ( 'NONE',  ( -16.73406348812019928, -22.22719469671659809, 68.79586406416278521 ) ) ;
#20086 =( BOUNDED_CURVE ( )  B_SPLINE_CURVE ( 3, ( #25481, #6538, #10957, #6292 ),
 .UNSPECIFIED., .F., .F. ) 
 B_SPLINE_CURVE_WITH_KNOTS ( ( 4, 4 ),
 ( 0.4074455897393650106, 0.5000000000000000000 ),
 .UNSPECIFIED. ) 
 CURVE ( )  GEOMETRIC_REPRESENTATION_ITEM ( )  RATIONAL_B_SPLINE_CURVE ( ( 0.6983129098260945078, 0.7760317562606938724, 0.8765941196519940748, 0.9999999999999911182 ) ) 
 REPRESENTATION_ITEM ( '' )  );
#20087 = ORIENTED_EDGE ( 'NONE', *, *, #24945, .T. ) ;
#20088 = FACE_OUTER_BOUND ( 'NONE', #7834, .T. ) ;
#20089 = VECTOR ( 'NONE', #48365, 1000.000000000000000 ) ;
#20090 = FACE_BOUND ( 'NONE', #27769, .T. ) ;
#20091 = ORIENTED_EDGE ( 'NONE', *, *, #1190, .T. ) ;
#20092 = ORIENTED_EDGE ( 'NONE', *, *, #38850, .T. ) ;
#20093 = VERTEX_POINT ( 'NONE', #11915 ) ;
#20094 = CARTESIAN_POINT ( 'NONE',  ( -10.43098718212803000, -15.70539730037032911, 61.32316937334011442 ) ) ;
#20095 = CARTESIAN_POINT ( 'NONE',  ( -16.31159385759798752, -8.990409506049202193, 49.61344411288074951 ) ) ;
#20096 = DIRECTION ( 'NONE',  ( 0.000000000000000000, 0.000000000000000000, 1.000000000000000000 ) ) ;
#20097 = CARTESIAN_POINT ( 'NONE',  ( -10.96921284960095377, -11.97350354382807680, 74.84368195529052059 ) ) ;
#20098 = CARTESIAN_POINT ( 'NONE',  ( -16.29006019099003666, -22.17251760029243712, 61.87851267503305053 ) ) ;
#20099 =( BOUNDED_CURVE ( )  B_SPLINE_CURVE ( 3, ( #47494, #43805, #17671, #35897 ),
 .UNSPECIFIED., .F., .F. ) 
 B_SPLINE_CURVE_WITH_KNOTS ( ( 4, 4 ),
 ( 0.4074455897393731707, 0.5000000000000000000 ),
 .UNSPECIFIED. ) 
 CURVE ( )  GEOMETRIC_REPRESENTATION_ITEM ( )  RATIONAL_B_SPLINE_CURVE ( ( 0.6983129098261171563, 0.7760317562606884323, 0.8765941196519738687, 0.9999999999999514833 ) ) 
 REPRESENTATION_ITEM ( '' )  );
#20100 = VERTEX_POINT ( 'NONE', #8454 ) ;
#20101 = VERTEX_POINT ( 'NONE', #30150 ) ;
#20102 = CARTESIAN_POINT ( 'NONE',  ( -22.49909385650551741, -8.114302828567740988, 52.18300498402516041 ) ) ;
#20103 = ADVANCED_FACE ( 'NONE', ( #34541 ), #26933, .T. ) ;
#20104 = CARTESIAN_POINT ( 'NONE',  ( -22.42594789675818845, -19.77792426076253918, 69.45945937764655298 ) ) ;
#20105 = DIRECTION ( 'NONE',  ( -3.071710424422018668E-17, 6.404604876783312462E-16, 1.000000000000000000 ) ) ;
#20106 = CARTESIAN_POINT ( 'NONE',  ( -21.49815937814055999, -9.116931945208399668, 70.43132539264750847 ) ) ;
#20107 = ORIENTED_EDGE ( 'NONE', *, *, #29379, .F. ) ;
#20108 = CARTESIAN_POINT ( 'NONE',  ( -21.48659385650551457, -9.302874398569244363, 51.68646062012417985 ) ) ;
#20109 = B_SPLINE_CURVE_WITH_KNOTS ( 'NONE', 1,
 ( #20911, #35907 ),
 .UNSPECIFIED., .F., .F.,
 ( 2, 2 ),
 ( 0.000000000000000000, 1.000000000000000000 ),
 .UNSPECIFIED. ) ;
#20111 = VERTEX_POINT ( 'NONE', #8710 ) ;
#20110 = ADVANCED_FACE ( 'NONE', ( #30877 ), #826, .F. ) ;
#20112 = CARTESIAN_POINT ( 'NONE',  ( -23.09439563802003903, -10.70187420503893883, 59.79130591064781441 ) ) ;
#20113 = DIRECTION ( 'NONE',  ( 1.927470528863119542E-16, 0.000000000000000000, -1.000000000000000000 ) ) ;
#20114 = ADVANCED_FACE ( 'NONE', ( #348 ), #38480, .T. ) ;
#20115 = DIRECTION ( 'NONE',  ( -1.140458109893898545E-06, -1.256740822519431765E-06, 0.9999999999985598187 ) ) ;
#20116 = EDGE_CURVE ( 'NONE', #32298, #43417, #18803, .T. ) ;
#20117 = EDGE_LOOP ( 'NONE', ( #45150, #39861, #7114, #4588, #14959 ) ) ;
#20118 = CARTESIAN_POINT ( 'NONE',  ( -20.94909385541298974, -8.112991634885936776, 51.74999426922432377 ) ) ;
#20119 = CIRCLE ( 'NONE', #5158, 2.000000000000000888 ) ;
#20120 = CARTESIAN_POINT ( 'NONE',  ( -10.74628672884880309, -17.07053172313825939, 61.17215199736627795 ) ) ;
#20121 = CARTESIAN_POINT ( 'NONE',  ( -22.10931616815485512, -14.45671906187057765, 52.02966884056656482 ) ) ;
#20122 = CARTESIAN_POINT ( 'NONE',  ( -24.20565986263710201, -11.72478542327168327, 59.58961564006824574 ) ) ;
#20123 = VERTEX_POINT ( 'NONE', #30392 ) ;
#20124 = B_SPLINE_CURVE_WITH_KNOTS ( 'NONE', 3,
 ( #17410, #8959, #18875, #27176, #7563, #8719, #38488, #30885, #12158, #46131 ),
 .UNSPECIFIED., .F., .F.,
 ( 4, 2, 2, 2, 4 ),
 ( 0.1272669073658516392, 0.2522669073439419707, 0.3772669073220322744, 0.5022669073001225781, 0.6272669072782128818 ),
 .UNSPECIFIED. ) ;
#20125 = CARTESIAN_POINT ( 'NONE',  ( -10.44902906966473388, -15.40082580494429365, 57.86792826000680634 ) ) ;
#20126 = CARTESIAN_POINT ( 'NONE',  ( -24.82319332931276179, -15.68001985351029681, 73.16450280174184684 ) ) ;
#20127 = CARTESIAN_POINT ( 'NONE',  ( -12.41595477954341575, -20.32496163943406842, 68.49690828407896959 ) ) ;
#20128 = ORIENTED_EDGE ( 'NONE', *, *, #28355, .F. ) ;
#20129 = DIRECTION ( 'NONE',  ( -1.000000000000000000, 1.224646799147353207E-16, -4.267285103686820140E-17 ) ) ;
#20130 = VERTEX_POINT ( 'NONE', #15827 ) ;
#20131 = CYLINDRICAL_SURFACE ( 'NONE', #2981, 1.249999999999998668 ) ;
#20132 = CARTESIAN_POINT ( 'NONE',  ( -15.16478962180274870, -8.127860897350485558, 57.26488623981089177 ) ) ;
#20133 = VERTEX_POINT ( 'NONE', #11662 ) ;
#20134 = CARTESIAN_POINT ( 'NONE',  ( -38.65852941833841783, -25.10920654474410441, 78.99999999999998579 ) ) ;
#20135 = CARTESIAN_POINT ( 'NONE',  ( -17.42409385541299471, -14.80920654474434883, 62.02966884056656482 ) ) ;
#20136 = CARTESIAN_POINT ( 'NONE',  ( -15.12736045941317897, -21.89643407171298151, 68.69097498501147925 ) ) ;
#20137 = CARTESIAN_POINT ( 'NONE',  ( -11.55897615675186785, -7.397247749063358135, 53.49999999999995026 ) ) ;
#20138 = ORIENTED_EDGE ( 'NONE', *, *, #39785, .T. ) ;
#20139 = DIRECTION ( 'NONE',  ( -5.731567514496413899E-31, -1.020425574103664789E-16, -1.000000000000000000 ) ) ;
#20140 = CARTESIAN_POINT ( 'NONE',  ( -11.22844613476422460, -11.44458948612160043, 64.43409918096024569 ) ) ;
#20141 = FACE_OUTER_BOUND ( 'NONE', #32679, .T. ) ;
#20142 = CARTESIAN_POINT ( 'NONE',  ( -22.28894518008692316, -9.166670731632796887, 59.88317716683520331 ) ) ;
#20143 = ORIENTED_EDGE ( 'NONE', *, *, #16939, .T. ) ;
#20144 = CARTESIAN_POINT ( 'NONE',  ( -10.38752013045322009, -14.36951432065623813, 64.67331771650336236 ) ) ;
#20145 = CARTESIAN_POINT ( 'NONE',  ( -11.03038783319414939, -18.63467225643333336, 61.46366213062071182 ) ) ;
#20146 = VERTEX_POINT ( 'NONE', #45175 ) ;
#20147 = VERTEX_POINT ( 'NONE', #45891 ) ;
#20148 = CARTESIAN_POINT ( 'NONE',  ( -24.12071508562369715, -11.54438765950021306, 63.06722961171875852 ) ) ;
#20149 = CARTESIAN_POINT ( 'NONE',  ( -20.00853194199203600, -21.31477305597513094, 72.40478738567958317 ) ) ;
#20150 = CARTESIAN_POINT ( 'NONE',  ( -10.42707437616525645, -14.56501420157307791, 71.55612484073525081 ) ) ;
#20151 = CARTESIAN_POINT ( 'NONE',  ( -18.53034385650551386, -9.794322478646142471, 51.19202720610083901 ) ) ;
#20152 = CARTESIAN_POINT ( 'NONE',  ( -10.56492563526530581, -13.18000101695786341, 71.20828586226983248 ) ) ;
#20153 = EDGE_CURVE ( 'NONE', #22320, #34081, #16352, .T. ) ;
#20154 = CARTESIAN_POINT ( 'NONE',  ( -20.43749099114212342, -18.39845715627588874, 49.52966884056656482 ) ) ;
#20155 = LINE ( 'NONE', #8850, #35745 ) ;
#20156 = CARTESIAN_POINT ( 'NONE',  ( -11.32173637914110742, -11.26291225165672927, 67.76297573134488061 ) ) ;
#20157 = VECTOR ( 'NONE', #27265, 1000.000000000000227 ) ;
#20158 = AXIS2_PLACEMENT_3D ( 'NONE', #41351, #42092, #3941 ) ;
#20159 = VERTEX_POINT ( 'NONE', #37995 ) ;
#20160 = VERTEX_POINT ( 'NONE', #4281 ) ;
#20161 = CARTESIAN_POINT ( 'NONE',  ( -10.67448150008226904, -11.65383075329928886, 74.74495363721690921 ) ) ;
#20162 = CARTESIAN_POINT ( 'NONE',  ( -22.72031779163844334, -16.29245029320677673, 54.07175714974878389 ) ) ;
#20163 = CYLINDRICAL_SURFACE ( 'NONE', #23293, 0.1500000000000042133 ) ;
#20164 = CARTESIAN_POINT ( 'NONE',  ( -35.32409385541306079, -6.359206544744109735, 51.54999999999998295 ) ) ;
#20165 = VERTEX_POINT ( 'NONE', #19291 ) ;
#20166 = CARTESIAN_POINT ( 'NONE',  ( -4.424093855413049781, -25.10920654474410441, 52.99999999999998579 ) ) ;
#20167 = CARTESIAN_POINT ( 'NONE',  ( -12.96988148894724624, -20.27865218021415572, 71.80653631827996719 ) ) ;
#20168 = EDGE_CURVE ( 'NONE', #18224, #11801, #29599, .T. ) ;
#20169 = CARTESIAN_POINT ( 'NONE',  ( -21.79028809537168243, -9.273590339475653366, 63.47681654923867711 ) ) ;
#20170 = CARTESIAN_POINT ( 'NONE',  ( -11.08048641648777100, -18.71577166677792547, 61.47722039269356742 ) ) ;
#20171 = EDGE_CURVE ( 'NONE', #35776, #7471, #29144, .T. ) ;
#20172 = VERTEX_POINT ( 'NONE', #17026 ) ;
#20173 = CARTESIAN_POINT ( 'NONE',  ( -24.85346453946240786, -14.25412306239375049, 69.90921191474365060 ) ) ;
#20174 = EDGE_CURVE ( 'NONE', #15076, #29468, #10752, .T. ) ;
#20175 = CARTESIAN_POINT ( 'NONE',  ( -19.24025795797341942, -7.996846695050864540, 60.24620885950562865 ) ) ;
#20176 = ORIENTED_EDGE ( 'NONE', *, *, #1704, .T. ) ;
#20177 = CARTESIAN_POINT ( 'NONE',  ( -18.36404507162783162, -22.19967278815455458, 68.96514700280405918 ) ) ;
#20178 = EDGE_CURVE ( 'NONE', #17364, #39895, #23735, .T. ) ;
#20179 = CARTESIAN_POINT ( 'NONE',  ( -24.25171713147202368, -16.35308467727669068, 59.12332432120680181 ) ) ;
#20180 = EDGE_LOOP ( 'NONE', ( #11984, #24659, #23782, #3538 ) ) ;
#20181 = CARTESIAN_POINT ( 'NONE',  ( -20.31007010532247037, -7.940766544821113548, 70.37287609157104384 ) ) ;
#20182 = VECTOR ( 'NONE', #22155, 1000.000000000000000 ) ;
#20183 = VECTOR ( 'NONE', #44830, 1000.000000000000000 ) ;
#20184 = ORIENTED_EDGE ( 'NONE', *, *, #31988, .T. ) ;
#20185 = FACE_OUTER_BOUND ( 'NONE', #29074, .T. ) ;
#20186 = CARTESIAN_POINT ( 'NONE',  ( -18.60622096112062707, -22.16490860957766529, 72.47006221837980888 ) ) ;
#20187 = EDGE_LOOP ( 'NONE', ( #25482, #10075, #22575, #40391, #19070 ) ) ;
#20188 = CARTESIAN_POINT ( 'NONE',  ( -16.05534385541290376, -8.623186033802667794, 49.24843789510443059 ) ) ;
#20189 = CARTESIAN_POINT ( 'NONE',  ( -17.60534385650551670, -8.801233750844183135, 48.81488406609782515 ) ) ;
#20190 = ORIENTED_EDGE ( 'NONE', *, *, #14187, .T. ) ;
#20191 = CARTESIAN_POINT ( 'NONE',  ( -23.34481426128875015, -18.63642081788813343, 69.29371984264746231 ) ) ;
#20192 = AXIS2_PLACEMENT_3D ( 'NONE', #10040, #44034, #37089 ) ;
#20193 = CARTESIAN_POINT ( 'NONE',  ( -10.63534001824907449, -11.74074953021217382, 74.75851385465050214 ) ) ;
#20194 = LINE ( 'NONE', #31525, #40766 ) ;
#20195 = ORIENTED_EDGE ( 'NONE', *, *, #38766, .T. ) ;
#20196 = CARTESIAN_POINT ( 'NONE',  ( -16.19438353473653436, -7.918004163840022258, 60.48563071257218127 ) ) ;
#20197 = CARTESIAN_POINT ( 'NONE',  ( -11.73296596577226936, -10.64774513788296240, 74.72412863062541533 ) ) ;
#20198 = CARTESIAN_POINT ( 'NONE',  ( -12.74563483257940177, -17.19133189234193893, 52.02966884056656482 ) ) ;
#20199 = DIRECTION ( 'NONE',  ( 0.000000000000000000, -0.007114381193220334181, 0.9999746924698833528 ) ) ;
#20200 = CARTESIAN_POINT ( 'NONE',  ( -24.68275054790482770, -16.48720572190336853, 59.23837039904986312 ) ) ;
#20201 = ORIENTED_EDGE ( 'NONE', *, *, #17651, .F. ) ;
#20202 = ORIENTED_EDGE ( 'NONE', *, *, #1843, .T. ) ;
#20203 = FACE_OUTER_BOUND ( 'NONE', #8898, .T. ) ;
#20204 = CARTESIAN_POINT ( 'NONE',  ( -35.32409385541306079, -8.109206544744111511, 51.54999999999998295 ) ) ;
#20205 = ORIENTED_EDGE ( 'NONE', *, *, #32241, .F. ) ;
#20206 = CARTESIAN_POINT ( 'NONE',  ( -15.93879930885703011, -7.917138641544859468, 67.15479422225766371 ) ) ;
#20207 = CARTESIAN_POINT ( 'NONE',  ( -24.72409385541305582, -15.80920654474410725, 65.99999999999998579 ) ) ;
#20208 = CARTESIAN_POINT ( 'NONE',  ( -21.59909385759798894, -8.105421454601382081, 49.25000573077640098 ) ) ;
#20209 = LINE ( 'NONE', #1245, #28169 ) ;
#20210 = EDGE_CURVE ( 'NONE', #897, #188, #17279, .T. ) ;
#20211 = CARTESIAN_POINT ( 'NONE',  ( -10.98557796499954087, -17.68114198556070704, 71.86718193507100239 ) ) ;
#20212 = ORIENTED_EDGE ( 'NONE', *, *, #27682, .F. ) ;
#20213 = PLANE ( 'NONE',  #22584 ) ;
#20214 = CARTESIAN_POINT ( 'NONE',  ( -13.02047698205977433, -8.799930754719115455, 64.01608198847371511 ) ) ;
#20215 = CARTESIAN_POINT ( 'NONE',  ( 18.54465614458695910, 0.6404988570616596544, 50.61053642849761758 ) ) ;
#20216 = CARTESIAN_POINT ( 'NONE',  ( -14.51911023200684703, -18.48675360735852280, 49.52966884056656482 ) ) ;
#20217 = CARTESIAN_POINT ( 'NONE',  ( -50.42409385541304800, -25.10920654474410441, 63.99999999999998579 ) ) ;
#20218 =( BOUNDED_CURVE ( )  B_SPLINE_CURVE ( 3, ( #11247, #8061, #18367, #22083 ),
 .UNSPECIFIED., .F., .F. ) 
 B_SPLINE_CURVE_WITH_KNOTS ( ( 4, 4 ),
 ( 1.570796326794896780, 1.780235837034216617 ),
 .UNSPECIFIED. ) 
 CURVE ( )  GEOMETRIC_REPRESENTATION_ITEM ( )  RATIONAL_B_SPLINE_CURVE ( ( 1.000000000000000000, 0.9963479302455154896, 0.9963479302455154896, 1.000000000000000000 ) ) 
 REPRESENTATION_ITEM ( '' )  );
#20219 = EDGE_CURVE ( 'NONE', #44556, #17241, #36321, .T. ) ;
#20220 = ORIENTED_EDGE ( 'NONE', *, *, #35174, .F. ) ;
#20221 = VECTOR ( 'NONE', #33147, 1000.000000000000000 ) ;
#20222 = ORIENTED_EDGE ( 'NONE', *, *, #43997, .F. ) ;
#20223 = VECTOR ( 'NONE', #28152, 1000.000000000000000 ) ;
#20224 = VERTEX_POINT ( 'NONE', #24207 ) ;
#20225 = CARTESIAN_POINT ( 'NONE',  ( -24.47368665962210343, -14.70950332193510413, 62.72768537250228604 ) ) ;
#20226 = FACE_OUTER_BOUND ( 'NONE', #8145, .T. ) ;
#20227 = VECTOR ( 'NONE', #42952, 1000.000000000000114 ) ;
#20228 = VERTEX_POINT ( 'NONE', #20023 ) ;
#20229 =( BOUNDED_SURFACE ( )  B_SPLINE_SURFACE ( 3, 1, ( 
 ( #28771, #10307 ),
 ( #43804, #10059 ),
 ( #25082, #6364 ),
 ( #21396, #17670 ),
 ( #40335, #26534 ),
 ( #446, #27259 ),
 ( #23578, #33916 ) ),
 .UNSPECIFIED., .T., .F., .F. ) 
 B_SPLINE_SURFACE_WITH_KNOTS ( ( 4, 3, 4 ),
 ( 2, 2 ),
 ( 0.000000000000000000, 0.5000000000000000000, 1.000000000000000000 ),
 ( 0.000000000000000000, 1.000000000000000000 ),
 .UNSPECIFIED. ) 
 GEOMETRIC_REPRESENTATION_ITEM ( )  RATIONAL_B_SPLINE_SURFACE ( (
 ( 1.000000000000000000, 1.000000000000000000),
 ( 0.3333333333333335369, 0.3333333333333330373),
 ( 0.3333333333333335369, 0.3333333333333330373),
 ( 1.000000000000000000, 1.000000000000000000),
 ( 0.3333333333333333703, 0.3333333333333333703),
 ( 0.3333333333333333703, 0.3333333333333333703),
 ( 1.000000000000000000, 1.000000000000000000) ) ) 
 REPRESENTATION_ITEM ( '' )  SURFACE ( )  );
#20230 = CARTESIAN_POINT ( 'NONE',  ( -10.81696127132008023, -11.36705524461777905, 67.81875810329987075 ) ) ;
#20231 = EDGE_CURVE ( 'NONE', #16774, #28537, #20515, .T. ) ;
#20232 = B_SPLINE_CURVE_WITH_KNOTS ( 'NONE', 1,
 ( #12175, #46647 ),
 .UNSPECIFIED., .F., .F.,
 ( 2, 2 ),
 ( 0.000000000000000000, 1.000000000000000000 ),
 .UNSPECIFIED. ) ;
#20233 = DIRECTION ( 'NONE',  ( 0.000000000000000000, -0.9999954153791273948, -0.003028072113819838245 ) ) ;
#20234 = VERTEX_POINT ( 'NONE', #1544 ) ;
#20235 = B_SPLINE_CURVE_WITH_KNOTS ( 'NONE', 3,
 ( #1646, #1884, #12242, #5599, #9048, #9534, #35127, #23826, #35843, #31442 ),
 .UNSPECIFIED., .F., .F.,
 ( 4, 2, 2, 2, 4 ),
 ( 0.000000000000000000, 0.2500000000000000000, 0.5000000000000000000, 0.7500000000000000000, 1.000000000000000000 ),
 .UNSPECIFIED. ) ;
#20236 = CARTESIAN_POINT ( 'NONE',  ( -13.75915741662262270, -20.84105630778929097, 72.07040738930723478 ) ) ;
#20237 = EDGE_CURVE ( 'NONE', #6964, #37778, #7579, .T. ) ;
#20238 = CARTESIAN_POINT ( 'NONE',  ( -23.80698203817894054, -17.68407506542587271, 62.75744385471828934 ) ) ;
#20239 = B_SPLINE_CURVE_WITH_KNOTS ( 'NONE', 3,
 ( #15102, #38002, #30158, #44687, #37258, #40981, #45183, #3545, #11421, #18553 ),
 .UNSPECIFIED., .F., .F.,
 ( 4, 2, 2, 2, 4 ),
 ( 0.000000000000000000, 0.2500000000000000000, 0.5000000000000000000, 0.7500000000000000000, 1.000000000000000000 ),
 .UNSPECIFIED. ) ;
#20240 = ORIENTED_EDGE ( 'NONE', *, *, #30293, .T. ) ;
#20241 = CARTESIAN_POINT ( 'NONE',  ( -17.42409385541299471, -14.80920654474435771, 49.52966884056655772 ) ) ;
#20242 = CARTESIAN_POINT ( 'NONE',  ( -10.12033492330167306, -13.33947326246890341, 74.83850996365745800 ) ) ;
#20243 =( BOUNDED_SURFACE ( )  B_SPLINE_SURFACE ( 3, 1, ( 
 ( #24681, #5956 ),
 ( #35014, #5729 ),
 ( #1280, #20737 ),
 ( #1530, #35501 ),
 ( #12851, #35732 ),
 ( #27640, #27874 ),
 ( #42905, #39685 ) ),
 .UNSPECIFIED., .T., .F., .F. ) 
 B_SPLINE_SURFACE_WITH_KNOTS ( ( 4, 3, 4 ),
 ( 2, 2 ),
 ( 0.000000000000000000, 0.5000000000000000000, 1.000000000000000000 ),
 ( 0.000000000000000000, 1.000000000000000000 ),
 .UNSPECIFIED. ) 
 GEOMETRIC_REPRESENTATION_ITEM ( )  RATIONAL_B_SPLINE_SURFACE ( (
 ( 1.000000000000000000, 1.000000000000000000),
 ( 0.3333333333333335369, 0.3333333333333330373),
 ( 0.3333333333333335369, 0.3333333333333330373),
 ( 1.000000000000000000, 1.000000000000000000),
 ( 0.3333333333333333703, 0.3333333333333333703),
 ( 0.3333333333333333703, 0.3333333333333333703),
 ( 1.000000000000000000, 1.000000000000000000) ) ) 
 REPRESENTATION_ITEM ( '' )  SURFACE ( )  );
#20244 = ORIENTED_EDGE ( 'NONE', *, *, #3951, .T. ) ;
#20245 = CARTESIAN_POINT ( 'NONE',  ( -15.86712703025682103, -7.930203392541469221, 63.55522141739008646 ) ) ;
#20246 = CARTESIAN_POINT ( 'NONE',  ( -46.47622156840087371, -14.20920654474410760, 70.13000000000000966 ) ) ;
#20247 = CARTESIAN_POINT ( 'NONE',  ( -10.40888626530166405, -14.10966241957602207, 60.91821293886854249 ) ) ;
#20248 = VERTEX_POINT ( 'NONE', #28390 ) ;
#20249 = CARTESIAN_POINT ( 'NONE',  ( -24.25563565401629162, -17.78119069831516086, 62.57337365234224080 ) ) ;
#20250 = LINE ( 'NONE', #8044, #25772 ) ;
#20251 = CARTESIAN_POINT ( 'NONE',  ( -19.64535672665736143, -21.50393832739607802, 62.20323457844267523 ) ) ;
#20252 = EDGE_CURVE ( 'NONE', #3652, #16353, #20748, .T. ) ;
#20253 = CARTESIAN_POINT ( 'NONE',  ( -16.07865109465781117, -7.939724484389961034, 63.97011030347106697 ) ) ;
#20254 = FACE_OUTER_BOUND ( 'NONE', #2210, .T. ) ;
#20255 = FACE_OUTER_BOUND ( 'NONE', #47838, .T. ) ;
#20256 = ORIENTED_EDGE ( 'NONE', *, *, #13014, .T. ) ;
#20257 = CARTESIAN_POINT ( 'NONE',  ( -14.99973435974856883, -8.185210394751409879, 60.61996258296040452 ) ) ;
#20258 = EDGE_CURVE ( 'NONE', #12617, #11419, #43326, .T. ) ;
#20259 = CIRCLE ( 'NONE', #43066, 2.000000000000000000 ) ;
#20260 = CIRCLE ( 'NONE', #35954, 1.999999999999999778 ) ;
#20261 = CARTESIAN_POINT ( 'NONE',  ( -14.05658557958971855, -19.17473784764406020, 53.88362224778187226 ) ) ;
#20262 = CARTESIAN_POINT ( 'NONE',  ( -10.44916060947156566, -15.83526976542894182, 64.65771589744088033 ) ) ;
#20263 = FACE_OUTER_BOUND ( 'NONE', #17933, .T. ) ;
#20264 = B_SPLINE_CURVE_WITH_KNOTS ( 'NONE', 3,
 ( #45516, #34887, #30972, #8092, #4375, #45988, #12733, #23829, #27748, #46224 ),
 .UNSPECIFIED., .F., .F.,
 ( 4, 2, 2, 2, 4 ),
 ( 0.000000000000000000, 0.2500000000000000000, 0.5000000000000000000, 0.7500000000000000000, 1.000000000000000000 ),
 .UNSPECIFIED. ) ;
#20265 = CARTESIAN_POINT ( 'NONE',  ( -15.93879930885702656, -7.917138641544857691, 67.15479422225767792 ) ) ;
#20266 = EDGE_CURVE ( 'NONE', #33080, #20101, #9680, .T. ) ;
#20267 = EDGE_CURVE ( 'NONE', #13276, #22004, #27535, .T. ) ;
#20268 = CARTESIAN_POINT ( 'NONE',  ( -17.63034385650551528, -9.794322478646142471, 51.19202720610083190 ) ) ;
#20269 = ORIENTED_EDGE ( 'NONE', *, *, #22508, .T. ) ;
#20270 = FACE_BOUND ( 'NONE', #43201, .T. ) ;
#20271 = CARTESIAN_POINT ( 'NONE',  ( -20.35492123770571382, -11.13690394275196560, 49.52966884056655772 ) ) ;
#20272 = ORIENTED_EDGE ( 'NONE', *, *, #20396, .T. ) ;
#20273 = DIRECTION ( 'NONE',  ( -5.935091885548698876E-07, -2.117535313761473712E-07, 0.9999999999998014921 ) ) ;
#20274 = CARTESIAN_POINT ( 'NONE',  ( -17.42409385541299471, -14.80920654474435594, 52.02966884056656482 ) ) ;
#20275 = CARTESIAN_POINT ( 'NONE',  ( -17.93986882229626190, -22.24133833173343788, 62.07547122339882151 ) ) ;
#20276 = CIRCLE ( 'NONE', #5339, 1.999999999999999778 ) ;
#20277 = CARTESIAN_POINT ( 'NONE',  ( -12.79501450006381269, -20.06007546732424629, 68.44543540964158979 ) ) ;
#20278 = CARTESIAN_POINT ( 'NONE',  ( -23.42915847708036736, -11.11517115755410146, 73.64721174900437006 ) ) ;
#20279 = ORIENTED_EDGE ( 'NONE', *, *, #27552, .T. ) ;
#20280 = CIRCLE ( 'NONE', #33638, 2.000000000000000000 ) ;
#20281 = CARTESIAN_POINT ( 'NONE',  ( -19.90432934692537614, -21.83431937171774706, 69.04987052938618319 ) ) ;
#20282 = CARTESIAN_POINT ( 'NONE',  ( -10.84385027318267447, -17.33971308591566185, 64.92739379503987607 ) ) ;
#20283 = CARTESIAN_POINT ( 'NONE',  ( -18.95380389027981494, -7.978394929000565128, 63.53975171141463818 ) ) ;
#20284 = ORIENTED_EDGE ( 'NONE', *, *, #45089, .F. ) ;
#20285 = CARTESIAN_POINT ( 'NONE',  ( -23.93648101794248362, -17.51022725521227841, 65.95829288617392194 ) ) ;
#20286 = CARTESIAN_POINT ( 'NONE',  ( -45.92409385541306222, -13.70421070448077039, 73.00000000000001421 ) ) ;
#20287 = LINE ( 'NONE', #8732, #20611 ) ;
#20288 = CARTESIAN_POINT ( 'NONE',  ( -13.77492725671111806, -20.78292389580533595, 64.98628829336273327 ) ) ;
#20289 = FACE_OUTER_BOUND ( 'NONE', #28911, .T. ) ;
#20290 = ORIENTED_EDGE ( 'NONE', *, *, #41668, .F. ) ;
#20291 = EDGE_LOOP ( 'NONE', ( #16680, #48525, #26427, #40576 ) ) ;
#20292 = CARTESIAN_POINT ( 'NONE',  ( -19.99284385541304232, -8.630756214087126565, 51.74842643355248129 ) ) ;
#20293 = DIRECTION ( 'NONE',  ( 0.000000000000000000, 0.000000000000000000, -1.000000000000000000 ) ) ;
#20294 = AXIS2_PLACEMENT_3D ( 'NONE', #1781, #24443, #28116 ) ;
#20295 = DIRECTION ( 'NONE',  ( 0.9687793358424821033, -0.2479245821708679909, 0.000000000000000000 ) ) ;
#20296 = VECTOR ( 'NONE', #19655, 1000.000000000000000 ) ;
#20297 = AXIS2_PLACEMENT_3D ( 'NONE', #12960, #35849, #43754 ) ;
#20298 = EDGE_CURVE ( 'NONE', #35964, #32538, #30424, .T. ) ;
#20299 = LINE ( 'NONE', #16588, #2509 ) ;
#20300 = CARTESIAN_POINT ( 'NONE',  ( -13.97464618706818840, -20.90036148544157157, 68.74159733221011948 ) ) ;
#20301 = CARTESIAN_POINT ( 'NONE',  ( -9.979672921070292801, -14.51892525773737574, 67.90154210966345261 ) ) ;
#20302 = AXIS2_PLACEMENT_3D ( 'NONE', #35210, #42130, #1482 ) ;
#20303 = CARTESIAN_POINT ( 'NONE',  ( -24.23636277187043220, -17.82529184948975498, 62.58865552117998021 ) ) ;
#20304 = VERTEX_POINT ( 'NONE', #36144 ) ;
#20305 = LINE ( 'NONE', #27928, #20227 ) ;
#20306 = VECTOR ( 'NONE', #44505, 1000.000000000000000 ) ;
#20307 = DIRECTION ( 'NONE',  ( 0.9710973231077277834, -0.2386838684389877285, 7.431671637556432894E-08 ) ) ;
#20308 = ORIENTED_EDGE ( 'NONE', *, *, #16829, .F. ) ;
#20309 = CARTESIAN_POINT ( 'NONE',  ( -10.68602809008750576, -16.88409676349039046, 57.70232650191087487 ) ) ;
#20310 = CARTESIAN_POINT ( 'NONE',  ( -42.67115267894247665, -14.80920654474414810, 61.02352941176469869 ) ) ;
#20311 = ORIENTED_EDGE ( 'NONE', *, *, #18264, .F. ) ;
#20312 = DIRECTION ( 'NONE',  ( -3.071710424422018668E-17, 6.404604876783312462E-16, 1.000000000000000000 ) ) ;
#20313 = CARTESIAN_POINT ( 'NONE',  ( -14.25548580596218429, -11.33998781794830712, 49.52966884056655772 ) ) ;
#20314 = B_SPLINE_CURVE_WITH_KNOTS ( 'NONE', 3,
 ( #47733, #21409, #9838, #20915, #13974, #21161, #43818, #36395, #17453, #32481 ),
 .UNSPECIFIED., .F., .F.,
 ( 4, 2, 2, 2, 4 ),
 ( 0.000000000000000000, 0.2500000000000000000, 0.5000000000000000000, 0.7500000000000000000, 1.000000000000000000 ),
 .UNSPECIFIED. ) ;
#20315 = CARTESIAN_POINT ( 'NONE',  ( -20.04769106148205537, -8.319399502215615527, 70.47773761195011843 ) ) ;
#20316 = CARTESIAN_POINT ( 'NONE',  ( -19.34682484732250884, -8.026308974676197749, 59.96652798359869507 ) ) ;
#20317 = EDGE_LOOP ( 'NONE', ( #39664, #5946, #38335, #11938 ) ) ;
#20318 = FACE_OUTER_BOUND ( 'NONE', #3554, .T. ) ;
#20319 = DIRECTION ( 'NONE',  ( 0.9640890753730593232, -0.2655790932026004803, 6.310348465037888425E-08 ) ) ;
#20320 = CARTESIAN_POINT ( 'NONE',  ( -24.55824875695236287, -12.66269769826935310, 70.02888935069151444 ) ) ;
#20321 = ADVANCED_FACE ( 'NONE', ( #2667 ), #14176, .T. ) ;
#20322 = CARTESIAN_POINT ( 'NONE',  ( -17.42409385541299471, -14.80920654474435771, 49.52966884056655772 ) ) ;
#20323 = ADVANCED_FACE ( 'NONE', ( #40339 ), #43123, .T. ) ;
#20324 = EDGE_CURVE ( 'NONE', #6587, #38614, #10548, .T. ) ;
#20325 = LINE ( 'NONE', #9007, #10865 ) ;
#20326 = CARTESIAN_POINT ( 'NONE',  ( -17.43006558257920346, -7.359130651351934560, 67.27685495689534889 ) ) ;
#20327 = VECTOR ( 'NONE', #32884, 1000.000000000000000 ) ;
#20328 = DIRECTION ( 'NONE',  ( 0.000000000000000000, 0.000000000000000000, -1.000000000000000000 ) ) ;
#20329 = ORIENTED_EDGE ( 'NONE', *, *, #32346, .T. ) ;
#20330 = DIRECTION ( 'NONE',  ( -0.2771212459065067191, 0.9608349572466770017, 4.100231986695772107E-08 ) ) ;
#20331 =( BOUNDED_SURFACE ( )  B_SPLINE_SURFACE ( 3, 1, ( 
 ( #28057, #24382 ),
 ( #8385, #43082 ),
 ( #8881, #23661 ),
 ( #38403, #32002 ),
 ( #27581, #16720 ),
 ( #38901, #35200 ),
 ( #5180, #39140 ) ),
 .UNSPECIFIED., .T., .F., .F. ) 
 B_SPLINE_SURFACE_WITH_KNOTS ( ( 4, 3, 4 ),
 ( 2, 2 ),
 ( 0.000000000000000000, 0.5000000000000000000, 1.000000000000000000 ),
 ( 0.000000000000000000, 1.000000000000000000 ),
 .UNSPECIFIED. ) 
 GEOMETRIC_REPRESENTATION_ITEM ( )  RATIONAL_B_SPLINE_SURFACE ( (
 ( 1.000000000000000000, 1.000000000000000000),
 ( 0.3333333333333335369, 0.3333333333333330373),
 ( 0.3333333333333335369, 0.3333333333333330373),
 ( 1.000000000000000000, 1.000000000000000000),
 ( 0.3333333333333333703, 0.3333333333333333703),
 ( 0.3333333333333333703, 0.3333333333333333703),
 ( 1.000000000000000000, 1.000000000000000000) ) ) 
 REPRESENTATION_ITEM ( '' )  SURFACE ( )  );
#20332 = ORIENTED_EDGE ( 'NONE', *, *, #28547, .F. ) ;
#20333 = DIRECTION ( 'NONE',  ( 0.6380325334150255268, -0.7700094066334542964, 0.000000000000000000 ) ) ;
#20334 = CARTESIAN_POINT ( 'NONE',  ( -24.09792875595538320, -17.08130417324981565, 72.88336032035921619 ) ) ;
#20335 = VERTEX_POINT ( 'NONE', #39853 ) ;
#20336 = CARTESIAN_POINT ( 'NONE',  ( -19.86401518824997225, -21.42384811948916834, 69.22010401872219632 ) ) ;
#20337 = VECTOR ( 'NONE', #42568, 1000.000000000000000 ) ;
#20338 = EDGE_CURVE ( 'NONE', #15343, #28414, #19872, .T. ) ;
#20339 = CARTESIAN_POINT ( 'NONE',  ( -12.68532267716109985, -9.060482739934947460, 71.03420753023118550 ) ) ;
#20340 = EDGE_LOOP ( 'NONE', ( #19802, #46215 ) ) ;
#20341 = VERTEX_POINT ( 'NONE', #29012 ) ;
#20342 = ORIENTED_EDGE ( 'NONE', *, *, #39122, .T. ) ;
#20343 = CARTESIAN_POINT ( 'NONE',  ( -10.03016471889695183, -15.72215649304404117, 61.08143109537672188 ) ) ;
#20344 = VECTOR ( 'NONE', #13915, 999.9999999999998863 ) ;
#20345 = CARTESIAN_POINT ( 'NONE',  ( -17.42409385541299471, -14.80920654474434883, 62.02966884056656482 ) ) ;
#20346 = CARTESIAN_POINT ( 'NONE',  ( -10.03035368457962662, -15.72374687363213575, 61.22284448286259817 ) ) ;
#20347 = CARTESIAN_POINT ( 'NONE',  ( -13.46747890590686403, -9.034676489092227314, 60.43950277890026967 ) ) ;
#20348 = VERTEX_POINT ( 'NONE', #29495 ) ;
#20349 = VERTEX_POINT ( 'NONE', #10311 ) ;
#20350 = CARTESIAN_POINT ( 'NONE',  ( -20.47409385650551528, -9.792211528768504536, 50.49490371617623197 ) ) ;
#20351 = EDGE_CURVE ( 'NONE', #27679, #30553, #47255, .T. ) ;
#20352 = DIRECTION ( 'NONE',  ( -0.8839923186919886877, 0.4675014229855999348, -2.842058574697934120E-08 ) ) ;
#20353 = CARTESIAN_POINT ( 'NONE',  ( -18.02409385541303877, -9.359200813967568422, 50.49621490985803263 ) ) ;
#20354 = CARTESIAN_POINT ( 'NONE',  ( -23.27870965407892712, -18.64632446977878999, 66.01492505208454986 ) ) ;
#20355 = CARTESIAN_POINT ( 'NONE',  ( -22.83659385650551954, -6.915538690918074494, 49.31353937987644542 ) ) ;
#20356 = B_SPLINE_CURVE_WITH_KNOTS ( 'NONE', 3,
 ( #2757, #26153, #41164, #46076, #19737, #780, #1020, #26641, #532, #53 ),
 .UNSPECIFIED., .F., .F.,
 ( 4, 2, 2, 2, 4 ),
 ( 0.6272669072783091382, 0.7522669073001884144, 0.8772669073220678015, 1.002266907343947189, 1.127266907365826354 ),
 .UNSPECIFIED. ) ;
#20357 = VERTEX_POINT ( 'NONE', #44527 ) ;
#20358 = B_SPLINE_CURVE_WITH_KNOTS ( 'NONE', 3,
 ( #24322, #1408, #46954, #20859, #6076, #10017, #1900, #16902, #24077, #20381 ),
 .UNSPECIFIED., .F., .F.,
 ( 4, 2, 2, 2, 4 ),
 ( 0.000000000000000000, 0.2500000000000000000, 0.5000000000000000000, 0.7500000000000000000, 1.000000000000000000 ),
 .UNSPECIFIED. ) ;
#20359 = CYLINDRICAL_SURFACE ( 'NONE', #40592, 0.1500000000000060452 ) ;
#20360 = CARTESIAN_POINT ( 'NONE',  ( -10.37433175079900849, -14.87184048509926271, 74.79778922563521348 ) ) ;
#20361 = CIRCLE ( 'NONE', #3844, 5.249999999999998224 ) ;
#20362 = CARTESIAN_POINT ( 'NONE',  ( -36.42409385541304800, -9.359200813967566646, 50.49621490985803263 ) ) ;
#20363 = ORIENTED_EDGE ( 'NONE', *, *, #33848, .T. ) ;
#20364 = CARTESIAN_POINT ( 'NONE',  ( -21.17409385541299116, -6.859212275519752211, 50.50378509014304029 ) ) ;
#20365 = VECTOR ( 'NONE', #40420, 1000.000000000000227 ) ;
#20366 = CIRCLE ( 'NONE', #4616, 1.250000000000001110 ) ;
#20367 = FACE_OUTER_BOUND ( 'NONE', #14856, .T. ) ;
#20368 = CARTESIAN_POINT ( 'NONE',  ( -41.92997620835424044, -14.80920654474420139, 66.95294117647057419 ) ) ;
#20369 = FACE_OUTER_BOUND ( 'NONE', #40462, .T. ) ;
#20370 = ORIENTED_EDGE ( 'NONE', *, *, #34151, .T. ) ;
#20371 = CIRCLE ( 'NONE', #40026, 0.5560000000000009379 ) ;
#20372 = DIRECTION ( 'NONE',  ( 0.6043825497304157190, -0.7966942535134532433, 5.656674838975381179E-08 ) ) ;
#20373 = B_SPLINE_CURVE_WITH_KNOTS ( 'NONE', 1,
 ( #43212, #5791 ),
 .UNSPECIFIED., .F., .F.,
 ( 2, 2 ),
 ( 0.000000000000000000, 1.000000000000000000 ),
 .UNSPECIFIED. ) ;
#20374 =( BOUNDED_CURVE ( )  B_SPLINE_CURVE ( 3, ( #33437, #3424, #21657, #22636 ),
 .UNSPECIFIED., .F., .F. ) 
 B_SPLINE_CURVE_WITH_KNOTS ( ( 4, 4 ),
 ( 4.712388980384689674, 4.921828490624008623 ),
 .UNSPECIFIED. ) 
 CURVE ( )  GEOMETRIC_REPRESENTATION_ITEM ( )  RATIONAL_B_SPLINE_CURVE ( ( 1.000000000000000000, 0.9963479302455156006, 0.9963479302455156006, 1.000000000000000000 ) ) 
 REPRESENTATION_ITEM ( '' )  );
#20375 = CARTESIAN_POINT ( 'NONE',  ( -17.36015951656348832, -7.359395083792595216, 67.20534920880687935 ) ) ;
#20376 = DIRECTION ( 'NONE',  ( -3.071710424422018668E-17, 6.404604876783312462E-16, 1.000000000000000000 ) ) ;
#20377 = VERTEX_POINT ( 'NONE', #10782 ) ;
#20378 = CARTESIAN_POINT ( 'NONE',  ( -13.08950423898529891, -12.99622877252704001, 49.52966884056655772 ) ) ;
#20379 = ORIENTED_EDGE ( 'NONE', *, *, #38313, .F. ) ;
#20380 = CARTESIAN_POINT ( 'NONE',  ( -19.23450401370881124, -7.582471044449923703, 63.53815095794843160 ) ) ;
#20381 = CARTESIAN_POINT ( 'NONE',  ( -16.39888349198502127, -21.73372412438269308, 62.05568132716130236 ) ) ;
#20382 = ORIENTED_EDGE ( 'NONE', *, *, #10032, .F. ) ;
#20383 = EDGE_CURVE ( 'NONE', #23878, #36333, #7354, .T. ) ;
#20384 = DIRECTION ( 'NONE',  ( 0.9687793358424821033, -0.2479245821708679909, 0.000000000000000000 ) ) ;
#20385 = CARTESIAN_POINT ( 'NONE',  ( -10.44911129250985482, -12.18941988514178121, 57.51512593431250764 ) ) ;
#20386 = CARTESIAN_POINT ( 'NONE',  ( -13.24129617563109740, -8.644154241298165786, 60.69596227262822907 ) ) ;
#20387 = DIRECTION ( 'NONE',  ( -3.071710424422018668E-17, 6.404604876783312462E-16, 1.000000000000000000 ) ) ;
#20388 = VERTEX_POINT ( 'NONE', #3391 ) ;
#20389 = PRODUCT_DEFINITION_CONTEXT ( 'detailed design', #3598, 'design' ) ;
#20390 = CARTESIAN_POINT ( 'NONE',  ( -11.73260704738458671, -10.00184175524024610, 67.61401452035728710 ) ) ;
#20391 = CARTESIAN_POINT ( 'NONE',  ( -20.06975372951847447, -8.274133229585533655, 73.73568642813194174 ) ) ;
#20392 = EDGE_LOOP ( 'NONE', ( #37754, #36752, #31764, #45563 ) ) ;
#20393 = CARTESIAN_POINT ( 'NONE',  ( -10.61328331460780561, -11.78972931969595273, 74.73557151665039555 ) ) ;
#20394 =( BOUNDED_CURVE ( )  B_SPLINE_CURVE ( 3, ( #22490, #18792, #26428, #7734 ),
 .UNSPECIFIED., .F., .F. ) 
 B_SPLINE_CURVE_WITH_KNOTS ( ( 4, 4 ),
 ( 0.9074455897393638448, 1.000000000000000000 ),
 .UNSPECIFIED. ) 
 CURVE ( )  GEOMETRIC_REPRESENTATION_ITEM ( )  RATIONAL_B_SPLINE_CURVE ( ( 0.6983129098260933976, 0.7760317562606985353, 0.8765941196520007361, 1.000000000000000000 ) ) 
 REPRESENTATION_ITEM ( '' )  );
#20395 = EDGE_CURVE ( 'NONE', #25765, #11361, #18907, .T. ) ;
#20396 = EDGE_CURVE ( 'NONE', #27898, #25531, #44781, .T. ) ;
#20397 = PLANE ( 'NONE',  #47913 ) ;
#20398 = ORIENTED_EDGE ( 'NONE', *, *, #12549, .F. ) ;
#20399 = ORIENTED_EDGE ( 'NONE', *, *, #1147, .F. ) ;
#20400 = ADVANCED_FACE ( 'NONE', ( #45266 ), #39376, .T. ) ;
#20401 = CARTESIAN_POINT ( 'NONE',  ( -24.05420634179087358, -17.20676946999824608, 69.69867738674849988 ) ) ;
#20402 = CARTESIAN_POINT ( 'NONE',  ( -20.09525921507954038, -21.27957844515276875, 72.47766857650304928 ) ) ;
#20404 = CARTESIAN_POINT ( 'NONE',  ( -10.42496409221358178, -14.69883174549087279, 71.32782692796889989 ) ) ;
#20403 = AXIS2_PLACEMENT_3D ( 'NONE', #6221, #28397, #43422 ) ;
#20405 = CARTESIAN_POINT ( 'NONE',  ( -19.20534385650551457, -8.801233750844183135, 48.81488406609782515 ) ) ;
#20406 = ADVANCED_FACE ( 'NONE', ( #15425 ), #7842, .T. ) ;
#20407 = CARTESIAN_POINT ( 'NONE',  ( -12.32158608955787393, -9.943909642237139579, 60.57390139315987909 ) ) ;
#20408 = AXIS2_PLACEMENT_3D ( 'NONE', #46756, #20892, #16203 ) ;
#20409 = CARTESIAN_POINT ( 'NONE',  ( -19.53727001588333323, -22.01011538462517336, 53.63095954094023909 ) ) ;
#20410 = DIRECTION ( 'NONE',  ( -0.5022914217388751990, 0.8646984027090225400, 6.766381827299041184E-08 ) ) ;
#20411 = VECTOR ( 'NONE', #15041, 1000.000000000000114 ) ;
#20412 = AXIS2_PLACEMENT_3D ( 'NONE', #29094, #44148, #25407 ) ;
#20413 = CARTESIAN_POINT ( 'NONE',  ( -13.85036685459366090, -21.34611448311455106, 72.02633460110843089 ) ) ;
#20414 = EDGE_LOOP ( 'NONE', ( #16999, #13441 ) ) ;
#20415 = ORIENTED_EDGE ( 'NONE', *, *, #9046, .F. ) ;
#20416 = CARTESIAN_POINT ( 'NONE',  ( -12.34763169630739732, -20.26208273980121533, 68.51470172492967947 ) ) ;
#20417 = ADVANCED_FACE ( 'NONE', ( #30732 ), #22862, .T. ) ;
#20418 = CARTESIAN_POINT ( 'NONE',  ( 0.000000000000000000, 0.000000000000000000, 0.000000000000000000 ) ) ;
#20419 = CARTESIAN_POINT ( 'NONE',  ( -23.63040034176007609, -11.57141379323375219, 66.42214533111976493 ) ) ;
#20420 = VECTOR ( 'NONE', #7199, 1000.000000000000000 ) ;
#20421 = CARTESIAN_POINT ( 'NONE',  ( -22.45398830698411174, -19.67764612419960457, 72.64400540998924782 ) ) ;
#20422 = DIRECTION ( 'NONE',  ( 3.484385612528001215E-15, 0.000000000000000000, -1.000000000000000000 ) ) ;
#20423 = ORIENTED_EDGE ( 'NONE', *, *, #45828, .T. ) ;
#20424 = CARTESIAN_POINT ( 'NONE',  ( -20.23203131230217267, -21.71059417314907591, 72.51823477531823414 ) ) ;
#20425 = CARTESIAN_POINT ( 'NONE',  ( -24.72409385541305582, -15.80920654474410725, 65.99999999999998579 ) ) ;
#20426 = CYLINDRICAL_SURFACE ( 'NONE', #33093, 1.250000000000007994 ) ;
#20427 = CYLINDRICAL_SURFACE ( 'NONE', #1267, 1.999999999999999556 ) ;
#20428 = VERTEX_POINT ( 'NONE', #30493 ) ;
#20429 = CARTESIAN_POINT ( 'NONE',  ( -12.74698474939898496, -12.42443183621510094, 49.52966884056655772 ) ) ;
#20430 = DIRECTION ( 'NONE',  ( -3.071710424422018668E-17, 6.404604876783312462E-16, 1.000000000000000000 ) ) ;
#20431 = AXIS2_PLACEMENT_3D ( 'NONE', #22243, #44657, #29386 ) ;
#20432 = FACE_OUTER_BOUND ( 'NONE', #4481, .T. ) ;
#20433 = CYLINDRICAL_SURFACE ( 'NONE', #48549, 0.1499999999999992450 ) ;
#20434 = CARTESIAN_POINT ( 'NONE',  ( -22.49909385759799108, -8.105421454601382081, 49.25000573077640098 ) ) ;
#20435 = EDGE_CURVE ( 'NONE', #4639, #29387, #7103, .T. ) ;
#20436 = ORIENTED_EDGE ( 'NONE', *, *, #40106, .F. ) ;
#20437 = CARTESIAN_POINT ( 'NONE',  ( -20.31649657898477912, -7.943510300654241796, 70.43595776394847974 ) ) ;
#20438 = AXIS2_PLACEMENT_3D ( 'NONE', #8353, #11554, #12045 ) ;
#20439 = VERTEX_POINT ( 'NONE', #45508 ) ;
#20440 = CARTESIAN_POINT ( 'NONE',  ( -10.01583252691979986, -14.02010874201704738, 61.05787945157973695 ) ) ;
#20441 = CARTESIAN_POINT ( 'NONE',  ( -15.18259368501833784, -19.55664553709809894, 50.77966884056656482 ) ) ;
#20442 = VERTEX_POINT ( 'NONE', #8090 ) ;
#20443 = CARTESIAN_POINT ( 'NONE',  ( -10.69179989897285310, -16.90224548161295814, 57.69320343077063740 ) ) ;
#20444 = EDGE_CURVE ( 'NONE', #44245, #14220, #3636, .T. ) ;
#20445 = DIRECTION ( 'NONE',  ( 0.7700094066334511878, 0.6380325334150293015, 0.000000000000000000 ) ) ;
#20446 = CARTESIAN_POINT ( 'NONE',  ( -17.71784385650551741, -9.790100578890868377, 49.79778022625163203 ) ) ;
#20447 = ORIENTED_EDGE ( 'NONE', *, *, #32466, .F. ) ;
#20448 = VECTOR ( 'NONE', #19180, 1000.000000000000000 ) ;
#20449 = CARTESIAN_POINT ( 'NONE',  ( -14.93181132608235195, -7.787654600965993268, 57.03655263075181381 ) ) ;
#20450 = EDGE_LOOP ( 'NONE', ( #10509, #6604, #1032, #19582 ) ) ;
#20451 = DIRECTION ( 'NONE',  ( -3.071710424422018668E-17, 6.404604876783312462E-16, 1.000000000000000000 ) ) ;
#20452 = CARTESIAN_POINT ( 'NONE',  ( -45.92409385541306222, -14.80920654474410902, 68.00000000000000000 ) ) ;
#20453 = DIRECTION ( 'NONE',  ( -0.9922778767136676281, -4.321618136576820974E-17, 0.1240347345892086200 ) ) ;
#20454 = CARTESIAN_POINT ( 'NONE',  ( -24.59706333651279664, -12.79617740830267891, 66.48742133194130588 ) ) ;
#20455 = B_SPLINE_CURVE_WITH_KNOTS ( 'NONE', 1,
 ( #28659, #47618 ),
 .UNSPECIFIED., .F., .F.,
 ( 2, 2 ),
 ( 0.000000000000000000, 1.000000000000000000 ),
 .UNSPECIFIED. ) ;
#20456 = CARTESIAN_POINT ( 'NONE',  ( -20.68576094134451182, -21.00469108578126765, 62.22544513427146740 ) ) ;
#20458 = ORIENTED_EDGE ( 'NONE', *, *, #13982, .T. ) ;
#20457 = AXIS2_PLACEMENT_3D ( 'NONE', #950, #34672, #15212 ) ;
#20459 = ORIENTED_EDGE ( 'NONE', *, *, #47125, .F. ) ;
#20460 = EDGE_CURVE ( 'NONE', #27240, #20428, #2231, .T. ) ;
#20461 = CARTESIAN_POINT ( 'NONE',  ( -14.66630222544869078, -8.320656262913125545, 63.80450889863892172 ) ) ;
#20462 = CARTESIAN_POINT ( 'NONE',  ( -10.08052675126636721, -16.06451543208143917, 68.09272439531302723 ) ) ;
#20463 = ORIENTED_EDGE ( 'NONE', *, *, #14011, .T. ) ;
#20464 = FACE_OUTER_BOUND ( 'NONE', #44497, .T. ) ;
#20465 = FACE_OUTER_BOUND ( 'NONE', #40885, .T. ) ;
#20466 = CARTESIAN_POINT ( 'NONE',  ( -18.39284385759798823, -8.630756214087126565, 51.74842643355248129 ) ) ;
#20467 = EDGE_CURVE ( 'NONE', #48485, #16276, #47507, .T. ) ;
#20468 = CARTESIAN_POINT ( 'NONE',  ( -12.64995474452274316, -19.99670071527213366, 68.63657438322856308 ) ) ;
#20469 = CARTESIAN_POINT ( 'NONE',  ( -11.25989433568915032, -11.38792842781904469, 64.44882039367774951 ) ) ;
#20470 = FACE_OUTER_BOUND ( 'NONE', #21778, .T. ) ;
#20471 = VERTEX_POINT ( 'NONE', #26057 ) ;
#20472 = EDGE_CURVE ( 'NONE', #15515, #25922, #48697, .T. ) ;
#20473 = CARTESIAN_POINT ( 'NONE',  ( -16.50454646563301964, -22.20232569423288282, 65.34069100801451668 ) ) ;
#20474 = CARTESIAN_POINT ( 'NONE',  ( -15.61111608319569477, -19.14379616117205885, 49.52966884056656482 ) ) ;
#20475 = VECTOR ( 'NONE', #21873, 1000.000000000000000 ) ;
#20476 = CIRCLE ( 'NONE', #19697, 1.250000000000001110 ) ;
#20477 = FACE_OUTER_BOUND ( 'NONE', #3586, .T. ) ;
#20478 = LINE ( 'NONE', #21197, #5676 ) ;
#20479 = EDGE_CURVE ( 'NONE', #3957, #23794, #16586, .T. ) ;
#20480 = EDGE_LOOP ( 'NONE', ( #7369, #36661 ) ) ;
#20481 = EDGE_LOOP ( 'NONE', ( #6663, #47030, #15268, #37150, #43777 ) ) ;
#20482 = B_SPLINE_CURVE_WITH_KNOTS ( 'NONE', 3,
 ( #23580, #12952, #42289, #8809, #43004, #19881, #27023, #31438, #31684, #12240 ),
 .UNSPECIFIED., .F., .F.,
 ( 4, 2, 2, 2, 4 ),
 ( 0.000000000000000000, 0.2500000000000000000, 0.5000000000000000000, 0.7500000000000000000, 1.000000000000000000 ),
 .UNSPECIFIED. ) ;
#20483 = ORIENTED_EDGE ( 'NONE', *, *, #18315, .T. ) ;
#20484 = CARTESIAN_POINT ( 'NONE',  ( -41.67850562011894766, -14.90920654474422058, 68.96470588235293064 ) ) ;
#20485 = PRESENTATION_STYLE_ASSIGNMENT (( #23514 ) ) ;
#20486 = CARTESIAN_POINT ( 'NONE',  ( -13.30711168077662521, -9.147894172712071281, 64.20946529582356277 ) ) ;
#20487 = VECTOR ( 'NONE', #8820, 1000.000000000000227 ) ;
#20488 = ORIENTED_EDGE ( 'NONE', *, *, #829, .T. ) ;
#20489 = CARTESIAN_POINT ( 'NONE',  ( -10.83189492465945669, -11.33829310736856044, 67.79677371063019109 ) ) ;
#20490 = CARTESIAN_POINT ( 'NONE',  ( -10.37974201859533707, -14.52605273603761660, 68.15800121751649954 ) ) ;
#20491 = VERTEX_POINT ( 'NONE', #15923 ) ;
#20492 = CARTESIAN_POINT ( 'NONE',  ( -20.25191534917340874, -8.350868906188830820, 70.26572394742477456 ) ) ;
#20493 = ORIENTED_EDGE ( 'NONE', *, *, #231, .T. ) ;
#20494 = CARTESIAN_POINT ( 'NONE',  ( -10.78748997988023639, -12.58311375253882325, 57.51960598127043767 ) ) ;
#20495 = EDGE_CURVE ( 'NONE', #45387, #11424, #20482, .T. ) ;
#20496 = EDGE_LOOP ( 'NONE', ( #21483, #47932 ) ) ;
#20497 = CARTESIAN_POINT ( 'NONE',  ( -22.62394951084894146, -10.04809318868971424, 70.29706442286226320 ) ) ;
#20498 = ORIENTED_EDGE ( 'NONE', *, *, #43738, .F. ) ;
#20499 = DIRECTION ( 'NONE',  ( 0.9956360040033426229, -0.09332174201254549162, 0.000000000000000000 ) ) ;
#20500 = CARTESIAN_POINT ( 'NONE',  ( -22.47397867527990201, -20.28676549996637135, 65.86568223911946518 ) ) ;
#20501 = ORIENTED_EDGE ( 'NONE', *, *, #48546, .F. ) ;
#20502 = CARTESIAN_POINT ( 'NONE',  ( -8.424093855413094190, -6.359206544744109735, 64.00000000000002842 ) ) ;
#20503 = CARTESIAN_POINT ( 'NONE',  ( -24.42531087273439994, -14.77968204897741167, 62.94126267090115334 ) ) ;
#20504 = FACE_OUTER_BOUND ( 'NONE', #8775, .T. ) ;
#20505 = CIRCLE ( 'NONE', #24448, 5.249999999999998224 ) ;
#20506 = CARTESIAN_POINT ( 'NONE',  ( -16.16063032598464133, -7.467038112641824377, 60.38523865926408263 ) ) ;
#20507 = DIRECTION ( 'NONE',  ( -3.071710424422018668E-17, 6.404604876783312462E-16, 1.000000000000000000 ) ) ;
#20508 = CARTESIAN_POINT ( 'NONE',  ( -15.56465948913149155, -7.543361525925791788, 54.27966884056655061 ) ) ;
#20509 = ORIENTED_EDGE ( 'NONE', *, *, #45969, .T. ) ;
#20510 = AXIS2_PLACEMENT_3D ( 'NONE', #40283, #13905, #21085 ) ;
#20511 = DIRECTION ( 'NONE',  ( 1.000000000000000000, -4.164305804376849172E-17, 1.614929280266638808E-16 ) ) ;
#20512 = CARTESIAN_POINT ( 'NONE',  ( -11.79792992861738909, -18.97409303405279957, 71.98685885147807539 ) ) ;
#20513 = CARTESIAN_POINT ( 'NONE',  ( -24.86242983737997747, -14.39095285025967286, 66.36788159907001727 ) ) ;
#20514 = CARTESIAN_POINT ( 'NONE',  ( -15.13462684854361306, -21.89875038763135606, 68.68318760819161639 ) ) ;
#20515 = LINE ( 'NONE', #47096, #18954 ) ;
#20516 = CARTESIAN_POINT ( 'NONE',  ( -14.93034385650551599, -9.794322478646142471, 51.19202720610083190 ) ) ;
#20517 = ORIENTED_EDGE ( 'NONE', *, *, #46598, .T. ) ;
#20518 = ADVANCED_FACE ( 'NONE', ( #24307 ), #27978, .F. ) ;
#20519 = CARTESIAN_POINT ( 'NONE',  ( -22.75923480142028055, -10.27751027444597653, 66.84182257657300852 ) ) ;
#20520 = CARTESIAN_POINT ( 'NONE',  ( -10.86718109655241626, -12.20887211208692413, 57.62857328228790976 ) ) ;
#20521 = VERTEX_POINT ( 'NONE', #39060 ) ;
#20522 = CARTESIAN_POINT ( 'NONE',  ( -11.45045256087476027, -18.56827314959498310, 68.36122809857093330 ) ) ;
#20523 = FACE_OUTER_BOUND ( 'NONE', #32004, .T. ) ;
#20524 = CIRCLE ( 'NONE', #41745, 1.999999999999994893 ) ;
#20525 = CARTESIAN_POINT ( 'NONE',  ( -22.75539019595755263, -10.19575032747719590, 66.82710158566565894 ) ) ;
#20526 = ADVANCED_FACE ( 'NONE', ( #12480 ), #1882, .T. ) ;
#20527 = CARTESIAN_POINT ( 'NONE',  ( -15.44746548810605447, -21.57648140951198812, 72.04575476862331129 ) ) ;
#20528 =( BOUNDED_CURVE ( )  B_SPLINE_CURVE ( 3, ( #40863, #29539, #18441, #33449 ),
 .UNSPECIFIED., .F., .F. ) 
 B_SPLINE_CURVE_WITH_KNOTS ( ( 4, 4 ),
 ( 0.4074455897393652326, 0.5000000000000000000 ),
 .UNSPECIFIED. ) 
 CURVE ( )  GEOMETRIC_REPRESENTATION_ITEM ( )  RATIONAL_B_SPLINE_CURVE ( ( 0.6983129098260896228, 0.7760317562606828812, 0.8765941196519826395, 0.9999999999999802380 ) ) 
 REPRESENTATION_ITEM ( '' )  );
#20529 = ORIENTED_EDGE ( 'NONE', *, *, #47125, .T. ) ;
#20530 = CARTESIAN_POINT ( 'NONE',  ( -12.09359296509799719, -9.604326949652671530, 57.24968926044763862 ) ) ;
#20531 = PLANE ( 'NONE',  #39864 ) ;
#20532 = EDGE_CURVE ( 'NONE', #31415, #19901, #24586, .T. ) ;
#20533 = CARTESIAN_POINT ( 'NONE',  ( -13.82526118368687484, -18.63162768858978779, 50.77966884056655772 ) ) ;
#20534 = ORIENTED_EDGE ( 'NONE', *, *, #48683, .F. ) ;
#20535 = VECTOR ( 'NONE', #23227, 1000.000000000000000 ) ;
#20536 = DIRECTION ( 'NONE',  ( -3.071710424422018668E-17, 6.404604876783312462E-16, 1.000000000000000000 ) ) ;
#20537 = ADVANCED_FACE ( 'NONE', ( #38826 ), #8316, .T. ) ;
#20538 = CARTESIAN_POINT ( 'NONE',  ( -24.41897151118743636, -17.37347349776957017, 69.59835227440868266 ) ) ;
#20539 = CARTESIAN_POINT ( 'NONE',  ( -13.83484324388145303, -17.82260368047347399, 49.52966884056656482 ) ) ;
#20540 = CARTESIAN_POINT ( 'NONE',  ( -16.76159385759799036, -7.228003583438117552, 51.38655588711986155 ) ) ;
#20541 = CARTESIAN_POINT ( 'NONE',  ( -24.11794058161805054, -12.76166764465371628, 69.77243002474142486 ) ) ;
#20542 =( BOUNDED_CURVE ( )  B_SPLINE_CURVE ( 3, ( #12341, #27361, #34250, #19006 ),
 .UNSPECIFIED., .F., .F. ) 
 B_SPLINE_CURVE_WITH_KNOTS ( ( 4, 4 ),
 ( 0.000000000000000000, 0.4074455897393681747 ),
 .UNSPECIFIED. ) 
 CURVE ( )  GEOMETRIC_REPRESENTATION_ITEM ( )  RATIONAL_B_SPLINE_CURVE ( ( 1.000000000000000000, 0.4567392136813264170, 0.3561768502900282130, 0.6983129098261053880 ) ) 
 REPRESENTATION_ITEM ( '' )  );
#20543 = ORIENTED_EDGE ( 'NONE', *, *, #43986, .F. ) ;
#20544 = EDGE_LOOP ( 'NONE', ( #49, #24478, #48358, #6571 ) ) ;
#20545 = CARTESIAN_POINT ( 'NONE',  ( -21.79284385541304658, -8.630756214087126565, 51.74842643355248129 ) ) ;
#20546 = VECTOR ( 'NONE', #1381, 1000.000000000000000 ) ;
#20547 = CARTESIAN_POINT ( 'NONE',  ( -13.27359419718654365, -9.172268535653204324, 64.20946477989005530 ) ) ;
#20548 = AXIS2_PLACEMENT_3D ( 'NONE', #21884, #29516, #32488 ) ;
#20549 = FACE_OUTER_BOUND ( 'NONE', #795, .T. ) ;
#20550 = ADVANCED_FACE ( 'NONE', ( #35368 ), #12727, .T. ) ;
#20551 = CARTESIAN_POINT ( 'NONE',  ( -12.01932494161596487, -10.27783711031607261, 71.38381879606350822 ) ) ;
#20552 =( BOUNDED_CURVE ( )  B_SPLINE_CURVE ( 2, ( #26684, #46120, #19528, #34536, #12624, #27401, #820, #30632, #45658 ),
 .UNSPECIFIED., .F., .F. ) 
 B_SPLINE_CURVE_WITH_KNOTS ( ( 3, 2, 2, 2, 3 ),
 ( 0.4583333333333333148, 0.4687500000000000555, 0.4791666666666667962, 0.4895833333333334814, 0.5000000000000002220 ),
 .UNSPECIFIED. ) 
 CURVE ( )  GEOMETRIC_REPRESENTATION_ITEM ( )  RATIONAL_B_SPLINE_CURVE ( ( 1.000000000000000000, 0.9238795325112867385, 1.000000000000000000, 0.9238795325112867385, 1.000000000000000000, 0.9238795325112867385, 1.000000000000000000, 0.9238795325112850731, 1.000000000000001554 ) ) 
 REPRESENTATION_ITEM ( '' )  );
#20553 = EDGE_CURVE ( 'NONE', #1779, #12574, #38077, .T. ) ;
#20554 = CARTESIAN_POINT ( 'NONE',  ( -23.00381842360518547, -10.58230771189866104, 59.90203429537245228 ) ) ;
#20555 = EDGE_CURVE ( 'NONE', #45977, #7144, #12009, .T. ) ;
#20556 = CARTESIAN_POINT ( 'NONE',  ( -11.75774202113761113, -19.00384077433692909, 71.83685884782747166 ) ) ;
#20557 = VERTEX_POINT ( 'NONE', #20362 ) ;
#20558 = CARTESIAN_POINT ( 'NONE',  ( -19.94917705995926482, -8.226604131702123013, 74.00624557436877637 ) ) ;
#20559 = EDGE_CURVE ( 'NONE', #44086, #8618, #22216, .T. ) ;
#20560 = VECTOR ( 'NONE', #11567, 1000.000000000000000 ) ;
#20561 = CARTESIAN_POINT ( 'NONE',  ( -18.12432747636454877, -22.22630431188652977, 65.60178084401016463 ) ) ;
#20562 = ORIENTED_EDGE ( 'NONE', *, *, #34654, .F. ) ;
#20563 = CARTESIAN_POINT ( 'NONE',  ( -23.83080496556880945, -17.75212211224490133, 59.28906343887996400 ) ) ;
#20564 = CARTESIAN_POINT ( 'NONE',  ( -11.93522140360746064, -14.45952210441258501, 53.49999999999995026 ) ) ;
#20565 = EDGE_LOOP ( 'NONE', ( #14762, #19395, #28471, #14099 ) ) ;
#20566 = DIRECTION ( 'NONE',  ( 0.000000000000000000, 0.000000000000000000, 1.000000000000000000 ) ) ;
#20567 = CARTESIAN_POINT ( 'NONE',  ( -12.17848458102417908, -19.44617700360637613, 58.15512196582962900 ) ) ;
#20568 = ORIENTED_EDGE ( 'NONE', *, *, #32277, .F. ) ;
#20569 = FACE_OUTER_BOUND ( 'NONE', #6468, .T. ) ;
#20570 = CARTESIAN_POINT ( 'NONE',  ( -19.85534385759799392, -8.623186033802570094, 49.24843789510466507 ) ) ;
#20571 = CARTESIAN_POINT ( 'NONE',  ( -24.40987808923448554, -15.75888385863607333, 69.83307461037107089 ) ) ;
#20572 = DIRECTION ( 'NONE',  ( 0.9687793358424822143, -0.2479245821708672415, 0.000000000000000000 ) ) ;
#20573 = VERTEX_POINT ( 'NONE', #925 ) ;
#20574 = CARTESIAN_POINT ( 'NONE',  ( -10.33431758219403207, -12.52035302217920254, 60.98348881056122650 ) ) ;
#20575 = FACE_OUTER_BOUND ( 'NONE', #25475, .T. ) ;
#20576 = CARTESIAN_POINT ( 'NONE',  ( -23.10841418202883446, -18.98556259803724799, 65.91569706707790033 ) ) ;
#20577 = CARTESIAN_POINT ( 'NONE',  ( -12.01648241349452917, -10.28590705807702932, 67.49896869922172016 ) ) ;
#20578 = PRESENTATION_LAYER_ASSIGNMENT (  '', '', ( #6397 ) ) ;
#20579 = CARTESIAN_POINT ( 'NONE',  ( -18.25635609959491035, -22.28132141893295071, 53.76227901944321275 ) ) ;
#20580 = DIRECTION ( 'NONE',  ( -3.071710424422018668E-17, 6.404604876783312462E-16, 1.000000000000000000 ) ) ;
#20581 = AXIS2_PLACEMENT_3D ( 'NONE', #14113, #43479, #10224 ) ;
#20582 = ORIENTED_EDGE ( 'NONE', *, *, #39631, .T. ) ;
#20583 = DIRECTION ( 'NONE',  ( 1.224646799147353207E-16, 1.000000000000000000, -1.912410701131276611E-32 ) ) ;
#20584 = CARTESIAN_POINT ( 'NONE',  ( -15.79771479060332240, -19.20445095063907104, 52.02966884056656482 ) ) ;
#20585 = EDGE_LOOP ( 'NONE', ( #14912, #5978, #26841, #44416, #35266 ) ) ;
#20586 = CARTESIAN_POINT ( 'NONE',  ( -19.83852420082105894, -21.85790785478787868, 69.12137763959520953 ) ) ;
#20587 = EDGE_CURVE ( 'NONE', #39291, #7384, #42554, .T. ) ;
#20588 = ORIENTED_EDGE ( 'NONE', *, *, #4173, .F. ) ;
#20589 = ORIENTED_EDGE ( 'NONE', *, *, #26318, .T. ) ;
#20590 = VERTEX_POINT ( 'NONE', #1153 ) ;
#20591 = ADVANCED_FACE ( 'NONE', ( #27504 ), #40509, .T. ) ;
#20592 = DIRECTION ( 'NONE',  ( -3.071710424422018668E-17, 6.404604876783312462E-16, 1.000000000000000000 ) ) ;
#20593 = DIRECTION ( 'NONE',  ( 0.000000000000000000, 0.000000000000000000, 1.000000000000000000 ) ) ;
#20594 = DIRECTION ( 'NONE',  ( 0.9687793358424821033, -0.2479245821708677133, 0.000000000000000000 ) ) ;
#20595 = CARTESIAN_POINT ( 'NONE',  ( -13.43330777456016989, -9.058089930353723673, 60.43950223964813517 ) ) ;
#20596 = VERTEX_POINT ( 'NONE', #25496 ) ;
#20597 = EDGE_LOOP ( 'NONE', ( #18396, #30435, #33702, #36291 ) ) ;
#20598 = CARTESIAN_POINT ( 'NONE',  ( -21.99284385650551243, -7.406986770994973490, 48.81910596585309747 ) ) ;
#20599 = VECTOR ( 'NONE', #33482, 1000.000000000000114 ) ;
#20600 = CARTESIAN_POINT ( 'NONE',  ( -21.53861886228549949, -21.02004079589906027, 72.63951149839988375 ) ) ;
#20601 = CARTESIAN_POINT ( 'NONE',  ( -24.87377577156081898, -14.89435671199219335, 59.38266843862005828 ) ) ;
#20602 = CARTESIAN_POINT ( 'NONE',  ( -12.63240329231120995, -19.98054781565096505, 68.33657436980826105 ) ) ;
#20603 = CARTESIAN_POINT ( 'NONE',  ( -22.38659385650551670, -9.302874398569244363, 51.68646062012417985 ) ) ;
#20604 = EDGE_CURVE ( 'NONE', #16043, #7957, #46939, .T. ) ;
#20605 = ORIENTED_EDGE ( 'NONE', *, *, #6005, .F. ) ;
#20606 = ADVANCED_FACE ( 'NONE', ( #47910 ), #6306, .T. ) ;
#20607 = EDGE_CURVE ( 'NONE', #4739, #6094, #9531, .T. ) ;
#20608 = CARTESIAN_POINT ( 'NONE',  ( -12.32158608955787393, -9.943909642237139579, 60.57390139315987909 ) ) ;
#20609 = EDGE_CURVE ( 'NONE', #6656, #29328, #43504, .T. ) ;
#20610 = CARTESIAN_POINT ( 'NONE',  ( -17.42409385541300182, -14.80920654474440745, 54.28066884056654828 ) ) ;
#20611 = VECTOR ( 'NONE', #23760, 1000.000000000000000 ) ;
#20612 = CARTESIAN_POINT ( 'NONE',  ( -11.45099342332292025, -10.35672743380498062, 74.58885046824201481 ) ) ;
#20613 = ORIENTED_EDGE ( 'NONE', *, *, #5904, .T. ) ;
#20614 = DIRECTION ( 'NONE',  ( -7.484513356303811700E-07, 7.898531944235430371E-07, 0.9999999999994079181 ) ) ;
#20615 = DIRECTION ( 'NONE',  ( 0.5820088206811424580, -0.8131824719270214219, 7.019974882119937445E-08 ) ) ;
#20616 = CARTESIAN_POINT ( 'NONE',  ( -11.29385091374517458, -19.04286921470785288, 68.33194352083310719 ) ) ;
#20617 = CARTESIAN_POINT ( 'NONE',  ( -22.53655392111809164, -20.22829597721307948, 65.88917050827579658 ) ) ;
#20618 = ORIENTED_EDGE ( 'NONE', *, *, #8465, .T. ) ;
#20619 = B_SPLINE_CURVE_WITH_KNOTS ( 'NONE', 3,
 ( #48687, #26285, #40330, #10304, #21623, #48199, #32922, #14196, #40560, #14428 ),
 .UNSPECIFIED., .F., .F.,
 ( 4, 2, 2, 2, 4 ),
 ( 0.6272669072877824492, 0.7522669073072968393, 0.8772669073268113404, 1.002266907346325731, 1.127266907365840121 ),
 .UNSPECIFIED. ) ;
#20620 = DIRECTION ( 'NONE',  ( -0.3824554607245533866, 0.9239739285077093189, -8.917814418161381897E-09 ) ) ;
#20621 = CARTESIAN_POINT ( 'NONE',  ( -22.78930279417433624, -10.31314903132836136, 63.18071954302660487 ) ) ;
#20622 = CYLINDRICAL_SURFACE ( 'NONE', #40211, 5.249999999999998224 ) ;
#20623 = VERTEX_POINT ( 'NONE', #10490 ) ;
#20624 = CARTESIAN_POINT ( 'NONE',  ( -16.03410428664897225, -7.489899486381565552, 63.84823818164760212 ) ) ;
#20625 = ORIENTED_EDGE ( 'NONE', *, *, #44212, .T. ) ;
#20626 = DIRECTION ( 'NONE',  ( 1.000000000000000000, -4.164305804376849172E-17, 1.614929280266638808E-16 ) ) ;
#20627 = CARTESIAN_POINT ( 'NONE',  ( -9.983021216844335299, -14.44210324501309906, 68.03612869841425947 ) ) ;
#20628 = ORIENTED_EDGE ( 'NONE', *, *, #41243, .T. ) ;
#20629 = CARTESIAN_POINT ( 'NONE',  ( -22.16544622181183044, -20.55585424591192378, 58.88726014294076094 ) ) ;
#20631 = EDGE_CURVE ( 'NONE', #44357, #42725, #35466, .T. ) ;
#20630 = DIRECTION ( 'NONE',  ( 1.224646799147353207E-16, 1.000000000000000000, -1.912410701131276611E-32 ) ) ;
#20632 = CARTESIAN_POINT ( 'NONE',  ( -23.98984720795339243, -17.39877237835929691, 73.02768823732557735 ) ) ;
#20633 = FACE_OUTER_BOUND ( 'NONE', #27579, .T. ) ;
#20634 = ORIENTED_EDGE ( 'NONE', *, *, #34639, .F. ) ;
#20635 = CARTESIAN_POINT ( 'NONE',  ( -13.43773910423563400, -20.62433115109003268, 58.33177939114180788 ) ) ;
#20636 = CARTESIAN_POINT ( 'NONE',  ( -20.59780817978206002, -8.569521609192868539, 63.59504950924878131 ) ) ;
#20637 = CARTESIAN_POINT ( 'NONE',  ( -15.35027142736847239, -7.653576728715946409, 74.26480947788739684 ) ) ;
#20638 = ORIENTED_EDGE ( 'NONE', *, *, #38111, .F. ) ;
#20639 = CARTESIAN_POINT ( 'NONE',  ( -17.62313272718237300, -7.758403197964874209, 67.11219550178550719 ) ) ;
#20640 = FACE_OUTER_BOUND ( 'NONE', #24104, .T. ) ;
#20641 = ORIENTED_EDGE ( 'NONE', *, *, #25759, .T. ) ;
#20642 = ORIENTED_EDGE ( 'NONE', *, *, #33045, .F. ) ;
#20643 = CARTESIAN_POINT ( 'NONE',  ( -24.12000719736520438, -11.54295319193055214, 63.20864192093194589 ) ) ;
#20644 = CARTESIAN_POINT ( 'NONE',  ( -13.33011785382929126, -9.069340661520646663, 63.92418669539090814 ) ) ;
#20645 = EDGE_CURVE ( 'NONE', #16885, #44810, #33888, .T. ) ;
#20646 = DIRECTION ( 'NONE',  ( -0.3688590060343663324, 0.9294853595766526810, -1.901466464867638737E-17 ) ) ;
#20647 = CARTESIAN_POINT ( 'NONE',  ( -18.86784385650551954, -6.428312510596451368, 51.20221977374900035 ) ) ;
#20648 = DIRECTION ( 'NONE',  ( -0.2771212459065067191, 0.9608349572466771127, 4.100231986695772107E-08 ) ) ;
#20649 = CARTESIAN_POINT ( 'NONE',  ( -7.057530559158139205, -11.90597956881549102, 54.61912878955446615 ) ) ;
#20650 = DIRECTION ( 'NONE',  ( 0.7700094066334552956, 0.6380325334150243055, -6.510647142068464459E-17 ) ) ;
#20651 = CARTESIAN_POINT ( 'NONE',  ( -17.77594298899184366, -7.367433885636743618, 60.26556189360973548 ) ) ;
#20652 = ORIENTED_EDGE ( 'NONE', *, *, #28829, .T. ) ;
#20653 = ORIENTED_EDGE ( 'NONE', *, *, #47403, .T. ) ;
#20654 = CARTESIAN_POINT ( 'NONE',  ( -23.77487038158592014, -11.74745262826995429, 62.96690348473899235 ) ) ;
#20655 = DIRECTION ( 'NONE',  ( 0.000000000000000000, 0.000000000000000000, 1.000000000000000000 ) ) ;
#20656 = DIRECTION ( 'NONE',  ( 3.549360974554993999E-17, -6.371834667797928663E-18, -1.000000000000000000 ) ) ;
#20657 = CARTESIAN_POINT ( 'NONE',  ( -19.77435985551070274, -21.87886194922281646, 65.64981515446680760 ) ) ;
#20658 = CARTESIAN_POINT ( 'NONE',  ( -13.41559392277415341, -8.529421005230245711, 57.08472474434080368 ) ) ;
#20659 = DIRECTION ( 'NONE',  ( -2.210955089557150869E-06, 1.097707070272558804E-06, -0.9999999999969533260 ) ) ;
#20660 = VERTEX_POINT ( 'NONE', #13183 ) ;
#20661 = ADVANCED_FACE ( 'NONE', ( #5831 ), #5741, .T. ) ;
#20662 = EDGE_CURVE ( 'NONE', #45579, #13357, #39235, .T. ) ;
#20663 = CARTESIAN_POINT ( 'NONE',  ( -20.30052658356369477, -21.25444530744949390, 72.56046004230084634 ) ) ;
#20664 = CARTESIAN_POINT ( 'NONE',  ( -23.98641038275339099, -11.28202459292402082, 66.58247877162926898 ) ) ;
#20665 = CARTESIAN_POINT ( 'NONE',  ( -13.18904211892903078, -11.30002761096173813, 53.49999999999995026 ) ) ;
#20666 = CARTESIAN_POINT ( 'NONE',  ( -11.10470791607724550, -18.75498134223953883, 61.46206221440264983 ) ) ;
#20667 =( BOUNDED_CURVE ( )  B_SPLINE_CURVE ( 3, ( #26681, #42184, #8444, #23478 ),
 .UNSPECIFIED., .F., .F. ) 
 B_SPLINE_CURVE_WITH_KNOTS ( ( 4, 4 ),
 ( 0.5000000000000000000, 0.9074455897393587378 ),
 .UNSPECIFIED. ) 
 CURVE ( )  GEOMETRIC_REPRESENTATION_ITEM ( )  RATIONAL_B_SPLINE_CURVE ( ( 1.000000000000012657, 0.4567392136813444581, 0.3561768502900259925, 0.6983129098260709711 ) ) 
 REPRESENTATION_ITEM ( '' )  );
#20668 = VERTEX_POINT ( 'NONE', #9773 ) ;
#20669 = CARTESIAN_POINT ( 'NONE',  ( -12.18719842096713357, -10.08886484896570934, 64.04386393395434141 ) ) ;
#20670 = EDGE_CURVE ( 'NONE', #19987, #6217, #31184, .T. ) ;
#20671 = EDGE_CURVE ( 'NONE', #31941, #35848, #32415, .T. ) ;
#20672 = DIRECTION ( 'NONE',  ( -3.071710424422018668E-17, 6.404604876783312462E-16, 1.000000000000000000 ) ) ;
#20673 = CARTESIAN_POINT ( 'NONE',  ( -18.12574864353739201, -7.786197982121914052, 60.22493603095571046 ) ) ;
#20674 = ADVANCED_FACE ( 'NONE', ( #18089 ), #44236, .T. ) ;
#20675 = CARTESIAN_POINT ( 'NONE',  ( -10.13783977983156248, -13.25541127610578762, 74.79322348855123437 ) ) ;
#20676 = CARTESIAN_POINT ( 'NONE',  ( -16.77879762802476904, -7.785173775872046953, 74.16838186400050859 ) ) ;
#20677 = CARTESIAN_POINT ( 'NONE',  ( -18.90996118681096405, -7.968724231816139536, 67.20071784163268092 ) ) ;
#20678 = ORIENTED_EDGE ( 'NONE', *, *, #9747, .T. ) ;
#20679 = CARTESIAN_POINT ( 'NONE',  ( -23.66599411597432834, -18.87638235353465177, 69.48710309960380016 ) ) ;
#20680 =( BOUNDED_SURFACE ( )  B_SPLINE_SURFACE ( 3, 1, ( 
 ( #27068, #42093 ),
 ( #27794, #9590 ),
 ( #42823, #13489 ),
 ( #31739, #46992 ),
 ( #5882, #32227 ),
 ( #36139, #17175 ),
 ( #24606, #2173 ) ),
 .UNSPECIFIED., .T., .F., .F. ) 
 B_SPLINE_SURFACE_WITH_KNOTS ( ( 4, 3, 4 ),
 ( 2, 2 ),
 ( 0.000000000000000000, 0.5000000000000000000, 1.000000000000000000 ),
 ( 0.000000000000000000, 1.000000000000000000 ),
 .UNSPECIFIED. ) 
 GEOMETRIC_REPRESENTATION_ITEM ( )  RATIONAL_B_SPLINE_SURFACE ( (
 ( 1.000000000000000000, 1.000000000000000000),
 ( 0.3333333333333335369, 0.3333333333333330373),
 ( 0.3333333333333335369, 0.3333333333333330373),
 ( 1.000000000000000000, 1.000000000000000000),
 ( 0.3333333333333333703, 0.3333333333333333703),
 ( 0.3333333333333333703, 0.3333333333333333703),
 ( 1.000000000000000000, 1.000000000000000000) ) ) 
 REPRESENTATION_ITEM ( '' )  SURFACE ( )  );
#20681 = ORIENTED_EDGE ( 'NONE', *, *, #46908, .T. ) ;
#20682 = CARTESIAN_POINT ( 'NONE',  ( -11.33476867595667770, -19.10151316506851416, 68.40185013497388411 ) ) ;
#20683 = CARTESIAN_POINT ( 'NONE',  ( -10.42496409221358178, -14.69883174549087279, 71.32782692796889989 ) ) ;
#20684 = ORIENTED_EDGE ( 'NONE', *, *, #19431, .F. ) ;
#20685 = DIRECTION ( 'NONE',  ( -0.9999247414263406908, 0.01226831216845469807, 5.367905339378914507E-08 ) ) ;
#20686 = EDGE_CURVE ( 'NONE', #47586, #4886, #32746, .T. ) ;
#20687 = CARTESIAN_POINT ( 'NONE',  ( -11.42544933137708263, -10.39099551632332563, 74.56072225344634319 ) ) ;
#20688 = ORIENTED_EDGE ( 'NONE', *, *, #38500, .T. ) ;
#20689 = CARTESIAN_POINT ( 'NONE',  ( -13.56815751001608916, -20.71130982922042207, 61.81646292535575071 ) ) ;
#20690 = CARTESIAN_POINT ( 'NONE',  ( -10.61641583932764910, -11.78277314028518319, 74.74335662173743344 ) ) ;
#20691 = CARTESIAN_POINT ( 'NONE',  ( -16.05981277502693416, -21.73406819447767901, 61.90001277639490951 ) ) ;
#20692 = ORIENTED_EDGE ( 'NONE', *, *, #35709, .F. ) ;
#20693 = CARTESIAN_POINT ( 'NONE',  ( -23.83833616213321704, -17.61232902345998141, 62.77360984984811410 ) ) ;
#20694 = CARTESIAN_POINT ( 'NONE',  ( -10.49912617938483628, -17.55847672437320028, 64.74084113084838066 ) ) ;
#20695 = CARTESIAN_POINT ( 'NONE',  ( -20.57278697373333998, -8.057206101692887756, 66.89608655064280640 ) ) ;
#20696 = CARTESIAN_POINT ( 'NONE',  ( -23.34092642400682038, -10.28208056094584677, 59.78698708435513254 ) ) ;
#20697 = VECTOR ( 'NONE', #25458, 1000.000000000000000 ) ;
#20698 = VERTEX_POINT ( 'NONE', #11697 ) ;
#20699 = ORIENTED_EDGE ( 'NONE', *, *, #37931, .F. ) ;
#20700 = CARTESIAN_POINT ( 'NONE',  ( -27.42409385541305156, -14.65920654474411045, 48.99999999999997868 ) ) ;
#20701 = CARTESIAN_POINT ( 'NONE',  ( -14.80056147340629380, -21.78207226143426922, 61.82095877133116346 ) ) ;
#20702 = ORIENTED_EDGE ( 'NONE', *, *, #40228, .F. ) ;
#20703 = CARTESIAN_POINT ( 'NONE',  ( -19.33968306427223638, -21.54245604374635548, 62.27887115452926992 ) ) ;
#20704 = CARTESIAN_POINT ( 'NONE',  ( -19.12409385759799108, -9.359200813967568422, 50.49621490985803263 ) ) ;
#20705 = CARTESIAN_POINT ( 'NONE',  ( -13.18474066807476675, -20.93551553819402855, 58.23145462665691241 ) ) ;
#20706 = DIRECTION ( 'NONE',  ( 3.549360974551883545E-17, -6.371834667872732552E-18, -1.000000000000000000 ) ) ;
#20707 = EDGE_LOOP ( 'NONE', ( #23380, #17786, #34884, #26896, #44671 ) ) ;
#20708 = CARTESIAN_POINT ( 'NONE',  ( -22.61838138049972358, -19.58773617554900071, 69.32985287095068827 ) ) ;
#20709 = CARTESIAN_POINT ( 'NONE',  ( 23.52590614458706852, 1.890747609047893185, 50.53028072113869484 ) ) ;
#20710 = CARTESIAN_POINT ( 'NONE',  ( -23.16908677366360436, -10.06487111558154801, 63.18530634343710517 ) ) ;
#20711 = CARTESIAN_POINT ( 'NONE',  ( -24.87450840884172365, -14.73858704721042123, 59.35644987740099765 ) ) ;
#20712 = DIRECTION ( 'NONE',  ( -3.071710424422018668E-17, 6.404604876783312462E-16, 1.000000000000000000 ) ) ;
#20713 = EDGE_LOOP ( 'NONE', ( #9821, #6555, #16863, #44016 ) ) ;
#20714 = ORIENTED_EDGE ( 'NONE', *, *, #15735, .T. ) ;
#20715 = EDGE_LOOP ( 'NONE', ( #866, #30290 ) ) ;
#20716 = EDGE_CURVE ( 'NONE', #43113, #26442, #2767, .T. ) ;
#20717 = CARTESIAN_POINT ( 'NONE',  ( -17.63866143434000833, -7.362211242860705163, 63.66561706598076853 ) ) ;
#20718 = CARTESIAN_POINT ( 'NONE',  ( -23.63337334774834275, -11.57735749097352773, 63.14321518547134815 ) ) ;
#20719 = CARTESIAN_POINT ( 'NONE',  ( -10.97170681910752421, -18.53336975224134520, 57.90740351038629541 ) ) ;
#20720 = EDGE_LOOP ( 'NONE', ( #24715, #29909, #6642, #48730, #31383 ) ) ;
#20721 = CARTESIAN_POINT ( 'NONE',  ( -12.40380833417894912, -19.68739609921301792, 61.39678633575574906 ) ) ;
#20722 = EDGE_CURVE ( 'NONE', #467, #35820, #36230, .T. ) ;
#20723 = DIRECTION ( 'NONE',  ( 0.9950649908465212246, 0.09922531930717197468, -4.894557009475175470E-08 ) ) ;
#20724 = VECTOR ( 'NONE', #25877, 1000.000000000000114 ) ;
#20725 = VERTEX_POINT ( 'NONE', #3830 ) ;
#20726 = ADVANCED_FACE ( 'NONE', ( #41744 ), #14868, .T. ) ;
#20727 = FACE_OUTER_BOUND ( 'NONE', #19698, .T. ) ;
#20728 = CARTESIAN_POINT ( 'NONE',  ( -24.72409385541305582, -14.80920654474421205, 67.95882352941174531 ) ) ;
#20729 = ADVANCED_FACE ( 'NONE', ( #380 ), #11448, .T. ) ;
#20730 = ORIENTED_EDGE ( 'NONE', *, *, #18036, .F. ) ;
#20731 = CARTESIAN_POINT ( 'NONE',  ( -11.73260704738458671, -10.00184175524024610, 67.61401452035728710 ) ) ;
#20732 = ORIENTED_EDGE ( 'NONE', *, *, #43106, .F. ) ;
#20733 = CARTESIAN_POINT ( 'NONE',  ( -10.54994933093899867, -13.24305344519376781, 71.49356453765415154 ) ) ;
#20734 = ORIENTED_EDGE ( 'NONE', *, *, #31880, .F. ) ;
#20735 = CARTESIAN_POINT ( 'NONE',  ( -24.87417209744295477, -14.81009202510037959, 59.28654333241698993 ) ) ;
#20736 = DIRECTION ( 'NONE',  ( -0.9687793358424819923, 0.2479245821708680464, 0.000000000000000000 ) ) ;
#20737 = CARTESIAN_POINT ( 'NONE',  ( -19.37462041217285957, -21.99941596162432589, 58.56861435762115775 ) ) ;
#20738 = ORIENTED_EDGE ( 'NONE', *, *, #1271, .T. ) ;
#20739 = CARTESIAN_POINT ( 'NONE',  ( -24.70006301780203017, -16.41064289384416242, 59.24519641474478959 ) ) ;
#20740 = FACE_OUTER_BOUND ( 'NONE', #39778, .T. ) ;
#20741 = CARTESIAN_POINT ( 'NONE',  ( -11.16720114480400383, -11.56054632708127450, 67.61864607954859707 ) ) ;
#20742 = CARTESIAN_POINT ( 'NONE',  ( -23.56138462120852495, -11.33988936615837950, 70.04210750373424332 ) ) ;
#20743 = DIRECTION ( 'NONE',  ( -0.3478314405900309603, -0.9375570856950864451, 9.567072274253697654E-17 ) ) ;
#20744 = ORIENTED_EDGE ( 'NONE', *, *, #5878, .F. ) ;
#20745 = DIRECTION ( 'NONE',  ( 1.653275065793327654E-06, -1.135554159585744654E-05, -0.9999999999341592227 ) ) ;
#20746 = CARTESIAN_POINT ( 'NONE',  ( -24.09792889798371007, -17.08130376423426000, 73.18336032035891492 ) ) ;
#20747 = CARTESIAN_POINT ( 'NONE',  ( -12.18836193727821460, -19.53083876418623532, 57.94154444592973618 ) ) ;
#20748 = LINE ( 'NONE', #13576, #39374 ) ;
#20749 = CARTESIAN_POINT ( 'NONE',  ( -15.04284385650551670, -8.811426318492348031, 52.18089403414752070 ) ) ;
#20750 = PRODUCT_RELATED_PRODUCT_CATEGORY ( 'part', '', ( #33418 ) ) ;
#20751 = VERTEX_POINT ( 'NONE', #7530 ) ;
#20752 = DIRECTION ( 'NONE',  ( -0.000000000000000000, -1.000000000000000000, 0.000000000000000000 ) ) ;
#20753 = CARTESIAN_POINT ( 'NONE',  ( -15.07409385759798859, -6.859212275519751323, 50.50378509014259265 ) ) ;
#20754 = ORIENTED_EDGE ( 'NONE', *, *, #9221, .F. ) ;
#20755 = CYLINDRICAL_SURFACE ( 'NONE', #44979, 0.1499999999999962474 ) ;
#20756 = CARTESIAN_POINT ( 'NONE',  ( -13.29845767883066543, -21.01266560759323809, 61.63150935275904629 ) ) ;
#20757 = CARTESIAN_POINT ( 'NONE',  ( -12.68532353738824803, -9.060482037740600347, 71.03420644255490402 ) ) ;
#20758 = CARTESIAN_POINT ( 'NONE',  ( -18.75534385541303806, -8.623186033802571870, 49.24843789510465797 ) ) ;
#20759 = CARTESIAN_POINT ( 'NONE',  ( -10.44911129250985482, -12.18941988514178121, 57.51512593431250764 ) ) ;
#20760 = ORIENTED_EDGE ( 'NONE', *, *, #29449, .T. ) ;
#20761 = CARTESIAN_POINT ( 'NONE',  ( -24.80964181269326829, -15.78832295113944895, 69.67160939887251914 ) ) ;
#20762 = CARTESIAN_POINT ( 'NONE',  ( -50.42609385541305755, -14.80920654474426534, 72.08823529411763786 ) ) ;
#20763 = AXIS2_PLACEMENT_3D ( 'NONE', #12213, #4835, #19605 ) ;
#20764 = CARTESIAN_POINT ( 'NONE',  ( -23.23616516995063819, -18.79948553760870666, 65.97389430042666447 ) ) ;
#20765 = EDGE_LOOP ( 'NONE', ( #24627, #12456, #42147, #46351, #5951 ) ) ;
#20766 = AXIS2_PLACEMENT_3D ( 'NONE', #8050, #34349, #635 ) ;
#20767 = CARTESIAN_POINT ( 'NONE',  ( -16.23116076413911557, -7.455249184188991407, 60.31533086125586607 ) ) ;
#20768 = CARTESIAN_POINT ( 'NONE',  ( -18.57335281209669731, -21.76520412651811043, 72.57038810541313012 ) ) ;
#20769 = CARTESIAN_POINT ( 'NONE',  ( -24.40290088483126851, -17.41666877191872587, 69.61350989034804115 ) ) ;
#20770 = CARTESIAN_POINT ( 'NONE',  ( -21.15336808330806662, -20.73310000539657949, 69.35450185099439580 ) ) ;
#20771 = B_SPLINE_CURVE_WITH_KNOTS ( 'NONE', 1,
 ( #3744, #45130 ),
 .UNSPECIFIED., .F., .F.,
 ( 2, 2 ),
 ( 0.000000000000000000, 1.000000000000000000 ),
 .UNSPECIFIED. ) ;
#20772 = EDGE_CURVE ( 'NONE', #37849, #1571, #17361, .T. ) ;
#20773 = CARTESIAN_POINT ( 'NONE',  ( -11.16823349194678627, -11.55205338407005122, 71.50349565124497531 ) ) ;
#20774 = DIRECTION ( 'NONE',  ( -3.071710424422018668E-17, 6.404604876783312462E-16, 1.000000000000000000 ) ) ;
#20775 = ORIENTED_EDGE ( 'NONE', *, *, #34557, .T. ) ;
#20776 = EDGE_LOOP ( 'NONE', ( #40260, #12251, #41633, #43540, #20290 ) ) ;
#20777 = CARTESIAN_POINT ( 'NONE',  ( -18.08034385541304445, -9.360768649639302552, 51.01397948905922419 ) ) ;
#20778 = CARTESIAN_POINT ( 'NONE',  ( -10.37518579106875194, -14.94145004404884602, 75.09219096253774239 ) ) ;
#20779 = CARTESIAN_POINT ( 'NONE',  ( -17.79084007069931417, -7.768752218527304798, 60.38060768310334936 ) ) ;
#20780 = CARTESIAN_POINT ( 'NONE',  ( -19.74436319619195501, -10.72363366794506412, 49.52966884056655772 ) ) ;
#20781 = DIRECTION ( 'NONE',  ( 0.000000000000000000, -1.000000000000000000, 0.000000000000000000 ) ) ;
#20782 = VERTEX_POINT ( 'NONE', #33341 ) ;
#20783 = ADVANCED_FACE ( 'NONE', ( #37790 ), #14376, .T. ) ;
#20784 = DIRECTION ( 'NONE',  ( 3.071710424422018668E-17, -6.404604876783312462E-16, -1.000000000000000000 ) ) ;
#20785 = CARTESIAN_POINT ( 'NONE',  ( -18.05440415122280484, -21.83127237841607027, 65.36004252941745563 ) ) ;
#20786 = EDGE_CURVE ( 'NONE', #16929, #39540, #42778, .T. ) ;
#20787 = ORIENTED_EDGE ( 'NONE', *, *, #17680, .F. ) ;
#20788 = CYLINDRICAL_SURFACE ( 'NONE', #15490, 0.1500000000000041578 ) ;
#20789 = CARTESIAN_POINT ( 'NONE',  ( -17.00708550189658652, -7.821638742870105965, 73.96018273346899718 ) ) ;
#20790 = VECTOR ( 'NONE', #43428, 1000.000000000000000 ) ;
#20791 = EDGE_LOOP ( 'NONE', ( #25080, #18488, #24302, #5570, #23092 ) ) ;
#20792 = EDGE_CURVE ( 'NONE', #15544, #22481, #23006, .T. ) ;
#20793 = CARTESIAN_POINT ( 'NONE',  ( -20.92409385541305511, -10.60920654474410618, 79.49999999999998579 ) ) ;
#20794 = CARTESIAN_POINT ( 'NONE',  ( -18.50162525266306091, -21.72577549820248421, 72.58510940979837756 ) ) ;
#20795 = EDGE_LOOP ( 'NONE', ( #46018, #21923 ) ) ;
#20796 = CARTESIAN_POINT ( 'NONE',  ( -10.52215041504658188, -13.37196039468857833, 74.97817647370040106 ) ) ;
#20797 = CIRCLE ( 'NONE', #4283, 3.982850737850970990 ) ;
#20798 = CARTESIAN_POINT ( 'NONE',  ( -20.02409385759798965, -9.359200813967568422, 50.49621490985803263 ) ) ;
#20799 = EDGE_CURVE ( 'NONE', #4399, #34284, #36197, .T. ) ;
#20800 =( BOUNDED_CURVE ( )  B_SPLINE_CURVE ( 3, ( #34195, #12051, #48733, #37391 ),
 .UNSPECIFIED., .F., .F. ) 
 B_SPLINE_CURVE_WITH_KNOTS ( ( 4, 4 ),
 ( 0.9074455897393668424, 1.000000000000000000 ),
 .UNSPECIFIED. ) 
 CURVE ( )  GEOMETRIC_REPRESENTATION_ITEM ( )  RATIONAL_B_SPLINE_CURVE ( ( 0.6983129098260865142, 0.7760317562606925401, 0.8765941196519970724, 1.000000000000000000 ) ) 
 REPRESENTATION_ITEM ( '' )  );
#20801 = DIRECTION ( 'NONE',  ( 0.000000000000000000, 0.000000000000000000, -1.000000000000000000 ) ) ;
#20802 = CARTESIAN_POINT ( 'NONE',  ( -11.06300712566464561, -17.73109164226346479, 71.58220677401085652 ) ) ;
#20803 = VERTEX_POINT ( 'NONE', #26725 ) ;
#20804 = CARTESIAN_POINT ( 'NONE',  ( -50.42609385541305755, -14.90920654474423301, 69.07058823529411029 ) ) ;
#20805 = CARTESIAN_POINT ( 'NONE',  ( -17.03658212107600889, -14.90837637761275403, 53.27966884056655061 ) ) ;
#20806 = ADVANCED_FACE ( 'NONE', ( #3569 ), #15781, .T. ) ;
#20807 = CARTESIAN_POINT ( 'NONE',  ( -12.75531685953890282, -14.40201664703461049, 49.52966884056655772 ) ) ;
#20808 = FACE_OUTER_BOUND ( 'NONE', #5019, .T. ) ;
#20809 = CARTESIAN_POINT ( 'NONE',  ( -20.25445156252866497, -7.916983464207429932, 73.90751836168473687 ) ) ;
#20810 = CARTESIAN_POINT ( 'NONE',  ( -11.40127056704611519, -11.24191079892443135, 60.67885781060143557 ) ) ;
#20811 = FACE_OUTER_BOUND ( 'NONE', #5634, .T. ) ;
#20812 = ORIENTED_EDGE ( 'NONE', *, *, #40893, .F. ) ;
#20813 = CARTESIAN_POINT ( 'NONE',  ( -24.35031885046671007, -17.55372768567562858, 66.08210759853170657 ) ) ;
#20814 = FACE_OUTER_BOUND ( 'NONE', #4647, .T. ) ;
#20815 = DIRECTION ( 'NONE',  ( 0.9687793358424819923, -0.2479245821708676023, 0.000000000000000000 ) ) ;
#20816 = ORIENTED_EDGE ( 'NONE', *, *, #24191, .F. ) ;
#20817 = B_SPLINE_CURVE_WITH_KNOTS ( 'NONE', 3,
 ( #37853, #19386, #19142, #922, #41303, #41807, #11277, #11765, #45981, #27019 ),
 .UNSPECIFIED., .F., .F.,
 ( 4, 2, 2, 2, 4 ),
 ( 0.000000000000000000, 0.2500000000000000000, 0.5000000000000000000, 0.7500000000000000000, 1.000000000000000000 ),
 .UNSPECIFIED. ) ;
#20818 =( BOUNDED_SURFACE ( )  B_SPLINE_SURFACE ( 3, 1, ( 
 ( #47457, #2628 ),
 ( #37073, #44257 ),
 ( #3355, #18361 ),
 ( #13925, #28971 ),
 ( #44020, #25290 ),
 ( #40305, #10513 ),
 ( #6810, #21827 ) ),
 .UNSPECIFIED., .T., .F., .F. ) 
 B_SPLINE_SURFACE_WITH_KNOTS ( ( 4, 3, 4 ),
 ( 2, 2 ),
 ( 0.000000000000000000, 0.5000000000000000000, 1.000000000000000000 ),
 ( 0.000000000000000000, 1.000000000000000000 ),
 .UNSPECIFIED. ) 
 GEOMETRIC_REPRESENTATION_ITEM ( )  RATIONAL_B_SPLINE_SURFACE ( (
 ( 1.000000000000000000, 1.000000000000000000),
 ( 0.3333333333333335369, 0.3333333333333330373),
 ( 0.3333333333333335369, 0.3333333333333330373),
 ( 1.000000000000000000, 1.000000000000000000),
 ( 0.3333333333333333703, 0.3333333333333333703),
 ( 0.3333333333333333703, 0.3333333333333333703),
 ( 1.000000000000000000, 1.000000000000000000) ) ) 
 REPRESENTATION_ITEM ( '' )  SURFACE ( )  );
#20819 = DIRECTION ( 'NONE',  ( 0.9687793358424817702, -0.2479245821708686570, 0.000000000000000000 ) ) ;
#20820 = ORIENTED_EDGE ( 'NONE', *, *, #20792, .F. ) ;
#20821 = ORIENTED_EDGE ( 'NONE', *, *, #20947, .T. ) ;
#20822 = ORIENTED_EDGE ( 'NONE', *, *, #41461, .T. ) ;
#20823 = DIRECTION ( 'NONE',  ( 0.8447509909909772796, -0.5351595679979587183, 5.460905094113815840E-17 ) ) ;
#20824 = DIRECTION ( 'NONE',  ( 7.404863042181874502E-06, -6.320720312887485007E-06, 0.9999999999526082428 ) ) ;
#20825 = ADVANCED_FACE ( 'NONE', ( #35307 ), #31471, .T. ) ;
#20826 = DIRECTION ( 'NONE',  ( -0.1240347345892086062, 1.145860353393066553E-16, -0.9922778767136676281 ) ) ;
#20827 = CARTESIAN_POINT ( 'NONE',  ( -19.84060376186859287, -21.38033729433684726, 72.48922594225743410 ) ) ;
#20828 = CARTESIAN_POINT ( 'NONE',  ( -16.28340391395008169, -22.17153211024223936, 61.89534802377870193 ) ) ;
#20829 =( BOUNDED_CURVE ( )  B_SPLINE_CURVE ( 3, ( #46600, #38948, #27632, #30860 ),
 .UNSPECIFIED., .F., .F. ) 
 B_SPLINE_CURVE_WITH_KNOTS ( ( 4, 4 ),
 ( 0.9074455897393733927, 1.000000000000000000 ),
 .UNSPECIFIED. ) 
 CURVE ( )  GEOMETRIC_REPRESENTATION_ITEM ( )  RATIONAL_B_SPLINE_CURVE ( ( 0.6983129098261244838, 0.7760317562607252917, 0.8765941196520171674, 1.000000000000000000 ) ) 
 REPRESENTATION_ITEM ( '' )  );
#20830 = VERTEX_POINT ( 'NONE', #19322 ) ;
#20831 = ORIENTED_EDGE ( 'NONE', *, *, #23521, .T. ) ;
#20832 = TOROIDAL_SURFACE ( 'NONE', #48330, 1.350000000000000311, 0.1000000000000000056 ) ;
#20833 = CARTESIAN_POINT ( 'NONE',  ( -17.38034385650551528, -6.424090610841176385, 49.80797279389977916 ) ) ;
#20834 = CIRCLE ( 'NONE', #40469, 2.000000000000001776 ) ;
#20835 = CARTESIAN_POINT ( 'NONE',  ( -24.87396285843436772, -14.85457912869396324, 59.44311433200221018 ) ) ;
#20836 = CARTESIAN_POINT ( 'NONE',  ( -24.09304468200822669, -16.93663518450954086, 73.11009419552426891 ) ) ;
#20837 = CARTESIAN_POINT ( 'NONE',  ( -21.03659385650551528, -6.915538690918074494, 49.31353937987644542 ) ) ;
#20838 = ADVANCED_FACE ( 'NONE', ( #1582 ), #46410, .F. ) ;
#20839 = ORIENTED_EDGE ( 'NONE', *, *, #16695, .F. ) ;
#20840 = CARTESIAN_POINT ( 'NONE',  ( -18.92057629138644970, -7.919864069981281673, 67.05071783789199458 ) ) ;
#20841 = CARTESIAN_POINT ( 'NONE',  ( -9.974215857974789046, -14.86484893678357544, 74.91283499353951925 ) ) ;
#20842 = CARTESIAN_POINT ( 'NONE',  ( -24.87424609913982110, -14.79435799483268177, 59.38153755231025599 ) ) ;
#20843 = EDGE_LOOP ( 'NONE', ( #46089, #24264, #8556, #7395 ) ) ;
#20844 = CARTESIAN_POINT ( 'NONE',  ( -11.75774095458083046, -19.00383931511212765, 71.68685884783835149 ) ) ;
#20845 = EDGE_CURVE ( 'NONE', #6404, #23831, #28011, .T. ) ;
#20846 = CARTESIAN_POINT ( 'NONE',  ( -27.42409385541305511, -15.80920654474410725, 48.99999999999997868 ) ) ;
#20847 = DIRECTION ( 'NONE',  ( 1.000000000000000000, 2.866981220435666553E-17, 0.000000000000000000 ) ) ;
#20848 = EDGE_CURVE ( 'NONE', #9159, #501, #19741, .T. ) ;
#20849 = ORIENTED_EDGE ( 'NONE', *, *, #10906, .F. ) ;
#20850 = CARTESIAN_POINT ( 'NONE',  ( -19.37484727228654080, -7.619050864103940057, 60.14588289477547534 ) ) ;
#20851 = EDGE_CURVE ( 'NONE', #47684, #25517, #19530, .T. ) ;
#20852 = CARTESIAN_POINT ( 'NONE',  ( -11.75743953354532856, -10.61491319464748351, 74.73885004197741466 ) ) ;
#20853 = CARTESIAN_POINT ( 'NONE',  ( -17.96469515596628597, -21.78991216099736405, 65.45605247325242715 ) ) ;
#20854 = EDGE_LOOP ( 'NONE', ( #30580, #40606, #36536, #16125, #38028, #11223 ) ) ;
#20855 = CARTESIAN_POINT ( 'NONE',  ( -22.09234551867295693, -20.09219114410425178, 62.53439162497838311 ) ) ;
#20856 = EDGE_LOOP ( 'NONE', ( #45256, #21912, #33586, #6013, #15506 ) ) ;
#20857 = VECTOR ( 'NONE', #9513, 1000.000000000000227 ) ;
#20858 = CARTESIAN_POINT ( 'NONE',  ( -11.81178328723415660, -10.62567094834893311, 74.73885052262691886 ) ) ;
#20859 = CARTESIAN_POINT ( 'NONE',  ( -16.26648990220133228, -21.71412262074107247, 61.82738493259662249 ) ) ;
#20860 = EDGE_LOOP ( 'NONE', ( #37979, #3133, #35707, #35010 ) ) ;
#20861 = CARTESIAN_POINT ( 'NONE',  ( -23.96075635701088657, -17.45014263229036899, 66.09357239682297802 ) ) ;
#20862 = CARTESIAN_POINT ( 'NONE',  ( -19.86401518824997581, -21.42384811948916479, 69.22010401872219632 ) ) ;
#20863 = AXIS2_PLACEMENT_3D ( 'NONE', #11360, #40904, #29583 ) ;
#20864 = CARTESIAN_POINT ( 'NONE',  ( -24.11881394502254849, -17.01995806294775448, 73.16863963025599560 ) ) ;
#20865 = CARTESIAN_POINT ( 'NONE',  ( -22.71955324316818547, -10.22924783853478559, 70.08348758896158870 ) ) ;
#20866 = ORIENTED_EDGE ( 'NONE', *, *, #12541, .F. ) ;
#20867 = FACE_OUTER_BOUND ( 'NONE', #29799, .T. ) ;
#20868 = CARTESIAN_POINT ( 'NONE',  ( -16.81162750399036909, -21.83617793957379050, 65.43384172164481072 ) ) ;
#20870 = EDGE_CURVE ( 'NONE', #4167, #39713, #24585, .T. ) ;
#20869 = CARTESIAN_POINT ( 'NONE',  ( -10.06841751317020872, -15.99566775706410482, 68.16423218926057359 ) ) ;
#20871 = B_SPLINE_CURVE_WITH_KNOTS ( 'NONE', 3,
 ( #35824, #40028, #21322, #9753, #43979, #24770, #46689, #27962, #21558, #40270 ),
 .UNSPECIFIED., .F., .F.,
 ( 4, 2, 2, 2, 4 ),
 ( 0.1272669073657797523, 0.2522669073488085223, 0.3772669073318372090, 0.5022669073148660068, 0.6272669072978946936 ),
 .UNSPECIFIED. ) ;
#20872 = ORIENTED_EDGE ( 'NONE', *, *, #16103, .F. ) ;
#20873 = CARTESIAN_POINT ( 'NONE',  ( -11.46028008028683942, -18.56947564720590194, 61.56238700194530367 ) ) ;
#20874 = EDGE_CURVE ( 'NONE', #4687, #34669, #34577, .T. ) ;
#20875 = CARTESIAN_POINT ( 'NONE',  ( -11.96084906401204506, -9.743958800322932490, 60.74413413563605957 ) ) ;
#20876 = ADVANCED_FACE ( 'NONE', ( #8749 ), #19249, .T. ) ;
#20877 = ADVANCED_FACE ( 'NONE', ( #2309 ), #25210, .T. ) ;
#20878 = VERTEX_POINT ( 'NONE', #2067 ) ;
#20879 = ORIENTED_EDGE ( 'NONE', *, *, #35791, .F. ) ;
#20880 = CARTESIAN_POINT ( 'NONE',  ( -14.88644031773417531, -21.33303323181352340, 58.35721170509270905 ) ) ;
#20881 = CARTESIAN_POINT ( 'NONE',  ( -17.42409385541299471, -14.80920654474435594, 52.02966884056656482 ) ) ;
#20882 = CARTESIAN_POINT ( 'NONE',  ( -11.34006216982616166, -11.24017310230250111, 57.41722930122209334 ) ) ;
#20883 = CARTESIAN_POINT ( 'NONE',  ( -17.40534385650551741, -8.801233750844183135, 48.81488406609782515 ) ) ;
#20884 = CARTESIAN_POINT ( 'NONE',  ( 18.57590614458706924, 0.6299963676414210845, 50.77646420411990391 ) ) ;
#20885 = CARTESIAN_POINT ( 'NONE',  ( -24.12651600458584511, -12.62191667979047338, 73.25697658996379857 ) ) ;
#20886 = CARTESIAN_POINT ( 'NONE',  ( -12.32149116705671332, -19.60131283701424820, 57.94184834235668546 ) ) ;
#20887 = FACE_OUTER_BOUND ( 'NONE', #20585, .T. ) ;
#20888 = CARTESIAN_POINT ( 'NONE',  ( -16.77581700079705485, -22.23100064957188593, 68.88834796384273318 ) ) ;
#20889 = ORIENTED_EDGE ( 'NONE', *, *, #32580, .F. ) ;
#20890 = VERTEX_POINT ( 'NONE', #13617 ) ;
#20891 = FACE_OUTER_BOUND ( 'NONE', #36589, .T. ) ;
#20892 = DIRECTION ( 'NONE',  ( 0.000000000000000000, 0.000000000000000000, 1.000000000000000000 ) ) ;
#20893 = CARTESIAN_POINT ( 'NONE',  ( -17.83128375312269753, -10.14042954887025871, 52.02966884056656482 ) ) ;
#20894 = CARTESIAN_POINT ( 'NONE',  ( -16.03289653659843594, -7.947204529361793668, 67.25080481985611414 ) ) ;
#20895 = CARTESIAN_POINT ( 'NONE',  ( -13.54792730259346456, -8.920061342218058797, 57.25495614889487683 ) ) ;
#20896 = CARTESIAN_POINT ( 'NONE',  ( 8.575906144586953772, -0.1092432217106413528, 50.52422457691089619 ) ) ;
#20897 = CARTESIAN_POINT ( 'NONE',  ( -20.30052658356369477, -21.25444530744949390, 72.56046004230084634 ) ) ;
#20898 = AXIS2_PLACEMENT_3D ( 'NONE', #38190, #31067, #46086 ) ;
#20899 = ORIENTED_EDGE ( 'NONE', *, *, #41673, .F. ) ;
#20900 = EDGE_CURVE ( 'NONE', #2612, #33183, #16271, .T. ) ;
#20901 = DIRECTION ( 'NONE',  ( 1.927470528863183637E-16, 1.434740771370715221E-29, -1.000000000000000000 ) ) ;
#20902 = CARTESIAN_POINT ( 'NONE',  ( -24.42218830102925509, -14.64588410380239480, 62.71296487252168816 ) ) ;
#20903 = CARTESIAN_POINT ( 'NONE',  ( -11.17855889551124982, -18.87086522978130532, 64.86211687253867808 ) ) ;
#20904 = ORIENTED_EDGE ( 'NONE', *, *, #45803, .F. ) ;
#20905 = CARTESIAN_POINT ( 'NONE',  ( -11.14016733508048240, -18.81244675540447631, 64.93362470803228348 ) ) ;
#20906 = EDGE_CURVE ( 'NONE', #18272, #1731, #34627, .T. ) ;
#20907 = CARTESIAN_POINT ( 'NONE',  ( -22.23733827145997566, -19.96043728507621040, 65.70421731380814379 ) ) ;
#20908 = CARTESIAN_POINT ( 'NONE',  ( -17.77754172124238963, -7.367517167730140315, 60.12414849856542531 ) ) ;
#20909 = EDGE_CURVE ( 'NONE', #20596, #42703, #20455, .T. ) ;
#20910 = DIRECTION ( 'NONE',  ( 0.1847813031241905823, -0.9827796650397888634, 7.910442904995644076E-08 ) ) ;
#20911 = CARTESIAN_POINT ( 'NONE',  ( -18.85724798917316392, -7.906108138700305155, 67.18599644112759961 ) ) ;
#20912 = CARTESIAN_POINT ( 'NONE',  ( -11.10758613922248905, -10.85889423684567490, 57.31564880789826333 ) ) ;
#20913 = DIRECTION ( 'NONE',  ( -8.766499794606700203E-07, -3.805972782304116817E-07, 0.9999999999995433653 ) ) ;
#20914 = VERTEX_POINT ( 'NONE', #47135 ) ;
#20915 = CARTESIAN_POINT ( 'NONE',  ( -23.04636716567627275, -18.97944391780718121, 58.95698644230029117 ) ) ;
#20916 = ORIENTED_EDGE ( 'NONE', *, *, #9026, .F. ) ;
#20917 = CARTESIAN_POINT ( 'NONE',  ( -22.27077318787935667, -19.92919612165446708, 65.99861962659834091 ) ) ;
#20918 = CARTESIAN_POINT ( 'NONE',  ( -14.73659385759798823, -8.995762431863214559, 51.38120296130585274 ) ) ;
#20919 = ORIENTED_EDGE ( 'NONE', *, *, #40108, .T. ) ;
#20920 = CARTESIAN_POINT ( 'NONE',  ( -13.65110067086344792, -21.23324738024127356, 68.57129742521463811 ) ) ;
#20921 = CARTESIAN_POINT ( 'NONE',  ( -13.61159385650551457, -6.922745924619793101, 51.69366785382590024 ) ) ;
#20922 = ORIENTED_EDGE ( 'NONE', *, *, #18323, .F. ) ;
#20923 = CARTESIAN_POINT ( 'NONE',  ( -11.97955794321693190, -10.40884752579252037, 71.25276566430856917 ) ) ;
#20924 = CARTESIAN_POINT ( 'NONE',  ( -14.86627003481517839, -7.811970263561289762, 56.96504677300865893 ) ) ;
#20925 = B_SPLINE_CURVE_WITH_KNOTS ( 'NONE', 3,
 ( #4382, #41318, #23110, #18410, #18654, #22875, #41082, #7855, #37869, #4157 ),
 .UNSPECIFIED., .F., .F.,
 ( 4, 2, 2, 2, 4 ),
 ( 0.000000000000000000, 0.2500000000000000000, 0.5000000000000000000, 0.7500000000000000000, 1.000000000000000000 ),
 .UNSPECIFIED. ) ;
#20926 = CARTESIAN_POINT ( 'NONE',  ( -19.25408589567127038, -10.49476435801948071, 49.52966884056655772 ) ) ;
#20927 = ORIENTED_EDGE ( 'NONE', *, *, #46819, .T. ) ;
#20928 = DIRECTION ( 'NONE',  ( -0.3109111061729914471, -0.9504389954427826526, -3.354176643444200258E-08 ) ) ;
#20929 = VECTOR ( 'NONE', #13026, 1000.000000000000000 ) ;
#20930 = CARTESIAN_POINT ( 'NONE',  ( -10.68551981713787136, -12.73596763222149164, 64.28308208171728211 ) ) ;
#20931 = VECTOR ( 'NONE', #43379, 1000.000000000000114 ) ;
#20932 = CARTESIAN_POINT ( 'NONE',  ( -24.59330981698489538, -12.78255162097813447, 66.44100198564684945 ) ) ;
#20933 = FACE_OUTER_BOUND ( 'NONE', #14598, .T. ) ;
#20934 = EDGE_CURVE ( 'NONE', #9358, #26370, #47853, .T. ) ;
#20935 = EDGE_CURVE ( 'NONE', #15392, #2586, #439, .T. ) ;
#20936 = ORIENTED_EDGE ( 'NONE', *, *, #436, .F. ) ;
#20937 = EDGE_LOOP ( 'NONE', ( #11408, #44828 ) ) ;
#20938 = CARTESIAN_POINT ( 'NONE',  ( -11.77071142734671660, -18.93707127637648568, 68.40792700413676641 ) ) ;
#20939 = ORIENTED_EDGE ( 'NONE', *, *, #5717, .T. ) ;
#20940 = CARTESIAN_POINT ( 'NONE',  ( -23.82269675168534206, -17.76935429418745827, 59.29818642892983860 ) ) ;
#20941 = CARTESIAN_POINT ( 'NONE',  ( -19.28643826901335245, -21.55824987104777790, 62.06673959588616185 ) ) ;
#20942 = CARTESIAN_POINT ( 'NONE',  ( -17.49284385759798965, -8.630756214087126565, 51.74842643355248129 ) ) ;
#20943 = LINE ( 'NONE', #35943, #33654 ) ;
#20944 = CARTESIAN_POINT ( 'NONE',  ( -30.42409385541305156, -6.359206544744109735, 63.99999999999998579 ) ) ;
#20945 = CARTESIAN_POINT ( 'NONE',  ( -12.41631187035346962, -9.915882575277414901, 60.74845061171743055 ) ) ;
#20946 = ORIENTED_EDGE ( 'NONE', *, *, #42220, .T. ) ;
#20947 = EDGE_CURVE ( 'NONE', #12237, #10231, #3379, .T. ) ;
#20948 = ADVANCED_FACE ( 'NONE', ( #5537 ), #10197, .F. ) ;
#20949 = CARTESIAN_POINT ( 'NONE',  ( -16.65185932245351808, -21.81708442718849383, 65.51092266128213737 ) ) ;
#20950 = CARTESIAN_POINT ( 'NONE',  ( -10.43098718212803000, -15.70539730037032911, 61.32316937334011442 ) ) ;
#20951 = CARTESIAN_POINT ( 'NONE',  ( -24.47243858273885664, -15.17772250287404567, 59.38732937676161328 ) ) ;
#20952 = DIRECTION ( 'NONE',  ( 0.2843796944294933460, 0.9587117342539337450, 5.205739956168972140E-08 ) ) ;
#20953 =( BOUNDED_SURFACE ( )  B_SPLINE_SURFACE ( 3, 1, ( 
 ( #21098, #31934 ),
 ( #32185, #13444 ),
 ( #28490, #24565 ),
 ( #40295, #36095 ),
 ( #21584, #28961 ),
 ( #13194, #36562 ),
 ( #43515, #10503 ) ),
 .UNSPECIFIED., .T., .F., .F. ) 
 B_SPLINE_SURFACE_WITH_KNOTS ( ( 4, 3, 4 ),
 ( 2, 2 ),
 ( 0.000000000000000000, 0.5000000000000000000, 1.000000000000000000 ),
 ( 0.000000000000000000, 1.000000000000000000 ),
 .UNSPECIFIED. ) 
 GEOMETRIC_REPRESENTATION_ITEM ( )  RATIONAL_B_SPLINE_SURFACE ( (
 ( 1.000000000000000000, 1.000000000000000000),
 ( 0.3333333333333335369, 0.3333333333333330373),
 ( 0.3333333333333335369, 0.3333333333333330373),
 ( 1.000000000000000000, 1.000000000000000000),
 ( 0.3333333333333333703, 0.3333333333333333703),
 ( 0.3333333333333333703, 0.3333333333333333703),
 ( 1.000000000000000000, 1.000000000000000000) ) ) 
 REPRESENTATION_ITEM ( '' )  SURFACE ( )  );
#20954 = ORIENTED_EDGE ( 'NONE', *, *, #27294, .T. ) ;
#20955 = VERTEX_POINT ( 'NONE', #24734 ) ;
#20956 = EDGE_CURVE ( 'NONE', #38833, #28434, #13419, .T. ) ;
#20957 = CARTESIAN_POINT ( 'NONE',  ( -24.07704370891654122, -17.14264987453632827, 72.89808101046213551 ) ) ;
#20958 = CARTESIAN_POINT ( 'NONE',  ( -23.34715393241125980, -19.32824242744487719, 59.00597867367864779 ) ) ;
#20959 = EDGE_LOOP ( 'NONE', ( #40987, #6488, #37612, #30312, #45080 ) ) ;
#20960 = B_SPLINE_CURVE_WITH_KNOTS ( 'NONE', 1,
 ( #20930, #46564 ),
 .UNSPECIFIED., .F., .F.,
 ( 2, 2 ),
 ( 0.000000000000000000, 1.000000000000000000 ),
 .UNSPECIFIED. ) ;
#20961 =( BOUNDED_CURVE ( )  B_SPLINE_CURVE ( 3, ( #42597, #23147, #38375, #19434 ),
 .UNSPECIFIED., .F., .F. ) 
 B_SPLINE_CURVE_WITH_KNOTS ( ( 4, 4 ),
 ( 0.4074455897393639559, 0.5000000000000000000 ),
 .UNSPECIFIED. ) 
 CURVE ( )  GEOMETRIC_REPRESENTATION_ITEM ( )  RATIONAL_B_SPLINE_CURVE ( ( 0.6983129098260814072, 0.7760317562606796615, 0.8765941196519831946, 0.9999999999999863443 ) ) 
 REPRESENTATION_ITEM ( '' )  );
#20962 = DIRECTION ( 'NONE',  ( 0.000000000000000000, -0.007114381193220324640, 0.9999746924698832418 ) ) ;
#20963 = VECTOR ( 'NONE', #18413, 1000.000000000000114 ) ;
#20964 = VECTOR ( 'NONE', #13241, 1000.000000000000114 ) ;
#20965 = ORIENTED_EDGE ( 'NONE', *, *, #28339, .T. ) ;
#20966 = CARTESIAN_POINT ( 'NONE',  ( -20.13271805750754950, -8.299978134201072777, 70.53628287813307907 ) ) ;
#20967 = CARTESIAN_POINT ( 'NONE',  ( -17.87922833762628017, -21.79450501533915840, 62.17535931805394256 ) ) ;
#20968 = ORIENTED_EDGE ( 'NONE', *, *, #44949, .F. ) ;
#20969 = CARTESIAN_POINT ( 'NONE',  ( -21.93498049285785001, -8.880082814678040393, 66.86161196829021947 ) ) ;
#20970 = EDGE_LOOP ( 'NONE', ( #5808, #26537, #26508, #8957 ) ) ;
#20971 = CARTESIAN_POINT ( 'NONE',  ( -10.59617215550872693, -13.26637052363490810, 71.49363181683084179 ) ) ;
#20972 = VERTEX_POINT ( 'NONE', #1829 ) ;
#20973 = CARTESIAN_POINT ( 'NONE',  ( -11.95665483952126351, -19.86987859786184885, 58.11956535282013192 ) ) ;
#20974 = CARTESIAN_POINT ( 'NONE',  ( -17.42409385541299471, -14.80920654474435594, 52.02966884056656482 ) ) ;
#20975 = CARTESIAN_POINT ( 'NONE',  ( 22.62590614458706639, 1.890747609047893185, 50.53028072113869484 ) ) ;
#20976 = ORIENTED_EDGE ( 'NONE', *, *, #10002, .T. ) ;
#20977 = DIRECTION ( 'NONE',  ( -3.071710424422018668E-17, 6.404604876783312462E-16, 1.000000000000000000 ) ) ;
#20978 = FACE_OUTER_BOUND ( 'NONE', #15259, .T. ) ;
#20979 = DIRECTION ( 'NONE',  ( 3.071710424422018668E-17, -6.404604876783312462E-16, -1.000000000000000000 ) ) ;
#20980 = CARTESIAN_POINT ( 'NONE',  ( -13.75553758628831424, -8.845634084518218643, 57.08040952457714923 ) ) ;
#20981 = FACE_OUTER_BOUND ( 'NONE', #27795, .T. ) ;
#20982 = CARTESIAN_POINT ( 'NONE',  ( -15.39536932222403287, -19.92137602241599836, 53.49999999999995026 ) ) ;
#20983 = VERTEX_POINT ( 'NONE', #16827 ) ;
#20984 = LINE ( 'NONE', #13572, #21542 ) ;
#20985 = CARTESIAN_POINT ( 'NONE',  ( -24.66730449611544529, -13.06573935865489844, 62.94768786448354092 ) ) ;
#20986 = CARTESIAN_POINT ( 'NONE',  ( -16.15373903644572451, -7.468189973811639959, 60.32215689887271992 ) ) ;
#20987 = B_SPLINE_CURVE_WITH_KNOTS ( 'NONE', 1,
 ( #22397, #7886 ),
 .UNSPECIFIED., .F., .F.,
 ( 2, 2 ),
 ( 0.000000000000000000, 1.000000000000000000 ),
 .UNSPECIFIED. ) ;
#20988 = CARTESIAN_POINT ( 'NONE',  ( -13.37636250268599092, -20.58507941322447365, 61.93135214938352107 ) ) ;
#20989 = CARTESIAN_POINT ( 'NONE',  ( -14.07761608144266674, -20.95746532167037302, 71.92607703845176559 ) ) ;
#20990 = CARTESIAN_POINT ( 'NONE',  ( -13.74909385650551563, -8.104110260919579645, 48.81699501597546487 ) ) ;
#20991 = ADVANCED_FACE ( 'NONE', ( #31868 ), #46886, .T. ) ;
#20992 = ORIENTED_EDGE ( 'NONE', *, *, #977, .F. ) ;
#20993 = CARTESIAN_POINT ( 'NONE',  ( -15.56465948913149155, -7.543361525925791788, 54.27966884056655061 ) ) ;
#20994 = CARTESIAN_POINT ( 'NONE',  ( -46.92409385541305511, -15.80920654474410725, 61.49999999999999289 ) ) ;
#20995 = ORIENTED_EDGE ( 'NONE', *, *, #16142, .F. ) ;
#20996 = CARTESIAN_POINT ( 'NONE',  ( -10.37394849890712401, -14.76283852923608464, 71.61310637325181006 ) ) ;
#20997 = DIRECTION ( 'NONE',  ( -0.8201047403141396019, 0.5722134347551370848, 7.883065731424289661E-08 ) ) ;
#20998 = FACE_OUTER_BOUND ( 'NONE', #2138, .T. ) ;
#20999 = CARTESIAN_POINT ( 'NONE',  ( -16.22163365158137793, -21.75594374583092616, 58.58585541130567975 ) ) ;
#21000 = ORIENTED_EDGE ( 'NONE', *, *, #9829, .F. ) ;
#21001 = CARTESIAN_POINT ( 'NONE',  ( -23.91439695282944200, -17.43141281116713515, 66.24357239631997629 ) ) ;
#21002 = AXIS2_PLACEMENT_3D ( 'NONE', #742, #26349, #7904 ) ;
#21003 = CARTESIAN_POINT ( 'NONE',  ( -23.65624089557865872, -11.51332380282628343, 66.57214514605458078 ) ) ;
#21004 = VECTOR ( 'NONE', #8725, 1000.000000000000114 ) ;
#21005 = ADVANCED_FACE ( 'NONE', ( #44908 ), #85, .F. ) ;
#21006 = EDGE_CURVE ( 'NONE', #11419, #45533, #40948, .T. ) ;
#21007 = CARTESIAN_POINT ( 'NONE',  ( -21.94239013569476171, -20.22099906679998327, 58.76442899523448204 ) ) ;
#21008 = ORIENTED_EDGE ( 'NONE', *, *, #33907, .F. ) ;
#21009 = CARTESIAN_POINT ( 'NONE',  ( 23.52590614458706852, 1.904976371434334181, 48.53033133619892681 ) ) ;
#21010 = CARTESIAN_POINT ( 'NONE',  ( -35.32409385541306079, -6.359206544744109735, 49.44999999999998863 ) ) ;
#21011 = EDGE_CURVE ( 'NONE', #20172, #16663, #36734, .T. ) ;
#21012 = CIRCLE ( 'NONE', #37506, 2.000000000000001332 ) ;
#21013 = ADVANCED_FACE ( 'NONE', ( #37230 ), #21410, .T. ) ;
#21014 = LINE ( 'NONE', #18015, #39767 ) ;
#21015 = CARTESIAN_POINT ( 'NONE',  ( -24.15317529415027309, -18.00651073652558054, 59.11104256832918935 ) ) ;
#21016 = CARTESIAN_POINT ( 'NONE',  ( -24.20884359724224311, -11.73171579724705005, 59.59740298356196320 ) ) ;
#21017 = CARTESIAN_POINT ( 'NONE',  ( -16.59344707466788549, -21.75974795715521282, 65.52564390620075585 ) ) ;
#21018 = VERTEX_POINT ( 'NONE', #3024 ) ;
#21019 = ORIENTED_EDGE ( 'NONE', *, *, #27011, .T. ) ;
#21020 = CARTESIAN_POINT ( 'NONE',  ( -16.61784385541304587, -6.860780111191487229, 51.02154966934377711 ) ) ;
#21021 = EDGE_CURVE ( 'NONE', #30787, #37220, #28059, .T. ) ;
#21022 = DIRECTION ( 'NONE',  ( 1.000000000000000000, 2.866981220435666553E-17, 0.000000000000000000 ) ) ;
#21023 = DIRECTION ( 'NONE',  ( -3.071710424422018668E-17, 6.404604876783312462E-16, 1.000000000000000000 ) ) ;
#21024 = CARTESIAN_POINT ( 'NONE',  ( -50.42409385541305511, -14.80920654474410725, 74.99999999999998579 ) ) ;
#21025 = VERTEX_POINT ( 'NONE', #3767 ) ;
#21026 = CARTESIAN_POINT ( 'NONE',  ( -21.02147767800124356, -20.81425002204343500, 65.88453904403851880 ) ) ;
#21027 = DIRECTION ( 'NONE',  ( 1.000000000000000000, 0.000000000000000000, 0.000000000000000000 ) ) ;
#21028 = VERTEX_POINT ( 'NONE', #40694 ) ;
#21029 = CARTESIAN_POINT ( 'NONE',  ( -24.42256168835771746, -14.59956871858401684, 66.29365741613838736 ) ) ;
#21030 = CARTESIAN_POINT ( 'NONE',  ( -24.47432067347917695, -14.77756146504815327, 59.52828185648635184 ) ) ;
#21031 = AXIS2_PLACEMENT_3D ( 'NONE', #11374, #23436, #27364 ) ;
#21032 = VECTOR ( 'NONE', #26355, 1000.000000000000227 ) ;
#21033 = EDGE_LOOP ( 'NONE', ( #14463, #40543, #23105, #10517, #6862 ) ) ;
#21034 = DIRECTION ( 'NONE',  ( 1.927470528863119542E-16, 0.000000000000000000, -1.000000000000000000 ) ) ;
#21035 = CARTESIAN_POINT ( 'NONE',  ( -12.24245737956772473, -19.51581737952565376, 57.92682380653661056 ) ) ;
#21036 = EDGE_LOOP ( 'NONE', ( #42192, #33266 ) ) ;
#21037 = DIRECTION ( 'NONE',  ( 0.9687793358424819923, -0.2479245821708680464, 0.000000000000000000 ) ) ;
#21038 = CARTESIAN_POINT ( 'NONE',  ( -24.41160895735743352, -13.85031893932584701, 73.00782755091154286 ) ) ;
#21039 = CIRCLE ( 'NONE', #33590, 2.000000000000001332 ) ;
#21040 = ADVANCED_FACE ( 'NONE', ( #22479, #18779 ), #33530, .T. ) ;
#21041 = CARTESIAN_POINT ( 'NONE',  ( -16.72764935575746748, -21.77453510730240183, 65.29852372421919426 ) ) ;
#21042 = DIRECTION ( 'NONE',  ( 1.000000000000000000, -4.164305804376849788E-17, 1.614929280266638808E-16 ) ) ;
#21043 = EDGE_LOOP ( 'NONE', ( #32993, #4668, #24083, #48291 ) ) ;
#21044 = CARTESIAN_POINT ( 'NONE',  ( -22.17374636168253943, -9.068608547125135644, 63.37809084343794552 ) ) ;
#21045 = FACE_OUTER_BOUND ( 'NONE', #20480, .T. ) ;
#21046 = CARTESIAN_POINT ( 'NONE',  ( -24.30112618867181240, -13.25578303422174997, 59.64795780745660636 ) ) ;
#21047 = FACE_OUTER_BOUND ( 'NONE', #196, .T. ) ;
#21048 = DIRECTION ( 'NONE',  ( 0.9687793358424821033, -0.2479245821708679909, 0.000000000000000000 ) ) ;
#21049 = CARTESIAN_POINT ( 'NONE',  ( -22.97409385650551528, -9.792211528768504536, 50.49490371617623197 ) ) ;
#21050 = EDGE_CURVE ( 'NONE', #39081, #22354, #18687, .T. ) ;
#21051 = CARTESIAN_POINT ( 'NONE',  ( -17.11809369177854379, -21.86054179209348192, 68.85127668957714775 ) ) ;
#21052 = CARTESIAN_POINT ( 'NONE',  ( -19.19606018965890115, -19.75113282002397597, 52.02966884056656482 ) ) ;
#21053 = ORIENTED_EDGE ( 'NONE', *, *, #48071, .T. ) ;
#21054 = PLANE ( 'NONE',  #19810 ) ;
#21055 = CARTESIAN_POINT ( 'NONE',  ( -41.80005222645378637, -14.90920654474423124, 67.99233303167419251 ) ) ;
#21056 = CARTESIAN_POINT ( 'NONE',  ( -20.47136568995129480, -10.23054578351413468, 54.07175714974879099 ) ) ;
#21057 = ORIENTED_EDGE ( 'NONE', *, *, #34313, .T. ) ;
#21058 = CARTESIAN_POINT ( 'NONE',  ( -13.95487512861695834, -17.97781459419518058, 49.52966884056656482 ) ) ;
#21059 = ORIENTED_EDGE ( 'NONE', *, *, #5790, .F. ) ;
#21060 = VERTEX_POINT ( 'NONE', #26417 ) ;
#21061 = VERTEX_POINT ( 'NONE', #41427 ) ;
#21062 = EDGE_CURVE ( 'NONE', #1905, #20878, #22763, .T. ) ;
#21063 = CARTESIAN_POINT ( 'NONE',  ( -14.00884730389179822, -20.92003478889483858, 72.20991175584978805 ) ) ;
#21064 = AXIS2_PLACEMENT_3D ( 'NONE', #38399, #8153, #23166 ) ;
#21065 = ADVANCED_FACE ( 'NONE', ( #38707 ), #33028, .T. ) ;
#21066 = CARTESIAN_POINT ( 'NONE',  ( -23.72077351878440510, -11.75113111449199721, 59.67339008053482274 ) ) ;
#21067 = CARTESIAN_POINT ( 'NONE',  ( -15.94604045176571283, -7.966968909199487747, 63.89684263511286133 ) ) ;
#21068 = CARTESIAN_POINT ( 'NONE',  ( -19.85909425162068942, -21.37257694502213567, 72.64634926892956912 ) ) ;
#21069 = CARTESIAN_POINT ( 'NONE',  ( -22.88850900265194355, -15.54278860761184866, 53.88362224778186516 ) ) ;
#21070 = AXIS2_PLACEMENT_3D ( 'NONE', #19191, #4411, #15473 ) ;
#21071 = AXIS2_PLACEMENT_3D ( 'NONE', #13192, #43514, #24794 ) ;
#21072 = ORIENTED_EDGE ( 'NONE', *, *, #8484, .F. ) ;
#21073 = ORIENTED_EDGE ( 'NONE', *, *, #27493, .F. ) ;
#21074 = EDGE_CURVE ( 'NONE', #18139, #3011, #38073, .T. ) ;
#21075 = CARTESIAN_POINT ( 'NONE',  ( -19.12409385650551741, -6.426201560718813433, 50.50509628382439331 ) ) ;
#21076 = B_SPLINE_CURVE_WITH_KNOTS ( 'NONE', 3,
 ( #23810, #16138, #24048, #27727, #5327, #46204, #23314, #31671, #4356, #34374 ),
 .UNSPECIFIED., .F., .F.,
 ( 4, 2, 2, 2, 4 ),
 ( 0.000000000000000000, 0.2500000000000000000, 0.5000000000000000000, 0.7500000000000000000, 1.000000000000000000 ),
 .UNSPECIFIED. ) ;
#21077 = DIRECTION ( 'NONE',  ( -1.224646799147353207E-16, -1.000000000000000000, 1.912410701131276611E-32 ) ) ;
#21078 = AXIS2_PLACEMENT_3D ( 'NONE', #33614, #47935, #22076 ) ;
#21079 = DIRECTION ( 'NONE',  ( 0.3374354101627465297, 0.9413486835218388693, 1.423378189492272923E-08 ) ) ;
#21080 = EDGE_CURVE ( 'NONE', #32817, #35558, #36483, .T. ) ;
#21081 = CARTESIAN_POINT ( 'NONE',  ( -17.49284385650551599, -7.406986770994973490, 48.81910596585309747 ) ) ;
#21082 = AXIS2_PLACEMENT_3D ( 'NONE', #45411, #25708, #18302 ) ;
#21083 = ORIENTED_EDGE ( 'NONE', *, *, #13802, .F. ) ;
#21084 = CARTESIAN_POINT ( 'NONE',  ( -15.55648817577099585, -8.010769314271311003, 74.09457776258329886 ) ) ;
#21085 = DIRECTION ( 'NONE',  ( -2.430360958779124298E-06, -9.751098539734333949E-07, 0.9999999999965712982 ) ) ;
#21086 =( BOUNDED_CURVE ( )  B_SPLINE_CURVE ( 3, ( #40079, #20882, #32449, #17158 ),
 .UNSPECIFIED., .F., .F. ) 
 B_SPLINE_CURVE_WITH_KNOTS ( ( 4, 4 ),
 ( 0.000000000000000000, 0.4074455897393671200 ),
 .UNSPECIFIED. ) 
 CURVE ( )  GEOMETRIC_REPRESENTATION_ITEM ( )  RATIONAL_B_SPLINE_CURVE ( ( 1.000000000000000000, 0.4567392136813310244, 0.3561768502900299338, 0.6983129098260968393 ) ) 
 REPRESENTATION_ITEM ( '' )  );
#21087 = ORIENTED_EDGE ( 'NONE', *, *, #5334, .T. ) ;
#21088 = FACE_OUTER_BOUND ( 'NONE', #31468, .T. ) ;
#21089 = ORIENTED_EDGE ( 'NONE', *, *, #1147, .T. ) ;
#21090 = FACE_OUTER_BOUND ( 'NONE', #7292, .T. ) ;
#21091 = CARTESIAN_POINT ( 'NONE',  ( -10.40888601095206134, -14.10966482229656194, 61.21821293885882653 ) ) ;
#21092 = CARTESIAN_POINT ( 'NONE',  ( -14.43571338001569870, -7.984821196993008741, 63.88955222746418627 ) ) ;
#21093 = ORIENTED_EDGE ( 'NONE', *, *, #8608, .F. ) ;
#21094 = AXIS2_PLACEMENT_3D ( 'NONE', #48649, #11234, #40525 ) ;
#21095 = DIRECTION ( 'NONE',  ( 7.652304183832323392E-06, 2.165757503891338892E-06, 0.9999999999683758523 ) ) ;
#21096 = CIRCLE ( 'NONE', #13305, 0.5000000000000004441 ) ;
#21097 = EDGE_CURVE ( 'NONE', #11018, #22946, #20829, .T. ) ;
#21098 = CARTESIAN_POINT ( 'NONE',  ( -22.75539019595755263, -10.19575032747719590, 66.82710158566565894 ) ) ;
#21099 = FACE_OUTER_BOUND ( 'NONE', #26262, .T. ) ;
#21100 = ORIENTED_EDGE ( 'NONE', *, *, #32711, .F. ) ;
#21101 = CARTESIAN_POINT ( 'NONE',  ( -20.77672337442954031, -20.95411300689461953, 58.83578372821326496 ) ) ;
#21102 =( BOUNDED_CURVE ( )  B_SPLINE_CURVE ( 2, ( #21049, #21302, #47638, #25704, #6996, #10219, #24988, #22017, #13873, #17813, #36297, #3045, #29162, #6758, #48115, #40006, #14346, #44438, #3299, #33307, #2579, #17581, #28917, #25232, #7994, #34057, #38229, #582, #22501, #48596, #22259, #23242, #4514, #26440, #26201, #45663, #40973, #23012, #37250, #19534, #11916, #41708, #15576, #19292, #110, #14833, #29901, #19052, #10935, #15095, #33553, #34542, #4282, #30393, #30151, #37996, #34296, #30638, #26934, #7256, #3794, #3537, #33814, #827, #4050, #45176, #45407, #15828, #18804, #7500, #44932, #18546, #22761, #41952, #8227, #11185, #11415, #41212, #41452, #7748, #11663, #30878, #37499, #37753, #25955, #349, #26689, #15334, #27652, #35748, #39218, #16555, #5014, #35520, #12631, #20268, #1295, #1795, #31594, #8952, #5248, #8455, #12384, #42191, #27407, #20024, #31832, #28136, #31343, #2031, #46854, #35027, #42685, #42441, #42918, #23969, #13095, #4766, #43161, #17027, #35272, #12151, #24460, #16795, #16304, #23485, #23736, #46622, #39463, #12865, #5501, #9436, #38972, #46374, #27170, #1545, #27893, #9190, #19791, #5747, #24208, #20749, #45892, #20516, #38481, #38730, #46125, #34794, #1065, #16063, #31106, #8711, #36470, #48054, #32551, #10632, #21482, #6935, #17280, #5968, #43416, #13337, #24926, #17996, #20990, #39943, #43899, #36949, #36237, #13814, #28855, #47579, #9681, #25411, #21710, #28622, #6215, #44377, #2519 ),
 .UNSPECIFIED., .F., .F. ) 
 B_SPLINE_CURVE_WITH_KNOTS ( ( 3, 2, 2, 2, 2, 2, 2, 2, 2, 2, 2, 2, 2, 2, 2, 2, 2, 2, 2, 2, 2, 2, 2, 2, 2, 2, 2, 2, 2, 2, 2, 2, 2, 2, 2, 2, 2, 2, 2, 2, 2, 2, 2, 2, 2, 2, 2, 2, 2, 2, 2, 2, 2, 2, 2, 2, 2, 2, 2, 2, 2, 2, 2, 2, 2, 2, 2, 2, 2, 2, 2, 2, 2, 2, 2, 2, 2, 2, 2, 2, 2, 2, 2, 2, 2, 2, 2, 2, 2, 3 ),
 ( 0.000000000000000000, 0.01125025777839750753, 0.02250051555679501505, 0.03375077333519252432, 0.04500103111359003011, 0.05625128889198754284, 0.06750154667038504863, 0.07875180444878256136, 0.09000206222718006022, 0.1012523200055775729, 0.1125025777839750857, 0.1237528355623725845, 0.1350030933407700973, 0.1462533511191675961, 0.1575036088975651227, 0.1687538666759626216, 0.1800041244543601204, 0.1912543822327576470, 0.2025046400111551459, 0.2137548977895526447, 0.2250051555679501714, 0.2362554133463476702, 0.2475056711247451691, 0.2587559289031426957, 0.2700061866815401945, 0.2812564444599377489, 0.2925067022383351922, 0.3037569600167327466, 0.3150072177951302455, 0.3262574755735277443, 0.3375077333519252432, 0.3487579911303227975, 0.3600082489087202409, 0.3712585066871177952, 0.3825087644655152941, 0.3937590222439127929, 0.4050092800223102918, 0.4162595378007078462, 0.4275097955791052895, 0.4387600533575028439, 0.4500103111359003427, 0.4612605689142978416, 0.4725108266926953404, 0.4837610844710928948, 0.4950113422494903381, 0.5062616000278878925, 0.5175118578062853913, 0.5287621155846828902, 0.5400123733630803891, 0.5512626311414778879, 0.5625128889198754978, 0.5737631466982728856, 0.5850134044766703845, 0.5962636622550679943, 0.6075139200334654932, 0.6187641778118628810, 0.6300144355902604909, 0.6412646933686579898, 0.6525149511470554886, 0.6637652089254529875, 0.6750154667038504863, 0.6862657244822479852, 0.6975159822606455950, 0.7087662400390429829, 0.7200164978174404817, 0.7312667555958380916, 0.7425170133742355905, 0.7537672711526329783, 0.7650175289310305882, 0.7762677867094280870, 0.7875180444878255859, 0.7987683022662230847, 0.8100185600446205836, 0.8212688178230180824, 0.8325190756014156923, 0.8437693333798130801, 0.8550195911582105790, 0.8662698489366081889, 0.8775201067150056877, 0.8887703644934030756, 0.9000206222718006854, 0.9112708800501981843, 0.9225211378285956831, 0.9337713956069931820, 0.9450216533853906808, 0.9562719111637881797, 0.9675221689421857896, 0.9787724267205831774, 0.9900226844989806763, 1.000000000000000000 ),
 .UNSPECIFIED. ) 
 CURVE ( )  GEOMETRIC_REPRESENTATION_ITEM ( )  RATIONAL_B_SPLINE_CURVE ( ( 1.000000000000000000, 0.9238795325112867385, 1.000000000000000000, 0.9238795325112867385, 1.000000000000000000, 0.9238795325112867385, 1.000000000000000000, 0.9238795325112867385, 1.000000000000000000, 0.9238795325112867385, 1.000000000000000000, 0.9238795325112867385, 1.000000000000000000, 0.9238795325112867385, 1.000000000000000000, 0.9238795325112867385, 1.000000000000000000, 0.9238795325112867385, 1.000000000000000000, 0.9238795325112867385, 1.000000000000000000, 0.9238795325112867385, 1.000000000000000000, 0.9238795325112867385, 1.000000000000000000, 0.9238795325112867385, 1.000000000000000000, 0.9238795325112867385, 1.000000000000000000, 0.9238795325112867385, 1.000000000000000000, 0.9238795325112867385, 1.000000000000000000, 0.9238795325112867385, 1.000000000000000000, 0.9238795325112867385, 1.000000000000000000, 0.9238795325112867385, 1.000000000000000000, 0.9238795325112867385, 1.000000000000000000, 0.9238795325112867385, 1.000000000000000000, 0.9238795325112867385, 1.000000000000000000, 0.9238795325112867385, 1.000000000000000000, 0.9238795325112867385, 1.000000000000000000, 0.9238795325112867385, 1.000000000000000000, 0.9238795325112867385, 1.000000000000000000, 0.9238795325112867385, 1.000000000000000000, 0.9238795325112867385, 1.000000000000000000, 0.9238795325112867385, 1.000000000000000000, 0.9238795325112867385, 1.000000000000000000, 0.9238795325112867385, 1.000000000000000000, 0.9238795325112867385, 1.000000000000000000, 0.9238795325112867385, 1.000000000000000000, 0.9238795325112867385, 1.000000000000000000, 0.9238795325112867385, 1.000000000000000000, 0.9238795325112867385, 1.000000000000000000, 0.9238795325112867385, 1.000000000000000000, 0.9238795325112867385, 1.000000000000000000, 0.9238795325112867385, 1.000000000000000000, 0.9238795325112867385, 1.000000000000000000, 0.9238795325112867385, 1.000000000000000000, 0.9238795325112867385, 1.000000000000000000, 0.9238795325112867385, 1.000000000000000000, 0.9238795325112867385, 1.000000000000000000, 0.9238795325112867385, 1.000000000000000000, 0.9238795325112867385, 1.000000000000000000, 0.9238795325112867385, 1.000000000000000000, 0.9238795325112867385, 1.000000000000000000, 0.9238795325112867385, 1.000000000000000000, 0.9238795325112867385, 1.000000000000000000, 0.9238795325112867385, 1.000000000000000000, 0.9238795325112867385, 1.000000000000000000, 0.9238795325112867385, 1.000000000000000000, 0.9238795325112867385, 1.000000000000000000, 0.9238795325112867385, 1.000000000000000000, 0.9238795325112867385, 1.000000000000000000, 0.9238795325112867385, 1.000000000000000000, 0.9238795325112867385, 1.000000000000000000, 0.9238795325112867385, 1.000000000000000000, 0.9238795325112867385, 1.000000000000000000, 0.9238795325112867385, 1.000000000000000000, 0.9238795325112867385, 1.000000000000000000, 0.9238795325112867385, 1.000000000000000000, 0.9238795325112867385, 1.000000000000000000, 0.9238795325112867385, 1.000000000000000000, 0.9238795325112867385, 1.000000000000000000, 0.9238795325112867385, 1.000000000000000000, 0.9238795325112867385, 1.000000000000000000, 0.9238795325112867385, 1.000000000000000000, 0.9238795325112867385, 1.000000000000000000, 0.9238795325112867385, 1.000000000000000000, 0.9238795325112867385, 1.000000000000000000, 0.9238795325112867385, 1.000000000000000000, 0.9238795325112867385, 1.000000000000000000, 0.9238795325112867385, 1.000000000000000000, 0.9238795325112867385, 1.000000000000000000, 0.9238795325112867385, 1.000000000000000000, 0.9238795325112867385, 1.000000000000000000, 0.9238795325112867385, 1.000000000000000000, 0.9238795325112867385, 1.000000000000000000, 0.9238795325112867385, 1.000000000000000000, 0.9238795325112867385, 1.000000000000000000, 0.9238795325112867385, 1.000000000000000000, 0.9238795325112867385, 1.000000000000000000, 0.9238795325112867385, 1.000000000000000000, 0.9238795325112867385, 1.000000000000000000, 0.9238795325112867385, 1.000000000000000000, 0.9238795325112867385, 1.000000000000000000, 0.9324923983805685213, 0.9847233224627454096 ) ) 
 REPRESENTATION_ITEM ( '' )  );
#21103 = AXIS2_PLACEMENT_3D ( 'NONE', #46953, #2857, #24570 ) ;
#21104 = EDGE_LOOP ( 'NONE', ( #28113, #12305 ) ) ;
#21105 = DIRECTION ( 'NONE',  ( 0.9904243694481097426, 0.1380563957348939774, 6.973877024228147881E-08 ) ) ;
#21106 = DIRECTION ( 'NONE',  ( 0.3111098983483954750, 0.8385765505603235415, 0.4472135954999582608 ) ) ;
#21107 = ORIENTED_EDGE ( 'NONE', *, *, #26894, .F. ) ;
#21108 = DIRECTION ( 'NONE',  ( 0.9271861211590526342, 0.3746009833543293421, -1.005599061620490611E-08 ) ) ;
#21109 = LINE ( 'NONE', #13204, #45200 ) ;
#21110 = CARTESIAN_POINT ( 'NONE',  ( -17.20949509180255887, -7.759470163990226155, 74.37506982372057962 ) ) ;
#21111 = DIRECTION ( 'NONE',  ( 0.9372362738803845517, 0.3486949482324239735, -5.386914174890155429E-09 ) ) ;
#21112 = ORIENTED_EDGE ( 'NONE', *, *, #16613, .T. ) ;
#21113 = DIRECTION ( 'NONE',  ( -0.7700094066334557397, -0.6380325334150237504, 0.000000000000000000 ) ) ;
#21114 = CIRCLE ( 'NONE', #22707, 1.999999999999999112 ) ;
#21115 = CARTESIAN_POINT ( 'NONE',  ( -15.09544287645192640, -21.46351977604527761, 65.10596681500476279 ) ) ;
#21116 = FACE_OUTER_BOUND ( 'NONE', #7533, .T. ) ;
#21117 = ORIENTED_EDGE ( 'NONE', *, *, #20258, .F. ) ;
#21118 = CARTESIAN_POINT ( 'NONE',  ( -10.38974003836240634, -14.29666208179129150, 68.27288787427933414 ) ) ;
#21119 =( BOUNDED_CURVE ( )  B_SPLINE_CURVE ( 3, ( #36490, #2771, #32098, #28158 ),
 .UNSPECIFIED., .F., .F. ) 
 B_SPLINE_CURVE_WITH_KNOTS ( ( 4, 4 ),
 ( 0.000000000000000000, 0.4074455897393701176 ),
 .UNSPECIFIED. ) 
 CURVE ( )  GEOMETRIC_REPRESENTATION_ITEM ( )  RATIONAL_B_SPLINE_CURVE ( ( 1.000000000000000000, 0.4567392136813304138, 0.3561768502900297118, 0.6983129098260978385 ) ) 
 REPRESENTATION_ITEM ( '' )  );
#21120 = CARTESIAN_POINT ( 'NONE',  ( -12.50648677543191134, -9.746390325112967545, 60.70350793514798937 ) ) ;
#21121 = EDGE_LOOP ( 'NONE', ( #5382, #23893, #47865, #46684, #24178 ) ) ;
#21122 = ORIENTED_EDGE ( 'NONE', *, *, #5429, .T. ) ;
#21123 = LINE ( 'NONE', #36120, #40882 ) ;
#21124 = LINE ( 'NONE', #36121, #22549 ) ;
#21125 = ADVANCED_FACE ( 'NONE', ( #41926 ), #27145, .T. ) ;
#21126 = CARTESIAN_POINT ( 'NONE',  ( -19.92736525831631766, -21.34646298403863085, 72.70478735915031621 ) ) ;
#21127 = CARTESIAN_POINT ( 'NONE',  ( -19.82409385650551670, -6.426201560718813433, 50.50509628382439331 ) ) ;
#21128 = CARTESIAN_POINT ( 'NONE',  ( -10.12326218194131044, -13.32541594658350448, 74.86312942357149325 ) ) ;
#21129 = CARTESIAN_POINT ( 'NONE',  ( -23.85760449859744625, -11.05106826658364838, 70.00555402674318373 ) ) ;
#21130 = CARTESIAN_POINT ( 'NONE',  ( -12.37644175686812709, -19.65923236128709561, 61.39678630681033411 ) ) ;
#21131 = CARTESIAN_POINT ( 'NONE',  ( -12.89671927708317689, -20.22380232670898081, 68.49224713894388117 ) ) ;
#21132 = DIRECTION ( 'NONE',  ( -2.866981220435666553E-17, 1.000000000000000000, 1.190614954331866791E-16 ) ) ;
#21133 = ORIENTED_EDGE ( 'NONE', *, *, #3796, .F. ) ;
#21134 = EDGE_LOOP ( 'NONE', ( #87, #9659, #44325, #11722, #15219 ) ) ;
#21135 = EDGE_CURVE ( 'NONE', #25681, #37096, #25853, .T. ) ;
#21136 = CARTESIAN_POINT ( 'NONE',  ( -10.45033584411928551, -15.86823462405053853, 61.03788874849474411 ) ) ;
#21137 = CARTESIAN_POINT ( 'NONE',  ( -23.11114181986270566, -9.996704532105994190, 66.64208010989614195 ) ) ;
#21138 = AXIS2_PLACEMENT_3D ( 'NONE', #16057, #576, #19047 ) ;
#21139 = CARTESIAN_POINT ( 'NONE',  ( -11.39216336840796373, -18.45920852072106300, 61.29182966166492719 ) ) ;
#21140 = CARTESIAN_POINT ( 'NONE',  ( -10.53786819255349805, -17.65216208274645382, 68.24721944767701132 ) ) ;
#21141 = EDGE_CURVE ( 'NONE', #18208, #2492, #5763, .T. ) ;
#21142 = CARTESIAN_POINT ( 'NONE',  ( -11.12358220677134035, -11.75903396576748605, 71.08860871065073184 ) ) ;
#21143 = CARTESIAN_POINT ( 'NONE',  ( -19.99284385650551243, -7.406986770994973490, 48.81910596585309747 ) ) ;
#21144 = VECTOR ( 'NONE', #31710, 1000.000000000000000 ) ;
#21145 = AXIS2_PLACEMENT_3D ( 'NONE', #3208, #18214, #14738 ) ;
#21146 = ORIENTED_EDGE ( 'NONE', *, *, #34780, .T. ) ;
#21147 = CARTESIAN_POINT ( 'NONE',  ( -22.92319923916556235, -10.39759239192951235, 63.07185995337424345 ) ) ;
#21148 = DIRECTION ( 'NONE',  ( 0.3047757271037813687, 0.002884009000661817267, -0.9524197806957001022 ) ) ;
#21149 = FACE_OUTER_BOUND ( 'NONE', #46994, .T. ) ;
#21150 = CARTESIAN_POINT ( 'NONE',  ( -10.38377074815290868, -15.30802594933397920, 61.18222038349547631 ) ) ;
#21151 = AXIS2_PLACEMENT_3D ( 'NONE', #22431, #29830, #33001 ) ;
#21152 = EDGE_CURVE ( 'NONE', #19754, #47755, #16331, .T. ) ;
#21153 = ORIENTED_EDGE ( 'NONE', *, *, #43993, .F. ) ;
#21154 = EDGE_CURVE ( 'NONE', #21258, #22071, #25156, .T. ) ;
#21155 = DIRECTION ( 'NONE',  ( 2.866981220435666553E-17, -1.000000000000000000, -1.190614954331866791E-16 ) ) ;
#21156 = EDGE_CURVE ( 'NONE', #6917, #45300, #32361, .T. ) ;
#21157 = DIRECTION ( 'NONE',  ( -1.000000000000000000, 0.000000000000000000, 9.637352644315596475E-17 ) ) ;
#21158 = DIRECTION ( 'NONE',  ( -0.09332174201254901658, -0.9956360040033422898, 0.000000000000000000 ) ) ;
#21159 = DIRECTION ( 'NONE',  ( 1.205044182495138397E-05, 2.694341358818416019E-06, 0.9999999999237635384 ) ) ;
#21160 = EDGE_LOOP ( 'NONE', ( #24931, #12544 ) ) ;
#21161 = CARTESIAN_POINT ( 'NONE',  ( -23.05544494128708521, -18.96707680103153493, 59.07513778477354549 ) ) ;
#21162 = ORIENTED_EDGE ( 'NONE', *, *, #25735, .T. ) ;
#21163 = CARTESIAN_POINT ( 'NONE',  ( -23.59327504554355315, -11.39630409041826020, 69.90682860766239060 ) ) ;
#21164 = CARTESIAN_POINT ( 'NONE',  ( -10.21764033814386963, -12.91954908504599331, 67.92327745040803677 ) ) ;
#21165 = ORIENTED_EDGE ( 'NONE', *, *, #23609, .F. ) ;
#21166 = CARTESIAN_POINT ( 'NONE',  ( -13.72534930678190079, -21.27637739626202062, 68.61658465623135328 ) ) ;
#21167 = CARTESIAN_POINT ( 'NONE',  ( -12.54422445394979135, -19.90840678475983694, 71.95086485943772914 ) ) ;
#21168 = VECTOR ( 'NONE', #13249, 1000.000000000000000 ) ;
#21169 = ORIENTED_EDGE ( 'NONE', *, *, #26603, .T. ) ;
#21170 = DIRECTION ( 'NONE',  ( -0.9687793358424819923, 0.2479245821708680464, 0.000000000000000000 ) ) ;
#21171 = PRODUCT_DEFINITION_FORMATION_WITH_SPECIFIED_SOURCE ( 'ANY', '', #33418, .NOT_KNOWN. ) ;
#21172 = CARTESIAN_POINT ( 'NONE',  ( -17.59331746331979929, -7.761237803891376963, 63.55057029381061540 ) ) ;
#21173 = CARTESIAN_POINT ( 'NONE',  ( -10.88209246082447912, -17.29963176008448400, 64.92739380462948873 ) ) ;
#21174 = ORIENTED_EDGE ( 'NONE', *, *, #15675, .F. ) ;
#21175 = CARTESIAN_POINT ( 'NONE',  ( -17.01690395770326347, -19.47798354061844961, 52.02966884056656482 ) ) ;
#21176 = VECTOR ( 'NONE', #22441, 1000.000000000000000 ) ;
#21177 = AXIS2_PLACEMENT_3D ( 'NONE', #48051, #44373, #44611 ) ;
#21178 = CARTESIAN_POINT ( 'NONE',  ( -17.26457240846633567, -7.760713630915982542, 70.50507891880883449 ) ) ;
#21179 = DIRECTION ( 'NONE',  ( 0.9660698163281071782, 0.2582810677919975539, -5.363434502754611677E-08 ) ) ;
#21180 = CARTESIAN_POINT ( 'NONE',  ( -23.00454255336054743, -10.50046069577333263, 59.88731295783226471 ) ) ;
#21181 = ORIENTED_EDGE ( 'NONE', *, *, #8727, .T. ) ;
#21182 = ORIENTED_EDGE ( 'NONE', *, *, #28709, .T. ) ;
#21183 = FACE_OUTER_BOUND ( 'NONE', #17974, .T. ) ;
#21184 = CARTESIAN_POINT ( 'NONE',  ( -24.31717724401442027, -16.02832029180493478, 62.66616618629565494 ) ) ;
#21185 = EDGE_LOOP ( 'NONE', ( #702, #1557, #16244, #33681, #9857, #22833, #14502, #26419, #44463, #25685, #16140, #21947, #44860, #27087, #1485, #44631, #32304, #48104, #26884, #7873, #47857, #25643, #9416, #18599, #1929, #38607, #19912, #2450, #42719, #40486, #38465, #21181, #3034 ) ) ;
#21186 = CARTESIAN_POINT ( 'NONE',  ( -10.56492483649129710, -13.18000429128331596, 71.50828586225091499 ) ) ;
#21187 = AXIS2_PLACEMENT_3D ( 'NONE', #31163, #12443, #12207 ) ;
#21188 = CARTESIAN_POINT ( 'NONE',  ( -18.28034385759799108, -9.360768649639302552, 51.01397948905922419 ) ) ;
#21189 = CARTESIAN_POINT ( 'NONE',  ( -15.83093346616859876, -7.941424302753512521, 67.43447455194694840 ) ) ;
#21190 = DIRECTION ( 'NONE',  ( -1.000000000000000000, -1.669677910507523057E-21, -6.493791346278465266E-22 ) ) ;
#21191 = CARTESIAN_POINT ( 'NONE',  ( -20.58562488885964825, -8.063118024066820766, 66.94250577013032455 ) ) ;
#21192 = ORIENTED_EDGE ( 'NONE', *, *, #18905, .F. ) ;
#21193 = EDGE_CURVE ( 'NONE', #15483, #20349, #15023, .T. ) ;
#21194 = CARTESIAN_POINT ( 'NONE',  ( -11.10681587527927938, -11.67891925637714401, 71.10332952723315714 ) ) ;
#21195 = CARTESIAN_POINT ( 'NONE',  ( -14.86706299937602793, -21.37930449507021180, 61.64160199363316650 ) ) ;
#21196 = DIRECTION ( 'NONE',  ( 0.5510797171261918592, -0.8280216580999281151, 0.1033986416233892563 ) ) ;
#21197 = CARTESIAN_POINT ( 'NONE',  ( -11.42622260759249286, -18.51434353338492400, 61.57710833179551457 ) ) ;
#21198 = EDGE_LOOP ( 'NONE', ( #5748, #1259, #11003, #10990, #11281 ) ) ;
#21199 = VERTEX_POINT ( 'NONE', #24672 ) ;
#21200 = CARTESIAN_POINT ( 'NONE',  ( -24.87289997924709439, -14.67112824012948202, 62.82801159608117558 ) ) ;
#21201 = CARTESIAN_POINT ( 'NONE',  ( -14.07810500574514556, -21.01869930352526694, 68.66444892306193992 ) ) ;
#21202 = AXIS2_PLACEMENT_3D ( 'NONE', #18162, #33174, #14440 ) ;
#21203 = CARTESIAN_POINT ( 'NONE',  ( -24.09792889798371007, -17.08130376423426000, 73.18336032035891492 ) ) ;
#21204 = VERTEX_POINT ( 'NONE', #39916 ) ;
#21205 = CIRCLE ( 'NONE', #32951, 5.249999999999998224 ) ;
#21206 = EDGE_CURVE ( 'NONE', #25341, #14217, #39662, .T. ) ;
#21207 = CARTESIAN_POINT ( 'NONE',  ( -20.75918756122348441, -8.147305293919229641, 63.42626095967343502 ) ) ;
#21208 = B_SPLINE_CURVE_WITH_KNOTS ( 'NONE', 3,
 ( #46844, #38966, #32544, #35265, #13805, #39694, #13570, #17272, #35984, #5494 ),
 .UNSPECIFIED., .F., .F.,
 ( 4, 2, 2, 2, 4 ),
 ( 0.000000000000000000, 0.2500000000000000000, 0.5000000000000000000, 0.7500000000000000000, 1.000000000000000000 ),
 .UNSPECIFIED. ) ;
#21209 = CARTESIAN_POINT ( 'NONE',  ( -30.42409385541305156, -8.109206544744111511, 50.50000000000000000 ) ) ;
#21210 = EDGE_CURVE ( 'NONE', #41834, #14119, #987, .T. ) ;
#21211 = ADVANCED_FACE ( 'NONE', ( #20727 ), #44419, .T. ) ;
#21212 = VERTEX_POINT ( 'NONE', #20492 ) ;
#21213 = DIRECTION ( 'NONE',  ( -0.8244078399817417191, -0.5659962132175737626, -7.627400653636452305E-08 ) ) ;
#21214 = VECTOR ( 'NONE', #1855, 1000.000000000000000 ) ;
#21215 = CARTESIAN_POINT ( 'NONE',  ( -12.51352073908361184, -20.41184545669705130, 71.91379515285952095 ) ) ;
#21216 = CARTESIAN_POINT ( 'NONE',  ( -16.82968708298378857, -21.83425273348639806, 68.99000854178609643 ) ) ;
#21217 = ORIENTED_EDGE ( 'NONE', *, *, #41730, .T. ) ;
#21218 = CARTESIAN_POINT ( 'NONE',  ( 6.575906144586949331, -9.359200813967568422, 50.49621490985803263 ) ) ;
#21219 = VERTEX_POINT ( 'NONE', #5719 ) ;
#21220 = CARTESIAN_POINT ( 'NONE',  ( -14.19282086353638661, -8.542981675383003903, 71.01485553001869278 ) ) ;
#21221 = PLANE ( 'NONE',  #22047 ) ;
#21222 = CARTESIAN_POINT ( 'NONE',  ( -10.76763519559319882, -17.13171766695033327, 61.15743118826002700 ) ) ;
#21223 = EDGE_LOOP ( 'NONE', ( #24914, #9785, #7860, #40489, #44803 ) ) ;
#21224 = CARTESIAN_POINT ( 'NONE',  ( -21.36930209557634086, -21.12890771240575916, 69.16176048667763610 ) ) ;
#21225 = CARTESIAN_POINT ( 'NONE',  ( -24.47354813883760016, -12.39902559715248032, 73.42720875634239519 ) ) ;
#21226 = CARTESIAN_POINT ( 'NONE',  ( -24.10584550580110985, -12.56049697540380095, 73.54225570139644219 ) ) ;
#21227 = DIRECTION ( 'NONE',  ( 0.000000000000000000, -0.000000000000000000, 1.000000000000000000 ) ) ;
#21228 = CARTESIAN_POINT ( 'NONE',  ( -45.55409385541306477, -12.76354662275040397, 71.04301729251712061 ) ) ;
#21229 = DIRECTION ( 'NONE',  ( 1.927470528863119542E-16, 0.000000000000000000, -1.000000000000000000 ) ) ;
#21230 = VERTEX_POINT ( 'NONE', #13073 ) ;
#21231 = CARTESIAN_POINT ( 'NONE',  ( -12.85925802207596114, -13.69662874518196993, 52.02966884056656482 ) ) ;
#21232 = CARTESIAN_POINT ( 'NONE',  ( -11.79792781917550570, -18.97409009807959279, 71.68685885149984927 ) ) ;
#21233 = CARTESIAN_POINT ( 'NONE',  ( -24.69063629745726374, -16.45233172012289558, 59.27332428859715918 ) ) ;
#21234 = DIRECTION ( 'NONE',  ( 5.551115123125782702E-17, 1.232595164407830946E-32, 1.000000000000000000 ) ) ;
#21235 = DIRECTION ( 'NONE',  ( -2.866981220435666553E-17, 1.000000000000000000, 1.190614954331866791E-16 ) ) ;
#21236 = CARTESIAN_POINT ( 'NONE',  ( -24.26335596148664564, -16.30820463372698725, 62.78255861953126526 ) ) ;
#21237 = EDGE_CURVE ( 'NONE', #10202, #18022, #43132, .T. ) ;
#21238 = ORIENTED_EDGE ( 'NONE', *, *, #44578, .T. ) ;
#21239 = EDGE_LOOP ( 'NONE', ( #25619, #35829 ) ) ;
#21240 = AXIS2_PLACEMENT_3D ( 'NONE', #35913, #48217, #6380 ) ;
#21241 = CARTESIAN_POINT ( 'NONE',  ( -21.24416713127566325, -21.20535426119284139, 65.62808000370414163 ) ) ;
#21242 = CARTESIAN_POINT ( 'NONE',  ( -11.53247254227971830, -18.68106628708273931, 65.04707076447483871 ) ) ;
#21243 = VERTEX_POINT ( 'NONE', #43626 ) ;
#21244 = CARTESIAN_POINT ( 'NONE',  ( -11.83425018566923370, -19.11833757169930692, 68.37256453262955347 ) ) ;
#21246 = CARTESIAN_POINT ( 'NONE',  ( -10.50429924535250414, -16.15944446069506668, 71.46222527016213633 ) ) ;
#21245 = CARTESIAN_POINT ( 'NONE',  ( -17.98657259272421172, -21.83703102787368167, 62.16063850355641307 ) ) ;
#21247 = CARTESIAN_POINT ( 'NONE',  ( -12.91576191806997542, -9.388722997169708151, 71.13453240065665284 ) ) ;
#21248 = VECTOR ( 'NONE', #23954, 1000.000000000000000 ) ;
#21249 = FACE_OUTER_BOUND ( 'NONE', #33886, .T. ) ;
#21250 = CARTESIAN_POINT ( 'NONE',  ( -9.939267784769082681, -14.33236412611010913, 47.99999999999994316 ) ) ;
#21251 =( BOUNDED_CURVE ( )  B_SPLINE_CURVE ( 3, ( #25944, #14573, #40962, #29634 ),
 .UNSPECIFIED., .F., .F. ) 
 B_SPLINE_CURVE_WITH_KNOTS ( ( 4, 4 ),
 ( 0.000000000000000000, 0.4074455897393683412 ),
 .UNSPECIFIED. ) 
 CURVE ( )  GEOMETRIC_REPRESENTATION_ITEM ( )  RATIONAL_B_SPLINE_CURVE ( ( 1.000000000000000000, 0.4567392136813350767, 0.3561768502900314326, 0.6983129098260890677 ) ) 
 REPRESENTATION_ITEM ( '' )  );
#21252 = VERTEX_POINT ( 'NONE', #43389 ) ;
#21253 = CARTESIAN_POINT ( 'NONE',  ( -12.72102574358543059, -9.031338699541656467, 71.04936556502208589 ) ) ;
#21254 = FACE_OUTER_BOUND ( 'NONE', #35064, .T. ) ;
#21255 = VECTOR ( 'NONE', #18621, 1000.000000000000000 ) ;
#21256 = CARTESIAN_POINT ( 'NONE',  ( -16.94458744105653381, -7.374567917109038362, 74.14513580114275726 ) ) ;
#21257 = CARTESIAN_POINT ( 'NONE',  ( -14.87973245694827718, -7.806975737088362344, 56.98966612870860615 ) ) ;
#21258 = VERTEX_POINT ( 'NONE', #20966 ) ;
#21259 = FACE_OUTER_BOUND ( 'NONE', #16453, .T. ) ;
#21260 = CARTESIAN_POINT ( 'NONE',  ( -11.46875891826176819, -18.48806303968299858, 61.27710833525312495 ) ) ;
#21261 = ADVANCED_FACE ( 'NONE', ( #24905 ), #6185, .T. ) ;
#21262 = CARTESIAN_POINT ( 'NONE',  ( -24.41050200104759682, -17.39623818674726863, 69.61328578849980886 ) ) ;
#21263 = CARTESIAN_POINT ( 'NONE',  ( -20.80666424517567492, -21.44721877540349908, 58.80621670974001347 ) ) ;
#21264 = LINE ( 'NONE', #32806, #12625 ) ;
#21265 = CARTESIAN_POINT ( 'NONE',  ( -18.50517187854146783, -19.38160480531894336, 52.02966884056656482 ) ) ;
#21266 =( BOUNDED_SURFACE ( )  B_SPLINE_SURFACE ( 3, 1, ( 
 ( #37169, #26609 ),
 ( #749, #41627 ),
 ( #37413, #3710 ),
 ( #4435, #3455 ),
 ( #12074, #19215 ),
 ( #8376, #18712 ),
 ( #38154, #33725 ) ),
 .UNSPECIFIED., .T., .F., .F. ) 
 B_SPLINE_SURFACE_WITH_KNOTS ( ( 4, 3, 4 ),
 ( 2, 2 ),
 ( 0.000000000000000000, 0.5000000000000000000, 1.000000000000000000 ),
 ( 0.000000000000000000, 1.000000000000000000 ),
 .UNSPECIFIED. ) 
 GEOMETRIC_REPRESENTATION_ITEM ( )  RATIONAL_B_SPLINE_SURFACE ( (
 ( 1.000000000000000000, 1.000000000000000000),
 ( 0.3333333333333335369, 0.3333333333333330373),
 ( 0.3333333333333335369, 0.3333333333333330373),
 ( 1.000000000000000000, 1.000000000000000000),
 ( 0.3333333333333333703, 0.3333333333333333703),
 ( 0.3333333333333333703, 0.3333333333333333703),
 ( 1.000000000000000000, 1.000000000000000000) ) ) 
 REPRESENTATION_ITEM ( '' )  SURFACE ( )  );
#21267 = EDGE_LOOP ( 'NONE', ( #46399, #12022, #12539, #1262, #46101 ) ) ;
#21268 = ORIENTED_EDGE ( 'NONE', *, *, #26392, .T. ) ;
#21269 = CARTESIAN_POINT ( 'NONE',  ( -17.51784385541304090, -6.860780111191487229, 51.02154966934377001 ) ) ;
#21270 = LINE ( 'NONE', #2553, #22514 ) ;
#21271 = CLOSED_SHELL ( 'NONE', ( #7437, #13356, #693, #7100, #39212, #21040, #28639, #10554, #492, #17186, #32599 ) ) ;
#21272 = DIRECTION ( 'NONE',  ( -1.000000000000000000, -1.669677910507523057E-21, -6.493791346278465266E-22 ) ) ;
#21273 = DIRECTION ( 'NONE',  ( 0.9687793358424821033, -0.2479245821708677133, 0.000000000000000000 ) ) ;
#21274 = EDGE_CURVE ( 'NONE', #10355, #35561, #32529, .T. ) ;
#21275 = EDGE_CURVE ( 'NONE', #26071, #2695, #43342, .T. ) ;
#21276 = PLANE ( 'NONE',  #22273 ) ;
#21277 = ORIENTED_EDGE ( 'NONE', *, *, #28283, .T. ) ;
#21278 = VECTOR ( 'NONE', #37178, 1000.000000000000000 ) ;
#21279 = CARTESIAN_POINT ( 'NONE',  ( -11.02112013093993426, -11.00071374030268778, 60.77911540634885768 ) ) ;
#21280 = DIRECTION ( 'NONE',  ( 3.549360974554993999E-17, -6.371834667797928663E-18, -1.000000000000000000 ) ) ;
#21281 = ORIENTED_EDGE ( 'NONE', *, *, #31918, .T. ) ;
#21282 = CARTESIAN_POINT ( 'NONE',  ( -17.96252028288565228, -22.23973478741342902, 61.97512300109620043 ) ) ;
#21283 = CIRCLE ( 'NONE', #31502, 1.249999999999999334 ) ;
#21284 = CARTESIAN_POINT ( 'NONE',  ( -20.72409385541304161, -9.359200813967568422, 50.49621490985803263 ) ) ;
#21285 = ORIENTED_EDGE ( 'NONE', *, *, #42111, .T. ) ;
#21286 = EDGE_CURVE ( 'NONE', #24954, #26610, #6411, .T. ) ;
#21287 = EDGE_CURVE ( 'NONE', #9616, #30534, #24290, .T. ) ;
#21288 = CARTESIAN_POINT ( 'NONE',  ( -10.40860991809309155, -15.50898095412354571, 57.85320721669017985 ) ) ;
#21289 = ORIENTED_EDGE ( 'NONE', *, *, #19393, .F. ) ;
#21290 = CARTESIAN_POINT ( 'NONE',  ( -10.76458884141051975, -11.46785096862322995, 71.27516169247240896 ) ) ;
#21291 = EDGE_CURVE ( 'NONE', #29446, #32298, #32759, .T. ) ;
#21292 = CARTESIAN_POINT ( 'NONE',  ( -24.45563843384471880, -14.25946414430215903, 73.53760260359439371 ) ) ;
#21293 = AXIS2_PLACEMENT_3D ( 'NONE', #12018, #27754, #38333 ) ;
#21294 = EDGE_CURVE ( 'NONE', #18524, #23374, #37034, .T. ) ;
#21295 = CARTESIAN_POINT ( 'NONE',  ( -26.92409385541305511, -6.359206544744109735, 52.99999999999997158 ) ) ;
#21296 = CARTESIAN_POINT ( 'NONE',  ( -24.69519500507366061, -13.18560008479083123, 59.52301243476822634 ) ) ;
#21297 = ORIENTED_EDGE ( 'NONE', *, *, #42209, .F. ) ;
#21298 = CARTESIAN_POINT ( 'NONE',  ( -13.33011785382929304, -9.069340661520646663, 63.92418669539090814 ) ) ;
#21299 = CARTESIAN_POINT ( 'NONE',  ( -11.24165692237015968, -11.41328057087977044, 60.67885513026408262 ) ) ;
#21300 = DIRECTION ( 'NONE',  ( 0.3163880819683242973, 0.8528035521334695890, -0.4154812667942338611 ) ) ;
#21301 = CARTESIAN_POINT ( 'NONE',  ( -17.42409385541300182, -14.80920654474440745, 52.02966884056655061 ) ) ;
#21302 = CARTESIAN_POINT ( 'NONE',  ( -22.91784385650551670, -9.790100578890868377, 49.79778022625162492 ) ) ;
#21303 = EDGE_CURVE ( 'NONE', #42385, #21562, #6908, .T. ) ;
#21304 = AXIS2_PLACEMENT_3D ( 'NONE', #30623, #22745, #12134 ) ;
#21305 = CYLINDRICAL_SURFACE ( 'NONE', #9409, 1.250000000000001110 ) ;
#21306 = DIRECTION ( 'NONE',  ( 0.9687793358424821033, -0.2479245821708677133, 0.000000000000000000 ) ) ;
#21307 = ORIENTED_EDGE ( 'NONE', *, *, #40745, .T. ) ;
#21308 = CARTESIAN_POINT ( 'NONE',  ( -23.49605051889219709, -11.22618518380361152, 73.37665428612797314 ) ) ;
#21309 = DIRECTION ( 'NONE',  ( 0.000000000000000000, 0.000000000000000000, -1.000000000000000000 ) ) ;
#21310 = CARTESIAN_POINT ( 'NONE',  ( -9.999902751509219812, -15.43079746462003854, 57.72939317863753672 ) ) ;
#21311 = B_SPLINE_CURVE_WITH_KNOTS ( 'NONE', 3,
 ( #36463, #14286, #32778, #36688, #18237, #29092, #40649, #6928, #33244, #36945 ),
 .UNSPECIFIED., .F., .F.,
 ( 4, 2, 2, 2, 4 ),
 ( 0.6272669072878210850, 0.7522669073073205981, 0.8772669073268200002, 1.002266907346319513, 1.127266907365819026 ),
 .UNSPECIFIED. ) ;
#21312 = ORIENTED_EDGE ( 'NONE', *, *, #8682, .T. ) ;
#21313 = B_SPLINE_CURVE_WITH_KNOTS ( 'NONE', 3,
 ( #15302, #37969, #34268, #23216, #37470, #46100, #19265, #30369, #34770, #41921 ),
 .UNSPECIFIED., .F., .F.,
 ( 4, 2, 2, 2, 4 ),
 ( 0.6272669072877787855, 0.7522669073072940638, 0.8772669073268094531, 1.002266907346324842, 1.127266907365840121 ),
 .UNSPECIFIED. ) ;
#21314 = CARTESIAN_POINT ( 'NONE',  ( -40.92409385541305511, -15.80920654474410725, 74.99999999999998579 ) ) ;
#21315 = B_SPLINE_CURVE_WITH_KNOTS ( 'NONE', 1,
 ( #1725, #35440 ),
 .UNSPECIFIED., .F., .F.,
 ( 2, 2 ),
 ( 0.000000000000000000, 1.000000000000000000 ),
 .UNSPECIFIED. ) ;
#21316 = CIRCLE ( 'NONE', #34648, 4.686499999999997890 ) ;
#21317 = ORIENTED_EDGE ( 'NONE', *, *, #36915, .F. ) ;
#21318 = VERTEX_POINT ( 'NONE', #7169 ) ;
#21319 = ORIENTED_EDGE ( 'NONE', *, *, #43765, .F. ) ;
#21321 = DIRECTION ( 'NONE',  ( -5.731567514496413899E-31, -1.020425574103664789E-16, -1.000000000000000000 ) ) ;
#21320 = VECTOR ( 'NONE', #34412, 1000.000000000000000 ) ;
#21322 = CARTESIAN_POINT ( 'NONE',  ( -12.91491141960329792, -8.878583893719202536, 67.51909449892792736 ) ) ;
#21323 = CARTESIAN_POINT ( 'NONE',  ( -17.42409385541299471, -14.80920654474435594, 52.02966884056656482 ) ) ;
#21324 = CARTESIAN_POINT ( 'NONE',  ( -12.70616753690738143, -9.559812705026583757, 71.00492334522255078 ) ) ;
#21325 = EDGE_LOOP ( 'NONE', ( #44783, #7812, #12113, #18771 ) ) ;
#21326 = ORIENTED_EDGE ( 'NONE', *, *, #20266, .T. ) ;
#21327 = CARTESIAN_POINT ( 'NONE',  ( -17.49284385650551599, -7.406986770994973490, 48.81910596585309747 ) ) ;
#21328 = PLANE ( 'NONE',  #9524 ) ;
#21329 = CARTESIAN_POINT ( 'NONE',  ( -11.42622172434740158, -18.51434208396348069, 61.42710833180511543 ) ) ;
#21330 = EDGE_CURVE ( 'NONE', #39625, #47942, #9846, .T. ) ;
#21331 = CARTESIAN_POINT ( 'NONE',  ( -19.18034385650551599, -6.424090610841176385, 49.80797279389977916 ) ) ;
#21332 = ORIENTED_EDGE ( 'NONE', *, *, #34070, .F. ) ;
#21333 = EDGE_CURVE ( 'NONE', #112, #20093, #23605, .T. ) ;
#21334 = CARTESIAN_POINT ( 'NONE',  ( -10.99373011207215356, -17.70814896605071809, 68.30541983026010655 ) ) ;
#21335 = CARTESIAN_POINT ( 'NONE',  ( -24.87387917185663966, -14.87237230681592948, 59.35026067257155802 ) ) ;
#21336 =( BOUNDED_CURVE ( )  B_SPLINE_CURVE ( 3, ( #22901, #4184, #14979, #19679 ),
 .UNSPECIFIED., .F., .F. ) 
 B_SPLINE_CURVE_WITH_KNOTS ( ( 4, 4 ),
 ( 0.000000000000000000, 0.4074455897393624015 ),
 .UNSPECIFIED. ) 
 CURVE ( )  GEOMETRIC_REPRESENTATION_ITEM ( )  RATIONAL_B_SPLINE_CURVE ( ( 1.000000000000000000, 0.4567392136813315240, 0.3561768502900301003, 0.6983129098260958401 ) ) 
 REPRESENTATION_ITEM ( '' )  );
#21337 = ORIENTED_EDGE ( 'NONE', *, *, #48209, .T. ) ;
#21338 = CYLINDRICAL_SURFACE ( 'NONE', #31199, 5.249999999999998224 ) ;
#21339 = EDGE_LOOP ( 'NONE', ( #33532, #39445 ) ) ;
#21340 = MECHANICAL_DESIGN_GEOMETRIC_PRESENTATION_REPRESENTATION (  '', ( #6397 ), #3270 ) ;
#21341 = CARTESIAN_POINT ( 'NONE',  ( -10.52215064345839757, -13.37195933026064232, 74.82817647370434599 ) ) ;
#21342 = CARTESIAN_POINT ( 'NONE',  ( -16.28288173181390874, -21.71561457058961153, 58.30087945820258000 ) ) ;
#21343 = CARTESIAN_POINT ( 'NONE',  ( -18.59285626271963210, -7.848678033734123538, 67.05638626395584367 ) ) ;
#21344 = ADVANCED_FACE ( 'NONE', ( #7412 ), #29305, .T. ) ;
#21345 = AXIS2_PLACEMENT_3D ( 'NONE', #30289, #27061, #4661 ) ;
#21346 = ORIENTED_EDGE ( 'NONE', *, *, #20555, .T. ) ;
#21347 = FACE_OUTER_BOUND ( 'NONE', #2497, .T. ) ;
#21348 = EDGE_CURVE ( 'NONE', #25, #10344, #37162, .T. ) ;
#21349 = CARTESIAN_POINT ( 'NONE',  ( -18.46410521509267610, -21.78222384695268588, 72.29070755221093236 ) ) ;
#21350 = CYLINDRICAL_SURFACE ( 'NONE', #36255, 2.000000000000000000 ) ;
#21351 = EDGE_LOOP ( 'NONE', ( #19753, #16435, #46427, #13449 ) ) ;
#21352 = LINE ( 'NONE', #47448, #39332 ) ;
#21353 = AXIS2_PLACEMENT_3D ( 'NONE', #10123, #21457, #2722 ) ;
#21354 = CARTESIAN_POINT ( 'NONE',  ( -10.68602809008750576, -16.88409676349039046, 57.70232650191087487 ) ) ;
#21355 = ORIENTED_EDGE ( 'NONE', *, *, #43624, .F. ) ;
#21356 = CARTESIAN_POINT ( 'NONE',  ( -14.93108437845038594, -21.82978844404615160, 65.36242591972883531 ) ) ;
#21357 = CARTESIAN_POINT ( 'NONE',  ( -9.982716954774490503, -14.44908413001617298, 67.97304700561097945 ) ) ;
#21358 = ORIENTED_EDGE ( 'NONE', *, *, #6947, .T. ) ;
#21359 = CARTESIAN_POINT ( 'NONE',  ( -12.69763806180496601, -20.04058448603118592, 68.62185382311069759 ) ) ;
#21360 = CARTESIAN_POINT ( 'NONE',  ( -24.66206412712445939, -13.04441865846056103, 62.93289937805066359 ) ) ;
#21361 = CARTESIAN_POINT ( 'NONE',  ( -13.24261710015883864, -8.643249176123326549, 60.55454998173587455 ) ) ;
#21362 = CARTESIAN_POINT ( 'NONE',  ( -22.73036010286993047, -10.24127059135640039, 70.12251572578897196 ) ) ;
#21363 = EDGE_LOOP ( 'NONE', ( #31022, #15012, #11255, #31259, #25042 ) ) ;
#21364 = CARTESIAN_POINT ( 'NONE',  ( -22.01903099019451560, -9.527854123353398208, 60.00554641628053076 ) ) ;
#21365 = VECTOR ( 'NONE', #16522, 1000.000000000000000 ) ;
#21366 = EDGE_CURVE ( 'NONE', #24678, #39727, #29075, .T. ) ;
#21367 = CARTESIAN_POINT ( 'NONE',  ( -16.58751095051766455, -21.80939428823196025, 65.22564390318969174 ) ) ;
#21368 = CARTESIAN_POINT ( 'NONE',  ( -21.55883939963115026, -8.611815437115641458, 73.78624134823098757 ) ) ;
#21369 = VERTEX_POINT ( 'NONE', #22666 ) ;
#21370 = CARTESIAN_POINT ( 'NONE',  ( -22.10120296142702045, -17.19398125327358073, 49.52966884056655772 ) ) ;
#21371 = CARTESIAN_POINT ( 'NONE',  ( -12.32158608955787393, -9.943909642237139579, 60.57390139315987909 ) ) ;
#21373 = VERTEX_POINT ( 'NONE', #10606 ) ;
#21372 = CIRCLE ( 'NONE', #25304, 2.000000000000001776 ) ;
#21374 = ORIENTED_EDGE ( 'NONE', *, *, #43145, .F. ) ;
#21375 = CARTESIAN_POINT ( 'NONE',  ( -14.62110356098912511, -21.71197821782932991, 58.32651279851500448 ) ) ;
#21376 = DIRECTION ( 'NONE',  ( 0.7700094066334515208, 0.6380325334150288574, 0.000000000000000000 ) ) ;
#21377 = CARTESIAN_POINT ( 'NONE',  ( -13.21599742097365038, -20.46930908964682416, 58.46138952334620598 ) ) ;
#21378 = CARTESIAN_POINT ( 'NONE',  ( -23.83043773139750243, -11.86620498678314561, 59.78235732590890450 ) ) ;
#21379 = CARTESIAN_POINT ( 'NONE',  ( -19.41926759185595586, -7.631331631424885131, 60.16104200576716465 ) ) ;
#21380 = CARTESIAN_POINT ( 'NONE',  ( -21.20288680779426116, -21.22975277188588805, 65.68479702206012405 ) ) ;
#21381 = CARTESIAN_POINT ( 'NONE',  ( -12.45682740369385044, -20.36257741321750103, 68.45002181329043367 ) ) ;
#21382 = CARTESIAN_POINT ( 'NONE',  ( -20.31413516131974362, -8.378470924821744603, 67.06632013881642251 ) ) ;
#21383 = EDGE_LOOP ( 'NONE', ( #19729, #13705 ) ) ;
#21384 = ORIENTED_EDGE ( 'NONE', *, *, #43580, .F. ) ;
#21386 = CARTESIAN_POINT ( 'NONE',  ( -24.81704557732260952, -15.73545128243976521, 73.18959105933400622 ) ) ;
#21385 = STYLED_ITEM ( 'NONE', ( #1939 ), #32222 ) ;
#21387 = VECTOR ( 'NONE', #44698, 1000.000000000000114 ) ;
#21388 = DIRECTION ( 'NONE',  ( -0.7700094066334558507, -0.6380325334150236394, 0.000000000000000000 ) ) ;
#21389 = CARTESIAN_POINT ( 'NONE',  ( -10.63632956816940300, -16.72782611610072934, 57.98760696268571024 ) ) ;
#21390 = CARTESIAN_POINT ( 'NONE',  ( -12.20309422964675150, -20.12380354524033521, 64.98179449731530610 ) ) ;
#21391 = CARTESIAN_POINT ( 'NONE',  ( -10.18401502636761968, -13.05277926903019470, 71.32333192088977114 ) ) ;
#21392 =( BOUNDED_CURVE ( )  B_SPLINE_CURVE ( 3, ( #46284, #16211, #43062, #35179 ),
 .UNSPECIFIED., .F., .F. ) 
 B_SPLINE_CURVE_WITH_KNOTS ( ( 4, 4 ),
 ( 0.000000000000000000, 0.4074455897393596260 ),
 .UNSPECIFIED. ) 
 CURVE ( )  GEOMETRIC_REPRESENTATION_ITEM ( )  RATIONAL_B_SPLINE_CURVE ( ( 1.000000000000000000, 0.4567392136813429593, 0.3561768502900343747, 0.6983129098260744128 ) ) 
 REPRESENTATION_ITEM ( '' )  );
#21393 = EDGE_CURVE ( 'NONE', #4575, #28527, #6668, .T. ) ;
#21394 = CARTESIAN_POINT ( 'NONE',  ( -18.98034385650551670, -6.424090610841176385, 49.80797279389977916 ) ) ;
#21395 = VERTEX_POINT ( 'NONE', #47786 ) ;
#21396 = CARTESIAN_POINT ( 'NONE',  ( -14.84927081153347039, -21.37251255130113137, 61.65072491673618771 ) ) ;
#21397 = CARTESIAN_POINT ( 'NONE',  ( -23.98985609448851264, -11.28854004645977582, 66.54401757043002874 ) ) ;
#21398 = CARTESIAN_POINT ( 'NONE',  ( -10.46944733747312917, -15.96661384539355133, 67.99239968927004441 ) ) ;
#21399 = ORIENTED_EDGE ( 'NONE', *, *, #26052, .T. ) ;
#21400 =( BOUNDED_SURFACE ( )  B_SPLINE_SURFACE ( 3, 1, ( 
 ( #18611, #33623 ),
 ( #14908, #13103 ),
 ( #43168, #31841 ),
 ( #24935, #31603 ),
 ( #10161, #32334 ),
 ( #47590, #46862 ),
 ( #21247, #20757 ) ),
 .UNSPECIFIED., .T., .F., .F. ) 
 B_SPLINE_SURFACE_WITH_KNOTS ( ( 4, 3, 4 ),
 ( 2, 2 ),
 ( 0.000000000000000000, 0.5000000000000000000, 1.000000000000000000 ),
 ( 0.000000000000000000, 1.000000000000000000 ),
 .UNSPECIFIED. ) 
 GEOMETRIC_REPRESENTATION_ITEM ( )  RATIONAL_B_SPLINE_SURFACE ( (
 ( 1.000000000000000000, 1.000000000000000000),
 ( 0.3333333333333335369, 0.3333333333333330373),
 ( 0.3333333333333335369, 0.3333333333333330373),
 ( 1.000000000000000000, 1.000000000000000000),
 ( 0.3333333333333333703, 0.3333333333333333703),
 ( 0.3333333333333333703, 0.3333333333333333703),
 ( 1.000000000000000000, 1.000000000000000000) ) ) 
 REPRESENTATION_ITEM ( '' )  SURFACE ( )  );
#21401 = B_SPLINE_CURVE_WITH_KNOTS ( 'NONE', 3,
 ( #26677, #37737, #41435, #8698, #16051, #7732, #22747, #31090, #8212, #811 ),
 .UNSPECIFIED., .F., .F.,
 ( 4, 2, 2, 2, 4 ),
 ( 0.1272669073658901084, 0.2522669073439965937, 0.3772669073221031066, 0.5022669073002096196, 0.6272669072783161326 ),
 .UNSPECIFIED. ) ;
#21402 = LINE ( 'NONE', #47974, #47949 ) ;
#21403 = CARTESIAN_POINT ( 'NONE',  ( -22.07864594086649390, -14.26292169798353981, 49.52966884056655772 ) ) ;
#21404 = ADVANCED_FACE ( 'NONE', ( #14267, #14024 ), #11096, .F. ) ;
#21405 = FACE_OUTER_BOUND ( 'NONE', #5365, .T. ) ;
#21406 = EDGE_CURVE ( 'NONE', #33162, #15971, #34466, .T. ) ;
#21407 = CARTESIAN_POINT ( 'NONE',  ( -20.72573862760241070, -8.580110178657996300, 60.14125250079694496 ) ) ;
#21408 = VERTEX_POINT ( 'NONE', #14499 ) ;
#21409 = CARTESIAN_POINT ( 'NONE',  ( -22.99015624685222292, -19.05428196339609315, 58.88410607238818528 ) ) ;
#21410 =( BOUNDED_SURFACE ( )  B_SPLINE_SURFACE ( 3, 1, ( 
 ( #18279, #6735 ),
 ( #21749, #15069 ),
 ( #29382, #45382 ),
 ( #44414, #26180 ),
 ( #33285, #11634 ),
 ( #22738, #40457 ),
 ( #18034, #10669 ) ),
 .UNSPECIFIED., .T., .F., .F. ) 
 B_SPLINE_SURFACE_WITH_KNOTS ( ( 4, 3, 4 ),
 ( 2, 2 ),
 ( 0.000000000000000000, 0.5000000000000000000, 1.000000000000000000 ),
 ( 0.000000000000000000, 1.000000000000000000 ),
 .UNSPECIFIED. ) 
 GEOMETRIC_REPRESENTATION_ITEM ( )  RATIONAL_B_SPLINE_SURFACE ( (
 ( 1.000000000000000000, 1.000000000000000000),
 ( 0.3333333333333335369, 0.3333333333333330373),
 ( 0.3333333333333335369, 0.3333333333333330373),
 ( 1.000000000000000000, 1.000000000000000000),
 ( 0.3333333333333333703, 0.3333333333333333703),
 ( 0.3333333333333333703, 0.3333333333333333703),
 ( 1.000000000000000000, 1.000000000000000000) ) ) 
 REPRESENTATION_ITEM ( '' )  SURFACE ( )  );
#21411 = ORIENTED_EDGE ( 'NONE', *, *, #4389, .T. ) ;
#21412 = CARTESIAN_POINT ( 'NONE',  ( -16.06904265174829405, -7.890656434512189676, 63.82011029958098192 ) ) ;
#21413 = CARTESIAN_POINT ( 'NONE',  ( -14.68034385759798965, -9.360768649639304329, 51.01397948905922419 ) ) ;
#21414 = ADVANCED_FACE ( 'NONE', ( #29555 ), #37786, .T. ) ;
#21415 = VERTEX_POINT ( 'NONE', #9285 ) ;
#21416 = DIRECTION ( 'NONE',  ( 3.071710424422018668E-17, -6.404604876783312462E-16, -1.000000000000000000 ) ) ;
#21417 = CARTESIAN_POINT ( 'NONE',  ( -14.56784385650551705, -6.428312510596451368, 51.20221977374900035 ) ) ;
#21418 = VECTOR ( 'NONE', #37277, 1000.000000000000114 ) ;
#21419 = ORIENTED_EDGE ( 'NONE', *, *, #17024, .F. ) ;
#21420 = CARTESIAN_POINT ( 'NONE',  ( -18.75616561686623740, -7.937006977771949856, 70.37068081711387890 ) ) ;
#21421 = ADVANCED_FACE ( 'NONE', ( #20367 ), #24310, .T. ) ;
#21422 = EDGE_CURVE ( 'NONE', #34511, #26563, #16159, .T. ) ;
#21423 = CARTESIAN_POINT ( 'NONE',  ( -24.72409385541305582, -14.80920654474418896, 65.04705882352939739 ) ) ;
#21424 = CARTESIAN_POINT ( 'NONE',  ( -17.42409385541299471, -14.80920654474435771, 49.52966884056655772 ) ) ;
#21425 = ORIENTED_EDGE ( 'NONE', *, *, #43452, .F. ) ;
#21426 = DIRECTION ( 'NONE',  ( 0.9997277805376393323, -0.02333162706040292980, -9.101776391673710038E-09 ) ) ;
#21427 = PLANE ( 'NONE',  #7010 ) ;
#21428 = CARTESIAN_POINT ( 'NONE',  ( -10.64854695470030599, -12.86019059820356780, 64.55364013863997741 ) ) ;
#21429 = DIRECTION ( 'NONE',  ( 7.357566626357555830E-06, 1.068273751274826037E-05, -0.9999999999158726283 ) ) ;
#21430 = EDGE_LOOP ( 'NONE', ( #586, #16862, #20681, #7567, #11083 ) ) ;
#21431 = ORIENTED_EDGE ( 'NONE', *, *, #30733, .F. ) ;
#21432 = CARTESIAN_POINT ( 'NONE',  ( -24.17067115178138081, -16.86763775777920316, 73.09156006070151079 ) ) ;
#21433 = CARTESIAN_POINT ( 'NONE',  ( -24.22652117640109992, -16.69121458274543102, 59.26765574801870429 ) ) ;
#21434 = VERTEX_POINT ( 'NONE', #9537 ) ;
#21435 = CARTESIAN_POINT ( 'NONE',  ( -10.44250057104172669, -15.78999660075996836, 64.51331401163844248 ) ) ;
#21436 = CARTESIAN_POINT ( 'NONE',  ( -19.74284385759798965, -7.587656875400192291, 49.25157356644813689 ) ) ;
#21437 = DIRECTION ( 'NONE',  ( 0.4639960340712823705, -0.8858372764600287441, 1.924356585498154222E-16 ) ) ;
#21438 = CARTESIAN_POINT ( 'NONE',  ( -16.92322068952146807, -21.79132391646259848, 68.76848671744031094 ) ) ;
#21439 = DIRECTION ( 'NONE',  ( 0.9687793358424821033, -0.2479245821708677133, 0.000000000000000000 ) ) ;
#21440 = EDGE_CURVE ( 'NONE', #31120, #38065, #12486, .T. ) ;
#21441 = VERTEX_POINT ( 'NONE', #34886 ) ;
#21442 = B_SPLINE_CURVE_WITH_KNOTS ( 'NONE', 1,
 ( #36075, #2356 ),
 .UNSPECIFIED., .F., .F.,
 ( 2, 2 ),
 ( 0.000000000000000000, 1.000000000000000000 ),
 .UNSPECIFIED. ) ;
#21443 = CARTESIAN_POINT ( 'NONE',  ( -11.89203589379550685, -19.18525226774134396, 71.89505619424038230 ) ) ;
#21444 = FACE_OUTER_BOUND ( 'NONE', #40473, .T. ) ;
#21445 = CARTESIAN_POINT ( 'NONE',  ( -10.79572390357762046, -11.40795830647630282, 67.80360014157953685 ) ) ;
#21446 = ADVANCED_FACE ( 'NONE', ( #31202 ), #41240, .T. ) ;
#21447 = ORIENTED_EDGE ( 'NONE', *, *, #40709, .F. ) ;
#21448 = VERTEX_POINT ( 'NONE', #27747 ) ;
#21449 = CARTESIAN_POINT ( 'NONE',  ( -20.66570527118851786, -8.604879590079393736, 60.14125219010794154 ) ) ;
#21450 = CARTESIAN_POINT ( 'NONE',  ( -10.00661911024752726, -14.11250400273905470, 61.04008521068034554 ) ) ;
#21451 = DIRECTION ( 'NONE',  ( 1.000000000000000000, -4.164305804376849172E-17, 1.614929280266638808E-16 ) ) ;
#21452 = EDGE_LOOP ( 'NONE', ( #36436, #6400, #43974, #39539 ) ) ;
#21453 = ADVANCED_FACE ( 'NONE', ( #42777 ), #699, .T. ) ;
#21454 = CARTESIAN_POINT ( 'NONE',  ( -16.24510065014822047, -7.452919174226901866, 60.36175022640202315 ) ) ;
#21455 = CARTESIAN_POINT ( 'NONE',  ( -23.77560840941285036, -17.75199072401120404, 59.00378408732571955 ) ) ;
#21456 = VERTEX_POINT ( 'NONE', #41621 ) ;
#21457 = DIRECTION ( 'NONE',  ( 1.000000000000000000, 0.000000000000000000, -2.406186529621654018E-16 ) ) ;
#21458 = CARTESIAN_POINT ( 'NONE',  ( -12.56172001024846452, -20.45377019276184427, 71.99149100736865137 ) ) ;
#21459 = EDGE_LOOP ( 'NONE', ( #42986, #44122, #29689, #2520 ) ) ;
#21460 = CARTESIAN_POINT ( 'NONE',  ( -28.42409385541305511, -6.859206544744110623, 47.99999999999997868 ) ) ;
#21461 = ORIENTED_EDGE ( 'NONE', *, *, #26182, .F. ) ;
#21462 = CARTESIAN_POINT ( 'NONE',  ( -24.34502386579654498, -17.56683345968398768, 66.12852568699506151 ) ) ;
#21463 = FACE_OUTER_BOUND ( 'NONE', #16744, .T. ) ;
#21464 = ADVANCED_FACE ( 'NONE', ( #39557 ), #40288, .T. ) ;
#21465 = CARTESIAN_POINT ( 'NONE',  ( -19.49109506855409180, -21.54969648977046148, 62.28031529404344013 ) ) ;
#21466 = ORIENTED_EDGE ( 'NONE', *, *, #30189, .F. ) ;
#21467 = CARTESIAN_POINT ( 'NONE',  ( -21.41609786863869758, -21.09944828077204804, 69.16111856145751347 ) ) ;
#21468 = LINE ( 'NONE', #43886, #37567 ) ;
#21469 = VECTOR ( 'NONE', #44905, 1000.000000000000114 ) ;
#21470 = CARTESIAN_POINT ( 'NONE',  ( -15.16142571637111303, -21.90729309775286282, 68.72592917306566562 ) ) ;
#21471 = ADVANCED_FACE ( 'NONE', ( #21090 ), #47195, .F. ) ;
#21472 = B_SPLINE_CURVE_WITH_KNOTS ( 'NONE', 1,
 ( #13149, #43470 ),
 .UNSPECIFIED., .F., .F.,
 ( 2, 2 ),
 ( 0.000000000000000000, 1.000000000000000000 ),
 .UNSPECIFIED. ) ;
#21473 = CARTESIAN_POINT ( 'NONE',  ( -24.86601949095794239, -14.46076817688473071, 66.43938638393159124 ) ) ;
#21474 = CARTESIAN_POINT ( 'NONE',  ( -14.11784385759799143, -6.860780111191492558, 51.02154966934379132 ) ) ;
#21475 = CARTESIAN_POINT ( 'NONE',  ( -16.58751391467172098, -21.80939466075598077, 65.52564390317479592 ) ) ;
#21476 = EDGE_LOOP ( 'NONE', ( #5820, #40011, #19992, #7421, #2874 ) ) ;
#21477 = CARTESIAN_POINT ( 'NONE',  ( -23.80321465417087978, -17.81075909821204917, 59.15378417737379380 ) ) ;
#21478 = CARTESIAN_POINT ( 'NONE',  ( -16.84865286310842336, -21.83598151670433296, 68.98088545748413480 ) ) ;
#21479 = CARTESIAN_POINT ( 'NONE',  ( -22.68646480449111635, -20.08284195570847430, 69.35913425646373298 ) ) ;
#21480 = CARTESIAN_POINT ( 'NONE',  ( -13.60236376389480384, -20.73382277062339085, 61.80174179654961364 ) ) ;
#21481 = FACE_OUTER_BOUND ( 'NONE', #32258, .T. ) ;
#21482 = CARTESIAN_POINT ( 'NONE',  ( -14.19909385650551847, -8.114302828567740988, 52.18300498402516041 ) ) ;
#21483 = ORIENTED_EDGE ( 'NONE', *, *, #30646, .T. ) ;
#21484 = ORIENTED_EDGE ( 'NONE', *, *, #32280, .F. ) ;
#21485 = CARTESIAN_POINT ( 'NONE',  ( -17.56955047399654646, -7.310617185930959216, 53.27966884056655061 ) ) ;
#21486 = LINE ( 'NONE', #27897, #1385 ) ;
#21487 = ORIENTED_EDGE ( 'NONE', *, *, #12834, .F. ) ;
#21488 = CARTESIAN_POINT ( 'NONE',  ( -36.42409385541304800, -8.109206544743658540, 50.50000000000030553 ) ) ;
#21490 = CARTESIAN_POINT ( 'NONE',  ( -13.61159385650551457, -6.922745924619793101, 51.69366785382590024 ) ) ;
#21489 = CARTESIAN_POINT ( 'NONE',  ( -10.13258914451759019, -16.33817228489381179, 71.63245656337019796 ) ) ;
#21491 = CARTESIAN_POINT ( 'NONE',  ( -24.19351282280050341, -13.02564333272532515, 66.58630226542909725 ) ) ;
#21492 = CARTESIAN_POINT ( 'NONE',  ( -19.37484727228654080, -7.619050864103940057, 60.14588289477547534 ) ) ;
#21493 = LINE ( 'NONE', #3485, #28960 ) ;
#21494 = CARTESIAN_POINT ( 'NONE',  ( -12.41315146567208139, -9.850077947585075933, 57.08935532239181754 ) ) ;
#21495 = EDGE_CURVE ( 'NONE', #32931, #11764, #42834, .T. ) ;
#21496 = CARTESIAN_POINT ( 'NONE',  ( -12.32278866559117780, -19.67576434477648917, 61.41150688479135766 ) ) ;
#21497 = DIRECTION ( 'NONE',  ( -3.159776991290051445E-16, -1.000000000000000000, -6.457808579236824910E-31 ) ) ;
#21498 = EDGE_CURVE ( 'NONE', #6432, #47754, #898, .T. ) ;
#21499 = DIRECTION ( 'NONE',  ( 2.866981220435666553E-17, -1.000000000000000000, -1.190614954331866791E-16 ) ) ;
#21500 = CARTESIAN_POINT ( 'NONE',  ( -14.82200063897825970, -7.828394103733741005, 57.04988785029721754 ) ) ;
#21501 = EDGE_CURVE ( 'NONE', #24601, #16655, #35903, .T. ) ;
#21502 = EDGE_CURVE ( 'NONE', #34949, #28014, #6313, .T. ) ;
#21503 = ORIENTED_EDGE ( 'NONE', *, *, #7793, .T. ) ;
#21504 = CARTESIAN_POINT ( 'NONE',  ( 18.57590614458706924, 1.890747609047893185, 50.53028072113869484 ) ) ;
#21505 = DIRECTION ( 'NONE',  ( -5.731567514496413899E-31, -1.020425574103664789E-16, -1.000000000000000000 ) ) ;
#21506 = DIRECTION ( 'NONE',  ( 1.224646799147353207E-16, 1.000000000000000000, -1.912410701131276611E-32 ) ) ;
#21507 = CARTESIAN_POINT ( 'NONE',  ( -21.02642564228531441, -20.81301427019056760, 69.16523372085018195 ) ) ;
#21508 = DIRECTION ( 'NONE',  ( 3.413470714839332458E-33, -1.190614954331866791E-16, 1.000000000000000000 ) ) ;
#21509 = DIRECTION ( 'NONE',  ( 0.2664710960620865765, -0.9638429098994649724, 4.833213314675752896E-08 ) ) ;
#21510 = ORIENTED_EDGE ( 'NONE', *, *, #2472, .F. ) ;
#21511 = ORIENTED_EDGE ( 'NONE', *, *, #23888, .F. ) ;
#21512 = CARTESIAN_POINT ( 'NONE',  ( -16.95534385541304445, -8.623186033802570094, 49.24843789510466507 ) ) ;
#21513 = ORIENTED_EDGE ( 'NONE', *, *, #36711, .T. ) ;
#21514 = CARTESIAN_POINT ( 'NONE',  ( -14.92898057683877155, -8.215345490092026637, 57.14440235176596161 ) ) ;
#21515 = VECTOR ( 'NONE', #10390, 1000.000000000000114 ) ;
#21516 = CARTESIAN_POINT ( 'NONE',  ( -11.64187585391237612, -10.11031112578646152, 67.61241562450165077 ) ) ;
#21517 = B_SPLINE_CURVE_WITH_KNOTS ( 'NONE', 1,
 ( #10608, #37919 ),
 .UNSPECIFIED., .F., .F.,
 ( 2, 2 ),
 ( 0.000000000000000000, 1.000000000000000000 ),
 .UNSPECIFIED. ) ;
#21518 = DIRECTION ( 'NONE',  ( -3.071710424422018668E-17, 6.404604876783312462E-16, 1.000000000000000000 ) ) ;
#21519 = EDGE_CURVE ( 'NONE', #17620, #9150, #2843, .T. ) ;
#21520 = LINE ( 'NONE', #14087, #21469 ) ;
#21521 = ORIENTED_EDGE ( 'NONE', *, *, #21741, .T. ) ;
#21522 = CARTESIAN_POINT ( 'NONE',  ( -20.12289122552838094, -7.865124802246414859, 73.90591932823114973 ) ) ;
#21523 = FACE_OUTER_BOUND ( 'NONE', #27089, .T. ) ;
#21524 =( BOUNDED_CURVE ( )  B_SPLINE_CURVE ( 3, ( #46916, #4290, #48602, #45415 ),
 .UNSPECIFIED., .F., .F. ) 
 B_SPLINE_CURVE_WITH_KNOTS ( ( 4, 4 ),
 ( 0.000000000000000000, 0.4074455897393559622 ),
 .UNSPECIFIED. ) 
 CURVE ( )  GEOMETRIC_REPRESENTATION_ITEM ( )  RATIONAL_B_SPLINE_CURVE ( ( 1.000000000000000000, 0.4567392136813420711, 0.3561768502900340416, 0.6983129098260760781 ) ) 
 REPRESENTATION_ITEM ( '' )  );
#21525 = ORIENTED_EDGE ( 'NONE', *, *, #45324, .F. ) ;
#21526 = DIRECTION ( 'NONE',  ( -0.3037135924646502394, 0.9527633776296274837, 2.170275161112374562E-08 ) ) ;
#21527 = CARTESIAN_POINT ( 'NONE',  ( -20.49909385541303308, -8.105421454601382081, 49.25000573077638677 ) ) ;
#21528 = ORIENTED_EDGE ( 'NONE', *, *, #9830, .T. ) ;
#21529 = CARTESIAN_POINT ( 'NONE',  ( -19.64401462542318200, -21.92156298671864434, 62.10848288909245696 ) ) ;
#21530 = CARTESIAN_POINT ( 'NONE',  ( -16.74780546227259848, -22.22844731805369278, 68.84560649934257981 ) ) ;
#21531 = CARTESIAN_POINT ( 'NONE',  ( -17.42409385541299471, -14.80920654474434883, 62.02966884056656482 ) ) ;
#21532 = ORIENTED_EDGE ( 'NONE', *, *, #8453, .F. ) ;
#21533 = FACE_OUTER_BOUND ( 'NONE', #20713, .T. ) ;
#21534 = DIRECTION ( 'NONE',  ( 2.866981220435666553E-17, -1.000000000000000000, -1.190614954331866791E-16 ) ) ;
#21535 =( BOUNDED_CURVE ( )  B_SPLINE_CURVE ( 2, ( #20364, #43007, #1156, #9284, #20118, #42291, #1391, #16408, #38584 ),
 .UNSPECIFIED., .F., .F. ) 
 B_SPLINE_CURVE_WITH_KNOTS ( ( 3, 2, 2, 2, 3 ),
 ( 0.01966989284433012450, 0.02065350756516602312, 0.02163712228600192522, 0.02262073700683782732, 0.02360435172767372594 ),
 .UNSPECIFIED. ) 
 CURVE ( )  GEOMETRIC_REPRESENTATION_ITEM ( )  RATIONAL_B_SPLINE_CURVE ( ( 0.9999999999999663602, 0.9238795325113203782, 1.000000000000000000, 0.9238795325112867385, 1.000000000000000000, 0.9238795325112867385, 1.000000000000000000, 0.9238795325112295620, 1.000000000000057288 ) ) 
 REPRESENTATION_ITEM ( '' )  );
#21536 = CARTESIAN_POINT ( 'NONE',  ( -24.70317136920038337, -13.22248578388119000, 59.46244285080189940 ) ) ;
#21537 = VERTEX_POINT ( 'NONE', #28485 ) ;
#21538 =( BOUNDED_CURVE ( )  B_SPLINE_CURVE ( 3, ( #22130, #18649, #45041, #18913 ),
 .UNSPECIFIED., .F., .F. ) 
 B_SPLINE_CURVE_WITH_KNOTS ( ( 4, 4 ),
 ( 0.9074455897393695070, 1.000000000000000000 ),
 .UNSPECIFIED. ) 
 CURVE ( )  GEOMETRIC_REPRESENTATION_ITEM ( )  RATIONAL_B_SPLINE_CURVE ( ( 0.6983129098261253720, 0.7760317562607260689, 0.8765941196520176115, 1.000000000000000000 ) ) 
 REPRESENTATION_ITEM ( '' )  );
#21539 = FACE_OUTER_BOUND ( 'NONE', #41277, .T. ) ;
#21540 = CARTESIAN_POINT ( 'NONE',  ( -12.00532783130394776, -19.33158900886926546, 58.07115174146640157 ) ) ;
#21541 = CARTESIAN_POINT ( 'NONE',  ( -10.78898398081525301, -17.19290454168847404, 61.44271037915215317 ) ) ;
#21542 = VECTOR ( 'NONE', #35267, 1000.000000000000000 ) ;
#21543 = DIRECTION ( 'NONE',  ( 0.9959323210854038599, -0.09010444948746666738, -2.601165157765165743E-08 ) ) ;
#21544 = CARTESIAN_POINT ( 'NONE',  ( -24.68345461824787890, -13.13130818398968103, 59.47612521039077649 ) ) ;
#21545 = EDGE_LOOP ( 'NONE', ( #21192, #34841, #22552, #22614 ) ) ;
#21546 = CARTESIAN_POINT ( 'NONE',  ( -18.48325495428488807, -7.889676674725549788, 73.84064351486135536 ) ) ;
#21547 = DIRECTION ( 'NONE',  ( 0.9687793358424821033, -0.2479245821708680464, 0.000000000000000000 ) ) ;
#21548 = B_SPLINE_CURVE_WITH_KNOTS ( 'NONE', 1,
 ( #13386, #42729 ),
 .UNSPECIFIED., .F., .F.,
 ( 2, 2 ),
 ( 0.000000000000000000, 1.000000000000000000 ),
 .UNSPECIFIED. ) ;
#21549 = EDGE_LOOP ( 'NONE', ( #47565, #27723, #8623, #11625, #40407 ) ) ;
#21550 = CARTESIAN_POINT ( 'NONE',  ( 18.82590614458706924, 1.890747609047893185, 50.53028072113869484 ) ) ;
#21551 =( BOUNDED_CURVE ( )  B_SPLINE_CURVE ( 3, ( #21475, #7428, #14761, #40183 ),
 .UNSPECIFIED., .F., .F. ) 
 B_SPLINE_CURVE_WITH_KNOTS ( ( 4, 4 ),
 ( 0.9074455897393642889, 1.000000000000000000 ),
 .UNSPECIFIED. ) 
 CURVE ( )  GEOMETRIC_REPRESENTATION_ITEM ( )  RATIONAL_B_SPLINE_CURVE ( ( 0.6983129098260967282, 0.7760317562607014219, 0.8765941196520025125, 1.000000000000000000 ) ) 
 REPRESENTATION_ITEM ( '' )  );
#21552 = ORIENTED_EDGE ( 'NONE', *, *, #43261, .F. ) ;
#21553 = EDGE_CURVE ( 'NONE', #20596, #15704, #34324, .T. ) ;
#21554 = ADVANCED_FACE ( 'NONE', ( #13671 ), #44003, .T. ) ;
#21555 = VERTEX_POINT ( 'NONE', #44242 ) ;
#21556 = ORIENTED_EDGE ( 'NONE', *, *, #24334, .F. ) ;
#21557 = CARTESIAN_POINT ( 'NONE',  ( -18.89230742602834923, -7.910091329180813702, 63.63909002588712127 ) ) ;
#21558 = CARTESIAN_POINT ( 'NONE',  ( -12.85294938858001501, -8.926356163590522641, 67.57216919348684314 ) ) ;
#21559 = DIRECTION ( 'NONE',  ( 0.7971031148784507581, -0.6038432116460916710, 6.916509187980650173E-08 ) ) ;
#21560 = CARTESIAN_POINT ( 'NONE',  ( -11.89178972046640936, -10.43929686452144878, 71.11893105542935700 ) ) ;
#21561 = VERTEX_POINT ( 'NONE', #25273 ) ;
#21562 = VERTEX_POINT ( 'NONE', #21807 ) ;
#21563 = EDGE_CURVE ( 'NONE', #11264, #25709, #28718, .T. ) ;
#21564 = ADVANCED_FACE ( 'NONE', ( #43750 ), #36334, .T. ) ;
#21565 = CARTESIAN_POINT ( 'NONE',  ( -18.61784385650552309, -9.790100578890868377, 49.79778022625163203 ) ) ;
#21566 = B_SPLINE_CURVE_WITH_KNOTS ( 'NONE', 3,
 ( #26874, #19720, #12319, #31044, #19463, #37684, #12085, #1002, #11847, #15266 ),
 .UNSPECIFIED., .F., .F.,
 ( 4, 2, 2, 2, 4 ),
 ( 0.6272669072964546233, 0.7522669073137989715, 0.8772669073311434307, 1.002266907348487779, 1.127266907365832127 ),
 .UNSPECIFIED. ) ;
#21567 = CYLINDRICAL_SURFACE ( 'NONE', #5588, 5.249999999999998224 ) ;
#21568 = CARTESIAN_POINT ( 'NONE',  ( -12.60227155074094441, -19.95281705956671559, 68.35129494334645983 ) ) ;
#21569 = CARTESIAN_POINT ( 'NONE',  ( -18.44909385650551670, -8.104110260919579645, 48.81699501597546487 ) ) ;
#21570 = ORIENTED_EDGE ( 'NONE', *, *, #24890, .T. ) ;
#21571 = ADVANCED_FACE ( 'NONE', ( #13910 ), #21579, .T. ) ;
#21572 = CARTESIAN_POINT ( 'NONE',  ( -45.92409385541306932, -16.43194983366105077, 71.05609102496107710 ) ) ;
#21573 = VECTOR ( 'NONE', #21426, 999.9999999999998863 ) ;
#21574 = CARTESIAN_POINT ( 'NONE',  ( -24.79803955827340545, -15.87155823828966561, 69.78953433284350183 ) ) ;
#21575 = ORIENTED_EDGE ( 'NONE', *, *, #35314, .T. ) ;
#21576 = CARTESIAN_POINT ( 'NONE',  ( -4.424093855413053333, -6.859206544744110623, 63.99999999999998579 ) ) ;
#21577 = B_SPLINE_CURVE_WITH_KNOTS ( 'NONE', 1,
 ( #47282, #32495 ),
 .UNSPECIFIED., .F., .F.,
 ( 2, 2 ),
 ( 0.000000000000000000, 1.000000000000000000 ),
 .UNSPECIFIED. ) ;
#21578 = VERTEX_POINT ( 'NONE', #34097 ) ;
#21579 = PLANE ( 'NONE',  #12699 ) ;
#21580 = CARTESIAN_POINT ( 'NONE',  ( -18.17450532280264142, -21.77015438960330229, 69.04344613823298005 ) ) ;
#21581 = CARTESIAN_POINT ( 'NONE',  ( -21.53227841957539113, -21.02428511524863097, 72.64729568458159292 ) ) ;
#21582 = EDGE_LOOP ( 'NONE', ( #37260, #12038, #14358, #38074 ) ) ;
#21583 = DIRECTION ( 'NONE',  ( -3.071710424422018668E-17, 6.404604876783312462E-16, 1.000000000000000000 ) ) ;
#21584 = CARTESIAN_POINT ( 'NONE',  ( -23.01445215836851688, -10.50074233538543211, 66.68615203886294296 ) ) ;
#21585 = CARTESIAN_POINT ( 'NONE',  ( -12.05483428091225129, -10.31798718066989551, 67.49896870046983111 ) ) ;
#21586 = VERTEX_POINT ( 'NONE', #18342 ) ;
#21587 = CARTESIAN_POINT ( 'NONE',  ( -20.76359895218475060, -20.96132515946565888, 58.87148521899143816 ) ) ;
#21588 = CARTESIAN_POINT ( 'NONE',  ( -21.55884032038934350, -8.611816057827914150, 73.78624026056009200 ) ) ;
#21589 = CARTESIAN_POINT ( 'NONE',  ( -17.42409385541300892, -14.80920654474439679, 56.49999999999994316 ) ) ;
#21590 = EDGE_LOOP ( 'NONE', ( #36535, #14605, #19359, #28681 ) ) ;
#21591 = CARTESIAN_POINT ( 'NONE',  ( -13.35818949714929360, -21.05197827947291955, 61.70141596610112344 ) ) ;
#21592 = ORIENTED_EDGE ( 'NONE', *, *, #14205, .F. ) ;
#21593 = CYLINDRICAL_SURFACE ( 'NONE', #34443, 0.1500000000000084044 ) ;
#21594 = CARTESIAN_POINT ( 'NONE',  ( -24.82750195234013191, -13.97654432178796569, 73.30766915316792165 ) ) ;
#21595 = CARTESIAN_POINT ( 'NONE',  ( -19.80301194551662647, -21.44571530912114099, 68.93482476707502826 ) ) ;
#21596 = B_SPLINE_CURVE_WITH_KNOTS ( 'NONE', 1,
 ( #11872, #11619 ),
 .UNSPECIFIED., .F., .F.,
 ( 2, 2 ),
 ( 0.000000000000000000, 1.000000000000000000 ),
 .UNSPECIFIED. ) ;
#21597 = DIRECTION ( 'NONE',  ( -0.3478314405900309603, -0.9375570856950864451, 9.567072274253697654E-17 ) ) ;
#21598 = ORIENTED_EDGE ( 'NONE', *, *, #865, .T. ) ;
#21599 = CARTESIAN_POINT ( 'NONE',  ( -10.47352321885900928, -13.96536482376412458, 61.02894424119286754 ) ) ;
#21600 = CARTESIAN_POINT ( 'NONE',  ( -10.85887813628090015, -11.28619579020030628, 64.26226673522833721 ) ) ;
#21601 = DIRECTION ( 'NONE',  ( -1.389773828427094234E-07, -3.718553705696926905E-07, 0.9999999999999211742 ) ) ;
#21602 = ORIENTED_EDGE ( 'NONE', *, *, #47467, .F. ) ;
#21603 = CARTESIAN_POINT ( 'NONE',  ( -23.80338573481879294, -11.80731802715296297, 59.76763678108634537 ) ) ;
#21604 = AXIS2_PLACEMENT_3D ( 'NONE', #14641, #28735, #37308 ) ;
#21605 = CARTESIAN_POINT ( 'NONE',  ( -24.77839546667076931, -16.00024531626065283, 66.18512132471579434 ) ) ;
#21606 = ADVANCED_FACE ( 'NONE', ( #48636 ), #30907, .T. ) ;
#21607 = EDGE_LOOP ( 'NONE', ( #17589, #42787 ) ) ;
#21608 = ORIENTED_EDGE ( 'NONE', *, *, #13811, .T. ) ;
#21609 = CARTESIAN_POINT ( 'NONE',  ( -14.99706723701585354, -21.85287888328288375, 65.29092001793476641 ) ) ;
#21610 = FACE_OUTER_BOUND ( 'NONE', #34742, .T. ) ;
#21611 = FACE_OUTER_BOUND ( 'NONE', #30054, .T. ) ;
#21612 = CARTESIAN_POINT ( 'NONE',  ( -21.25211362912655488, -21.20065753679924114, 65.76170813790885461 ) ) ;
#21613 = CARTESIAN_POINT ( 'NONE',  ( -22.82985190038863621, -19.93574988146554006, 72.68754644230530459 ) ) ;
#21614 = VERTEX_POINT ( 'NONE', #22298 ) ;
#21615 = VERTEX_POINT ( 'NONE', #22803 ) ;
#21616 = EDGE_CURVE ( 'NONE', #9195, #21614, #3968, .T. ) ;
#21617 = DIRECTION ( 'NONE',  ( 0.000000000000000000, 1.000000000000000000, -0.000000000000000000 ) ) ;
#21618 = ADVANCED_FACE ( 'NONE', ( #14876 ), #29938, .T. ) ;
#21619 = CARTESIAN_POINT ( 'NONE',  ( -19.95259202802825271, -8.281694549620906898, 73.72096610892648982 ) ) ;
#21620 = CYLINDRICAL_SURFACE ( 'NONE', #39380, 0.1499999999999994948 ) ;
#21621 = DIRECTION ( 'NONE',  ( 0.000000000000000000, 0.9999954153791273948, 0.003028072113820366902 ) ) ;
#21622 =( BOUNDED_SURFACE ( )  B_SPLINE_SURFACE ( 3, 1, ( 
 ( #13150, #23941 ),
 ( #46349, #4486 ),
 ( #38945, #16526 ),
 ( #31561, #9404 ),
 ( #28104, #31804 ),
 ( #46596, #16765 ),
 ( #1767, #27379 ) ),
 .UNSPECIFIED., .T., .F., .F. ) 
 B_SPLINE_SURFACE_WITH_KNOTS ( ( 4, 3, 4 ),
 ( 2, 2 ),
 ( 0.000000000000000000, 0.5000000000000000000, 1.000000000000000000 ),
 ( 0.000000000000000000, 1.000000000000000000 ),
 .UNSPECIFIED. ) 
 GEOMETRIC_REPRESENTATION_ITEM ( )  RATIONAL_B_SPLINE_SURFACE ( (
 ( 1.000000000000000000, 1.000000000000000000),
 ( 0.3333333333333335369, 0.3333333333333330373),
 ( 0.3333333333333335369, 0.3333333333333330373),
 ( 1.000000000000000000, 1.000000000000000000),
 ( 0.3333333333333333703, 0.3333333333333333703),
 ( 0.3333333333333333703, 0.3333333333333333703),
 ( 1.000000000000000000, 1.000000000000000000) ) ) 
 REPRESENTATION_ITEM ( '' )  SURFACE ( )  );
#21623 = CARTESIAN_POINT ( 'NONE',  ( -18.55266926790839221, -7.445060760019332591, 73.96251610088971518 ) ) ;
#21624 = ADVANCED_FACE ( 'NONE', ( #18847 ), #44720, .T. ) ;
#21625 = VERTEX_POINT ( 'NONE', #153 ) ;
#21626 = CARTESIAN_POINT ( 'NONE',  ( -18.08034385650551812, -6.424090610841176385, 49.80797279389977916 ) ) ;
#21627 = ORIENTED_EDGE ( 'NONE', *, *, #2315, .F. ) ;
#21628 = CARTESIAN_POINT ( 'NONE',  ( -24.35164181862008803, -15.81450316290537650, 69.53307533821916309 ) ) ;
#21629 = CARTESIAN_POINT ( 'NONE',  ( -23.98651520682892624, -11.28222280472095029, 66.56068001652479893 ) ) ;
#21630 = DIRECTION ( 'NONE',  ( 1.000000000000000000, -0.000000000000000000, -0.000000000000000000 ) ) ;
#21631 = ORIENTED_EDGE ( 'NONE', *, *, #6646, .F. ) ;
#21632 = VECTOR ( 'NONE', #30714, 1000.000000000000114 ) ;
#21633 = CARTESIAN_POINT ( 'NONE',  ( -10.57458500277835434, -16.25348641136583083, 71.44750329828485746 ) ) ;
#21634 = CARTESIAN_POINT ( 'NONE',  ( -10.76785811675247118, -12.48515291162924434, 57.61385273545094066 ) ) ;
#21635 = AXIS2_PLACEMENT_3D ( 'NONE', #34736, #27347, #39152 ) ;
#21636 = DIRECTION ( 'NONE',  ( -3.071710424422018668E-17, 6.404604876783312462E-16, 1.000000000000000000 ) ) ;
#21637 = CARTESIAN_POINT ( 'NONE',  ( -20.92788686586858660, -8.687255892883298358, 60.14125422863671844 ) ) ;
#21638 = ORIENTED_EDGE ( 'NONE', *, *, #13411, .F. ) ;
#21639 = PLANE ( 'NONE',  #13374 ) ;
#21640 = ORIENTED_EDGE ( 'NONE', *, *, #26514, .F. ) ;
#21641 = DIRECTION ( 'NONE',  ( 1.000000000000000000, 2.866981220435666553E-17, 0.000000000000000000 ) ) ;
#21642 = CARTESIAN_POINT ( 'NONE',  ( -17.61324970268224277, -7.361601100360097405, 63.75068226507995917 ) ) ;
#21643 = ORIENTED_EDGE ( 'NONE', *, *, #10028, .F. ) ;
#21644 = LINE ( 'NONE', #45285, #7768 ) ;
#21645 = CARTESIAN_POINT ( 'NONE',  ( -12.50776718604994109, -20.40684089597385764, 71.92158360616595303 ) ) ;
#21646 = ORIENTED_EDGE ( 'NONE', *, *, #9883, .T. ) ;
#21647 = CARTESIAN_POINT ( 'NONE',  ( -21.36489517220793743, -8.963474395264050543, 73.75128753236120360 ) ) ;
#21648 = EDGE_CURVE ( 'NONE', #24654, #5607, #15369, .T. ) ;
#21649 = CARTESIAN_POINT ( 'NONE',  ( -19.93475561761363934, -21.40553454266635569, 65.62053285436006433 ) ) ;
#21650 = CARTESIAN_POINT ( 'NONE',  ( -23.96159466281891071, -11.23502865522796768, 70.07866094266108803 ) ) ;
#21651 = ORIENTED_EDGE ( 'NONE', *, *, #33744, .T. ) ;
#21652 = LINE ( 'NONE', #33431, #44391 ) ;
#21653 = PLANE ( 'NONE',  #32217 ) ;
#21654 = FACE_OUTER_BOUND ( 'NONE', #18988, .T. ) ;
#21655 = VERTEX_POINT ( 'NONE', #10975 ) ;
#21656 = VERTEX_POINT ( 'NONE', #30191 ) ;
#21657 = CARTESIAN_POINT ( 'NONE',  ( -22.92161870814259217, -14.39064228688693170, 53.88362224778187226 ) ) ;
#21658 = CARTESIAN_POINT ( 'NONE',  ( -23.00442008925061899, -19.11762375203660724, 59.18410642057862248 ) ) ;
#21659 = ORIENTED_EDGE ( 'NONE', *, *, #37931, .T. ) ;
#21660 = CARTESIAN_POINT ( 'NONE',  ( -26.42409385541305511, -15.80920654474410725, 48.99999999999997868 ) ) ;
#21661 = CARTESIAN_POINT ( 'NONE',  ( -14.73659385759798823, -8.995762431863214559, 51.38120296130585274 ) ) ;
#21662 = CARTESIAN_POINT ( 'NONE',  ( -22.96375064570672819, -10.44813988596692411, 63.08658113699938497 ) ) ;
#21663 =( BOUNDED_CURVE ( )  B_SPLINE_CURVE ( 3, ( #45686, #45918, #4538, #26958 ),
 .UNSPECIFIED., .F., .F. ) 
 B_SPLINE_CURVE_WITH_KNOTS ( ( 4, 4 ),
 ( 0.9074455897393651771, 1.000000000000000000 ),
 .UNSPECIFIED. ) 
 CURVE ( )  GEOMETRIC_REPRESENTATION_ITEM ( )  RATIONAL_B_SPLINE_CURVE ( ( 0.6983129098260874024, 0.7760317562606933173, 0.8765941196519975165, 1.000000000000000000 ) ) 
 REPRESENTATION_ITEM ( '' )  );
#21664 = CARTESIAN_POINT ( 'NONE',  ( -13.99679447977218061, -20.97040113148658591, 71.94079819673058296 ) ) ;
#21665 = B_SPLINE_CURVE_WITH_KNOTS ( 'NONE', 3,
 ( #4764, #7746, #41706, #345, #19532, #11914, #11659, #41448, #33810, #26439 ),
 .UNSPECIFIED., .F., .F.,
 ( 4, 2, 2, 2, 4 ),
 ( 0.1272669073657870520, 0.2522669073463000844, 0.3772669073268131168, 0.5022669073073261492, 0.6272669072878391816 ),
 .UNSPECIFIED. ) ;
#21666 = CARTESIAN_POINT ( 'NONE',  ( -23.69549191163005020, -18.83074896771919526, 69.40033652239984008 ) ) ;
#21667 = CARTESIAN_POINT ( 'NONE',  ( -14.74956223559871482, -8.338905777109427930, 64.01808618867474365 ) ) ;
#21668 = VECTOR ( 'NONE', #38750, 1000.000000000000114 ) ;
#21669 = VERTEX_POINT ( 'NONE', #26235 ) ;
#21670 = CARTESIAN_POINT ( 'NONE',  ( -10.57110082969170683, -13.38215148069720861, 74.67817647591368768 ) ) ;
#21671 = FACE_OUTER_BOUND ( 'NONE', #40184, .T. ) ;
#21672 = ADVANCED_FACE ( 'NONE', ( #25999 ), #47859, .T. ) ;
#21673 = DIRECTION ( 'NONE',  ( -0.03181436478788691319, -0.9994937949748079475, -6.982004198809111150E-09 ) ) ;
#21674 = DIRECTION ( 'NONE',  ( 0.8967515337576290602, -0.4425343904188011046, 9.546469656967254525E-09 ) ) ;
#21675 = ADVANCED_FACE ( 'NONE', ( #46419 ), #870, .F. ) ;
#21676 =( BOUNDED_SURFACE ( )  B_SPLINE_SURFACE ( 3, 1, ( 
 ( #14890, #37550 ),
 ( #10989, #7057 ),
 ( #22555, #25514 ),
 ( #48403, #41509 ),
 ( #18355, #33360 ),
 ( #21820, #47929 ),
 ( #18860, #29953 ) ),
 .UNSPECIFIED., .T., .F., .F. ) 
 B_SPLINE_SURFACE_WITH_KNOTS ( ( 4, 3, 4 ),
 ( 2, 2 ),
 ( 0.000000000000000000, 0.5000000000000000000, 1.000000000000000000 ),
 ( 0.000000000000000000, 1.000000000000000000 ),
 .UNSPECIFIED. ) 
 GEOMETRIC_REPRESENTATION_ITEM ( )  RATIONAL_B_SPLINE_SURFACE ( (
 ( 1.000000000000000000, 1.000000000000000000),
 ( 0.3333333333333335369, 0.3333333333333330373),
 ( 0.3333333333333335369, 0.3333333333333330373),
 ( 1.000000000000000000, 1.000000000000000000),
 ( 0.3333333333333333703, 0.3333333333333333703),
 ( 0.3333333333333333703, 0.3333333333333333703),
 ( 1.000000000000000000, 1.000000000000000000) ) ) 
 REPRESENTATION_ITEM ( '' )  SURFACE ( )  );
#21677 = ORIENTED_EDGE ( 'NONE', *, *, #23518, .T. ) ;
#21678 = EDGE_CURVE ( 'NONE', #43576, #35243, #30408, .T. ) ;
#21679 = EDGE_LOOP ( 'NONE', ( #21748, #23972, #45062, #45384, #8785 ) ) ;
#21680 = DIRECTION ( 'NONE',  ( -1.389773828427094234E-07, -3.718553705696926905E-07, 0.9999999999999211742 ) ) ;
#21681 = CARTESIAN_POINT ( 'NONE',  ( -23.34754611528896362, -19.32773447048098348, 59.06127517204052424 ) ) ;
#21682 = DIRECTION ( 'NONE',  ( -0.9640890753730593232, 0.2655790932026005358, -6.310348464816974292E-08 ) ) ;
#21683 = ADVANCED_FACE ( 'NONE', ( #23527 ), #38527, .T. ) ;
#21684 = ORIENTED_EDGE ( 'NONE', *, *, #19300, .T. ) ;
#21685 = CARTESIAN_POINT ( 'NONE',  ( -12.64995486802317082, -19.99670083032576429, 68.33657438322859434 ) ) ;
#21686 = CARTESIAN_POINT ( 'NONE',  ( -11.22844613476422460, -11.44458948612160043, 64.43409918096024569 ) ) ;
#21687 = VERTEX_POINT ( 'NONE', #38265 ) ;
#21688 = CARTESIAN_POINT ( 'NONE',  ( -13.64505908608012064, -21.22973791158431922, 68.63437918312371266 ) ) ;
#21689 = CARTESIAN_POINT ( 'NONE',  ( -19.71455631245729379, -21.89842510487585869, 65.65824520983085222 ) ) ;
#21690 = CARTESIAN_POINT ( 'NONE',  ( -23.33670675297031849, -10.27651039223464657, 59.72390641345293716 ) ) ;
#21691 = VERTEX_POINT ( 'NONE', #13136 ) ;
#21692 = DIRECTION ( 'NONE',  ( -0.000000000000000000, -1.000000000000000000, -0.000000000000000000 ) ) ;
#21693 = AXIS2_PLACEMENT_3D ( 'NONE', #25926, #22231, #4013 ) ;
#21694 = ORIENTED_EDGE ( 'NONE', *, *, #21011, .T. ) ;
#21695 = CARTESIAN_POINT ( 'NONE',  ( -10.44881481234349252, -17.42631575494719698, 64.74243950200344955 ) ) ;
#21696 = CARTESIAN_POINT ( 'NONE',  ( -19.35593647574418341, -21.53741737806316792, 58.59795352067202145 ) ) ;
#21697 = EDGE_LOOP ( 'NONE', ( #1760, #3407, #1341, #33593, #25023 ) ) ;
#21698 = CARTESIAN_POINT ( 'NONE',  ( -24.43416774132473890, -14.02670544446237422, 69.86095212020217105 ) ) ;
#21699 = CARTESIAN_POINT ( 'NONE',  ( -23.41616298382994898, -18.52428493080399008, 72.77840375779385340 ) ) ;
#21700 = ADVANCED_FACE ( 'NONE', ( #15871 ), #24015, .T. ) ;
#21701 = CARTESIAN_POINT ( 'NONE',  ( -10.80042129562301589, -17.07348610811987299, 57.87863715479691251 ) ) ;
#21702 = CARTESIAN_POINT ( 'NONE',  ( -13.83659385759798965, -8.995762431863214559, 51.38120296130585274 ) ) ;
#21703 = CARTESIAN_POINT ( 'NONE',  ( -24.16575310113231367, -12.74704012323608104, 70.07243002239954421 ) ) ;
#21704 = VERTEX_POINT ( 'NONE', #4556 ) ;
#21705 = CARTESIAN_POINT ( 'NONE',  ( -10.06050713658121154, -13.29172449529390398, 53.76227901944321985 ) ) ;
#21706 = FACE_OUTER_BOUND ( 'NONE', #4732, .T. ) ;
#21707 = CARTESIAN_POINT ( 'NONE',  ( -22.93618324136711450, -9.797101482063153455, 70.13365771114293068 ) ) ;
#21708 = CARTESIAN_POINT ( 'NONE',  ( -13.14412777716299274, -20.90712260751159590, 58.14675838192486879 ) ) ;
#21709 = CYLINDRICAL_SURFACE ( 'NONE', #10947, 4.686499999999997002 ) ;
#21710 = CARTESIAN_POINT ( 'NONE',  ( -13.18659385650551918, -9.302874398569244363, 51.68646062012417985 ) ) ;
#21711 = ORIENTED_EDGE ( 'NONE', *, *, #1031, .F. ) ;
#21712 = VERTEX_POINT ( 'NONE', #35559 ) ;
#21713 = CARTESIAN_POINT ( 'NONE',  ( -23.49945856589985027, -11.21686614839013885, 66.57781614479455357 ) ) ;
#21714 = CARTESIAN_POINT ( 'NONE',  ( -45.55409385541306477, -13.72754205882879042, 70.03986341317408915 ) ) ;
#21715 = ORIENTED_EDGE ( 'NONE', *, *, #40332, .T. ) ;
#21717 = CARTESIAN_POINT ( 'NONE',  ( -13.66784385650551670, -6.428312510596451368, 51.20221977374900035 ) ) ;
#21716 = CARTESIAN_POINT ( 'NONE',  ( -15.41904748403203484, -7.634001509309876532, 74.19490257054667381 ) ) ;
#21718 = FACE_OUTER_BOUND ( 'NONE', #41475, .T. ) ;
#21719 = CARTESIAN_POINT ( 'NONE',  ( -15.69021238316472022, -21.64649376854531226, 72.04575306413649116 ) ) ;
#21720 = CARTESIAN_POINT ( 'NONE',  ( -22.17046091269999764, -9.065891900838490614, 59.83515915777798710 ) ) ;
#21721 = CARTESIAN_POINT ( 'NONE',  ( -24.71344798646422802, -16.35160113208834431, 62.77984073303771595 ) ) ;
#21722 = EDGE_CURVE ( 'NONE', #39291, #48597, #4808, .T. ) ;
#21723 = CARTESIAN_POINT ( 'NONE',  ( -11.13733870171179596, -11.61806121328042174, 67.90392505421056057 ) ) ;
#21724 = CYLINDRICAL_SURFACE ( 'NONE', #418, 0.1500000000000045464 ) ;
#21725 =( BOUNDED_CURVE ( )  B_SPLINE_CURVE ( 3, ( #37361, #44130, #8097, #33664 ),
 .UNSPECIFIED., .F., .F. ) 
 B_SPLINE_CURVE_WITH_KNOTS ( ( 4, 4 ),
 ( 0.5000000000000000000, 0.9074455897393660653 ),
 .UNSPECIFIED. ) 
 CURVE ( )  GEOMETRIC_REPRESENTATION_ITEM ( )  RATIONAL_B_SPLINE_CURVE ( ( 1.000000000000010214, 0.4567392136813359649, 0.3561768502900245492, 0.6983129098260869583 ) ) 
 REPRESENTATION_ITEM ( '' )  );
#21726 = CARTESIAN_POINT ( 'NONE',  ( -11.68335768792166185, -18.81469630946190819, 68.51689631952916670 ) ) ;
#21727 = VERTEX_POINT ( 'NONE', #1838 ) ;
#21728 = CARTESIAN_POINT ( 'NONE',  ( -10.78031428196279329, -11.32923628920978310, 54.27966884056655061 ) ) ;
#21729 = CARTESIAN_POINT ( 'NONE',  ( -11.60882265867669538, -10.15221075964790742, 71.13039628648064649 ) ) ;
#21730 = EDGE_CURVE ( 'NONE', #48127, #44738, #15108, .T. ) ;
#21731 = CARTESIAN_POINT ( 'NONE',  ( -11.16720068213728467, -11.56054720508597455, 67.76864607954532005 ) ) ;
#21732 = CARTESIAN_POINT ( 'NONE',  ( -24.57849813159777597, -12.72878314728456850, 66.41591366067137869 ) ) ;
#21733 = CARTESIAN_POINT ( 'NONE',  ( -10.73412848974934874, -11.53077067998621175, 71.20365450754333381 ) ) ;
#21734 = DIRECTION ( 'NONE',  ( 0.8547111024021490921, 0.5191039697695417621, 7.472447835916433805E-08 ) ) ;
#21735 = ORIENTED_EDGE ( 'NONE', *, *, #27398, .T. ) ;
#21736 = VECTOR ( 'NONE', #11568, 1000.000000000000000 ) ;
#21737 = EDGE_LOOP ( 'NONE', ( #32882, #30417, #5672, #34936 ) ) ;
#21738 = VECTOR ( 'NONE', #12006, 999.9999999999998863 ) ;
#21739 = CARTESIAN_POINT ( 'NONE',  ( -17.23659385541304445, -8.995762431863214559, 51.38120296130585274 ) ) ;
#21740 = B_SPLINE_CURVE_WITH_KNOTS ( 'NONE', 3,
 ( #4780, #9205, #42455, #26945, #16077, #41965, #24226, #8470, #8726, #31119 ),
 .UNSPECIFIED., .F., .F.,
 ( 4, 2, 2, 2, 4 ),
 ( 0.1272669073658330707, 0.2522669073463126299, 0.3772669073267921336, 0.5022669073072716373, 0.6272669072877512519 ),
 .UNSPECIFIED. ) ;
#21741 = EDGE_CURVE ( 'NONE', #25935, #38842, #29257, .T. ) ;
#21742 = VERTEX_POINT ( 'NONE', #16354 ) ;
#21743 = CARTESIAN_POINT ( 'NONE',  ( -17.40971054907340942, -7.359207646686905413, 67.12065337040019131 ) ) ;
#21744 = FACE_OUTER_BOUND ( 'NONE', #36876, .T. ) ;
#21745 = EDGE_CURVE ( 'NONE', #45033, #10587, #31571, .T. ) ;
#21746 = CARTESIAN_POINT ( 'NONE',  ( -15.42638489646220279, -7.631913115121209401, 74.20268781468831776 ) ) ;
#21747 = CARTESIAN_POINT ( 'NONE',  ( -9.975073501874963000, -14.93475060744560245, 74.84132960708070925 ) ) ;
#21748 = ORIENTED_EDGE ( 'NONE', *, *, #29922, .T. ) ;
#21749 = CARTESIAN_POINT ( 'NONE',  ( -13.99854101903132531, -20.98015058628177698, 65.14195714266269022 ) ) ;
#21750 = CARTESIAN_POINT ( 'NONE',  ( -20.94265863490610258, -21.37680627582274795, 62.30126734817043399 ) ) ;
#21751 = ORIENTED_EDGE ( 'NONE', *, *, #12269, .F. ) ;
#21752 = LINE ( 'NONE', #39742, #44635 ) ;
#21753 = EDGE_CURVE ( 'NONE', #3004, #37170, #43929, .T. ) ;
#21754 = CARTESIAN_POINT ( 'NONE',  ( -12.73047692465080338, -11.91646811004319062, 53.88362224778186516 ) ) ;
#21755 = EDGE_CURVE ( 'NONE', #21199, #18877, #4158, .T. ) ;
#21756 = EDGE_LOOP ( 'NONE', ( #38523, #36831, #36196, #32397, #44490 ) ) ;
#21757 = CARTESIAN_POINT ( 'NONE',  ( -23.32045150837215175, -18.68837265512984303, 62.50973769122266788 ) ) ;
#21758 = DIRECTION ( 'NONE',  ( -0.9687793358424819923, 0.2479245821708680464, 0.000000000000000000 ) ) ;
#21759 = CARTESIAN_POINT ( 'NONE',  ( -23.34189317711797429, -10.28335673940103590, 59.64557479084083269 ) ) ;
#21760 = EDGE_CURVE ( 'NONE', #44791, #8067, #39797, .T. ) ;
#21761 = ORIENTED_EDGE ( 'NONE', *, *, #8638, .F. ) ;
#21762 = CARTESIAN_POINT ( 'NONE',  ( -10.73412800634210029, -11.53077167852495677, 71.20365559628196195 ) ) ;
#21763 = CARTESIAN_POINT ( 'NONE',  ( -12.05615918852498680, -19.97535170061420828, 61.51183199568394144 ) ) ;
#21764 = CARTESIAN_POINT ( 'NONE',  ( -24.32852063849251323, -13.38246526728995001, 59.37740068604990995 ) ) ;
#21765 = DIRECTION ( 'NONE',  ( -1.000000000000000000, 0.000000000000000000, 0.000000000000000000 ) ) ;
#21766 = ORIENTED_EDGE ( 'NONE', *, *, #31095, .F. ) ;
#21767 = CYLINDRICAL_SURFACE ( 'NONE', #43182, 5.249999999999998224 ) ;
#21768 = CARTESIAN_POINT ( 'NONE',  ( -15.34011657121100924, -21.49348207936204247, 72.23502552990838410 ) ) ;
#21769 = AXIS2_PLACEMENT_3D ( 'NONE', #6161, #48236, #43603 ) ;
#21770 = VECTOR ( 'NONE', #26700, 1000.000000000000000 ) ;
#21771 = CARTESIAN_POINT ( 'NONE',  ( -11.73296596577226936, -10.64774513788296240, 74.72412863062541533 ) ) ;
#21772 = CARTESIAN_POINT ( 'NONE',  ( -16.98902004117856990, -21.84877635801032270, 68.58071880800348197 ) ) ;
#21773 = CARTESIAN_POINT ( 'NONE',  ( -24.30112618867181240, -13.25578303422174997, 59.64795780745660636 ) ) ;
#21774 = ORIENTED_EDGE ( 'NONE', *, *, #6369, .F. ) ;
#21775 = CARTESIAN_POINT ( 'NONE',  ( -10.67361454459859260, -12.95690279139224188, 64.45939287679182428 ) ) ;
#21776 = CARTESIAN_POINT ( 'NONE',  ( -15.52409385759799143, -9.359200813967568422, 50.49621490985803263 ) ) ;
#21777 = LINE ( 'NONE', #36763, #7042 ) ;
#21778 = EDGE_LOOP ( 'NONE', ( #46017, #45874, #44421, #26448, #3722 ) ) ;
#21779 = CARTESIAN_POINT ( 'NONE',  ( -17.85534385541293645, -8.623186033802644701, 49.24843789510448033 ) ) ;
#21780 = ORIENTED_EDGE ( 'NONE', *, *, #29388, .F. ) ;
#21781 = EDGE_LOOP ( 'NONE', ( #45819, #13160 ) ) ;
#21782 = ORIENTED_EDGE ( 'NONE', *, *, #43370, .T. ) ;
#21783 = FACE_OUTER_BOUND ( 'NONE', #3396, .T. ) ;
#21784 = CARTESIAN_POINT ( 'NONE',  ( -40.92409385541305511, -14.80920654474410725, 74.99999999999998579 ) ) ;
#21785 = CARTESIAN_POINT ( 'NONE',  ( -12.68532353738824803, -9.060482037740600347, 71.03420644255490402 ) ) ;
#21786 = EDGE_LOOP ( 'NONE', ( #443, #3101, #24872, #23932, #36380 ) ) ;
#21787 = ORIENTED_EDGE ( 'NONE', *, *, #26409, .F. ) ;
#21788 = CARTESIAN_POINT ( 'NONE',  ( -17.21159385650551599, -6.922745924619793101, 51.69366785382590024 ) ) ;
#21789 = ADVANCED_FACE ( 'NONE', ( #8498 ), #11336, .T. ) ;
#21790 = CARTESIAN_POINT ( 'NONE',  ( 22.62590614458706639, 3.140741878271520626, 50.53406581128081143 ) ) ;
#21791 = CARTESIAN_POINT ( 'NONE',  ( -23.44879792247470007, -11.14072156699261207, 69.89210571255328830 ) ) ;
#21792 =( BOUNDED_SURFACE ( )  B_SPLINE_SURFACE ( 3, 1, ( 
 ( #23755, #23256 ),
 ( #46639, #27910 ),
 ( #12166, #9208 ),
 ( #1810, #24231 ),
 ( #16081, #27185 ),
 ( #39234, #35537 ),
 ( #31121, #13112 ) ),
 .UNSPECIFIED., .T., .F., .F. ) 
 B_SPLINE_SURFACE_WITH_KNOTS ( ( 4, 3, 4 ),
 ( 2, 2 ),
 ( 0.000000000000000000, 0.5000000000000000000, 1.000000000000000000 ),
 ( 0.000000000000000000, 1.000000000000000000 ),
 .UNSPECIFIED. ) 
 GEOMETRIC_REPRESENTATION_ITEM ( )  RATIONAL_B_SPLINE_SURFACE ( (
 ( 1.000000000000000000, 1.000000000000000000),
 ( 0.3333333333333335369, 0.3333333333333330373),
 ( 0.3333333333333335369, 0.3333333333333330373),
 ( 1.000000000000000000, 1.000000000000000000),
 ( 0.3333333333333333703, 0.3333333333333333703),
 ( 0.3333333333333333703, 0.3333333333333333703),
 ( 1.000000000000000000, 1.000000000000000000) ) ) 
 REPRESENTATION_ITEM ( '' )  SURFACE ( )  );
#21793 = CARTESIAN_POINT ( 'NONE',  ( -17.66159385650551528, -9.295667164867525756, 49.30633214617472504 ) ) ;
#21794 = AXIS2_PLACEMENT_3D ( 'NONE', #11743, #41286, #41535 ) ;
#21795 = AXIS2_PLACEMENT_3D ( 'NONE', #15004, #30554, #22416 ) ;
#21796 = VERTEX_POINT ( 'NONE', #6508 ) ;
#21797 = CARTESIAN_POINT ( 'NONE',  ( -24.37451731887211892, -15.64135521309706967, 69.75980740431705840 ) ) ;
#21798 = CARTESIAN_POINT ( 'NONE',  ( -24.45288365649568618, -15.45035942066159862, 69.68874360283344060 ) ) ;
#21799 = AXIS2_PLACEMENT_3D ( 'NONE', #14564, #22742, #4026 ) ;
#21800 = CARTESIAN_POINT ( 'NONE',  ( -21.32695110138281791, -8.937895085234787373, 73.89568928637402223 ) ) ;
#21801 = ORIENTED_EDGE ( 'NONE', *, *, #42705, .T. ) ;
#21802 =( BOUNDED_CURVE ( )  B_SPLINE_CURVE ( 3, ( #15033, #44157, #30095, #40909 ),
 .UNSPECIFIED., .F., .F. ) 
 B_SPLINE_CURVE_WITH_KNOTS ( ( 4, 4 ),
 ( 0.000000000000000000, 0.4074455897393631787 ),
 .UNSPECIFIED. ) 
 CURVE ( )  GEOMETRIC_REPRESENTATION_ITEM ( )  RATIONAL_B_SPLINE_CURVE ( ( 1.000000000000000000, 0.4567392136813362979, 0.3561768502900319322, 0.6983129098260868473 ) ) 
 REPRESENTATION_ITEM ( '' )  );
#21803 = DIRECTION ( 'NONE',  ( 1.896855589267346620E-06, 2.136244919385519396E-06, 0.9999999999959191532 ) ) ;
#21804 =( BOUNDED_CURVE ( )  B_SPLINE_CURVE ( 3, ( #47261, #32704, #17193, #31993 ),
 .UNSPECIFIED., .F., .F. ) 
 B_SPLINE_CURVE_WITH_KNOTS ( ( 4, 4 ),
 ( 0.9074455897393587378, 1.000000000000000000 ),
 .UNSPECIFIED. ) 
 CURVE ( )  GEOMETRIC_REPRESENTATION_ITEM ( )  RATIONAL_B_SPLINE_CURVE ( ( 0.6983129098260755230, 0.7760317562606831032, 0.8765941196519912992, 1.000000000000000000 ) ) 
 REPRESENTATION_ITEM ( '' )  );
#21805 = EDGE_CURVE ( 'NONE', #73, #19297, #2072, .T. ) ;
#21806 = ORIENTED_EDGE ( 'NONE', *, *, #38120, .F. ) ;
#21807 = CARTESIAN_POINT ( 'NONE',  ( -24.72409385541305582, -14.90920654474414775, 61.92352941176469727 ) ) ;
#21808 = CARTESIAN_POINT ( 'NONE',  ( -10.11684863658992839, -16.26127201416540302, 71.62563171993747346 ) ) ;
#21809 = EDGE_CURVE ( 'NONE', #39260, #8618, #9286, .T. ) ;
#21811 = EDGE_CURVE ( 'NONE', #112, #39233, #39746, .T. ) ;
#21810 = CARTESIAN_POINT ( 'NONE',  ( -45.92409385541306932, -16.70920654474410938, 70.50000000000000000 ) ) ;
#21812 = CARTESIAN_POINT ( 'NONE',  ( -21.52668677937081299, -21.02802818395438322, 72.66413103959850162 ) ) ;
#21813 = ORIENTED_EDGE ( 'NONE', *, *, #8380, .T. ) ;
#21814 = CARTESIAN_POINT ( 'NONE',  ( -22.82568502052561499, -19.94010355682323166, 72.83674718307834439 ) ) ;
#21815 = DIRECTION ( 'NONE',  ( 5.517078692044801135E-07, 1.257343604232908019E-06, 0.9999999999990574207 ) ) ;
#21816 = CARTESIAN_POINT ( 'NONE',  ( -21.52726120556258849, -9.076273861542912158, 70.28132538914752558 ) ) ;
#21817 = VERTEX_POINT ( 'NONE', #47143 ) ;
#21818 = CARTESIAN_POINT ( 'NONE',  ( -20.71231197388234690, -20.98888764657868578, 58.65977609787367442 ) ) ;
#21819 = CARTESIAN_POINT ( 'NONE',  ( -8.424093855413071097, -6.859206544744110623, 52.99999999999997868 ) ) ;
#21821 =( BOUNDED_CURVE ( )  B_SPLINE_CURVE ( 3, ( #47504, #29022, #10074, #24854 ),
 .UNSPECIFIED., .F., .F. ) 
 B_SPLINE_CURVE_WITH_KNOTS ( ( 4, 4 ),
 ( 0.000000000000000000, 0.4074455897393606252 ),
 .UNSPECIFIED. ) 
 CURVE ( )  GEOMETRIC_REPRESENTATION_ITEM ( )  RATIONAL_B_SPLINE_CURVE ( ( 1.000000000000000000, 0.4567392136813354653, 0.3561768502900315991, 0.6983129098260884016 ) ) 
 REPRESENTATION_ITEM ( '' )  );
#21820 = CARTESIAN_POINT ( 'NONE',  ( -18.92901792560347829, -7.918630368440815026, 70.78556921992733919 ) ) ;
#21822 = VERTEX_POINT ( 'NONE', #48102 ) ;
#21823 = CARTESIAN_POINT ( 'NONE',  ( -11.72322480355222396, -10.74717599656355027, 74.62988016596645480 ) ) ;
#21824 = B_SPLINE_CURVE_WITH_KNOTS ( 'NONE', 3,
 ( #10636, #25644, #40658, #19732, #45607, #34240, #5196, #4229, #8896, #45352 ),
 .UNSPECIFIED., .F., .F.,
 ( 4, 2, 2, 2, 4 ),
 ( 0.1272669073657614613, 0.2522669073462631140, 0.3772669073267648221, 0.5022669073072665302, 0.6272669072877681273 ),
 .UNSPECIFIED. ) ;
#21825 = ORIENTED_EDGE ( 'NONE', *, *, #28709, .F. ) ;
#21826 = DIRECTION ( 'NONE',  ( 1.000000000000000000, 0.000000000000000000, 0.000000000000000000 ) ) ;
#21827 = CARTESIAN_POINT ( 'NONE',  ( -13.71293330176565384, -21.26916511146244915, 68.64120417180296840 ) ) ;
#21828 = CARTESIAN_POINT ( 'NONE',  ( -21.98892968875003717, -15.92178434430670642, 52.02966884056656482 ) ) ;
#21829 = CARTESIAN_POINT ( 'NONE',  ( -22.65633676998887935, -10.15891879009521581, 70.31178531762441253 ) ) ;
#21830 = ORIENTED_EDGE ( 'NONE', *, *, #40567, .T. ) ;
#21831 = CARTESIAN_POINT ( 'NONE',  ( -10.46640864507116753, -14.03671221754458109, 60.93437953636007620 ) ) ;
#21832 = VERTEX_POINT ( 'NONE', #43208 ) ;
#21833 = CARTESIAN_POINT ( 'NONE',  ( -24.20817551436923765, -11.73026151181330512, 59.73881638530829008 ) ) ;
#21834 = DIRECTION ( 'NONE',  ( -0.9294853595766571219, -0.3688590060343552857, 0.000000000000000000 ) ) ;
#21835 = ORIENTED_EDGE ( 'NONE', *, *, #6461, .F. ) ;
#21836 = DIRECTION ( 'NONE',  ( 0.000000000000000000, 0.000000000000000000, 1.000000000000000000 ) ) ;
#21837 = AXIS2_PLACEMENT_3D ( 'NONE', #48219, #25097, #40120 ) ;
#21838 = DIRECTION ( 'NONE',  ( -0.9132646967824439299, 0.4073666574609056124, -8.344532079829881716E-09 ) ) ;
#21839 = EDGE_CURVE ( 'NONE', #11979, #16837, #38520, .T. ) ;
#21840 = ORIENTED_EDGE ( 'NONE', *, *, #16694, .T. ) ;
#21841 = ORIENTED_EDGE ( 'NONE', *, *, #35914, .T. ) ;
#21842 = CARTESIAN_POINT ( 'NONE',  ( -14.77890319739905145, -21.35274797201484276, 65.25029445929627059 ) ) ;
#21843 = LINE ( 'NONE', #18132, #20221 ) ;
#21844 = CARTESIAN_POINT ( 'NONE',  ( -10.15209110106313695, -13.18697342404853146, 74.86472985364514443 ) ) ;
#21845 = CARTESIAN_POINT ( 'NONE',  ( -10.04084212758499994, -13.81292206000487433, 57.60971574196104683 ) ) ;
#21846 = CARTESIAN_POINT ( 'NONE',  ( -14.80624607021532135, -8.317144234858641738, 60.31996281969095719 ) ) ;
#21847 = CARTESIAN_POINT ( 'NONE',  ( -24.30048588269890075, -16.36411231998813065, 59.12332431758468942 ) ) ;
#21848 = CARTESIAN_POINT ( 'NONE',  ( -20.18610667881221232, -8.319513185189903126, 66.66615430743608783 ) ) ;
#21849 = AXIS2_PLACEMENT_3D ( 'NONE', #46020, #45302, #26826 ) ;
#21850 = ORIENTED_EDGE ( 'NONE', *, *, #41450, .T. ) ;
#21851 = EDGE_LOOP ( 'NONE', ( #42098, #7054, #29263, #30196, #39580 ) ) ;
#21852 = CARTESIAN_POINT ( 'NONE',  ( -13.38575581802539993, -9.030060914960570173, 60.72478133471773276 ) ) ;
#21853 = CARTESIAN_POINT ( 'NONE',  ( -13.40763370604777371, -17.22402126197653160, 49.52966884056655772 ) ) ;
#21854 = CARTESIAN_POINT ( 'NONE',  ( -21.07302329935935958, -21.30456606900342464, 62.29188282781374397 ) ) ;
#21855 = CARTESIAN_POINT ( 'NONE',  ( -24.03160971261424805, -17.26750559640275640, 69.71339792588547368 ) ) ;
#21856 = LINE ( 'NONE', #23091, #18152 ) ;
#21857 = VERTEX_POINT ( 'NONE', #6743 ) ;
#21858 = CARTESIAN_POINT ( 'NONE',  ( -20.49909385650551741, -8.114302828567740988, 52.18300498402516041 ) ) ;
#21859 = ORIENTED_EDGE ( 'NONE', *, *, #8908, .T. ) ;
#21860 = LINE ( 'NONE', #36860, #24102 ) ;
#21861 = CARTESIAN_POINT ( 'NONE',  ( -13.92409385541305511, -10.60920654474410618, 78.99999999999998579 ) ) ;
#21862 = DIRECTION ( 'NONE',  ( 0.9687793358424821033, -0.2479245821708677133, 0.000000000000000000 ) ) ;
#21863 = CIRCLE ( 'NONE', #7720, 5.249999999999998224 ) ;
#21864 = CARTESIAN_POINT ( 'NONE',  ( -10.39906353449755372, -15.43672942677450521, 61.45277822496478848 ) ) ;
#21865 = AXIS2_PLACEMENT_3D ( 'NONE', #14841, #17820, #21547 ) ;
#21866 = EDGE_LOOP ( 'NONE', ( #4097, #2551, #43077, #19942, #34391 ) ) ;
#21867 = CARTESIAN_POINT ( 'NONE',  ( -14.73482268938652417, -8.346338953448071862, 60.33498763304578461 ) ) ;
#21868 = EDGE_CURVE ( 'NONE', #35725, #37402, #25218, .T. ) ;
#21869 = ORIENTED_EDGE ( 'NONE', *, *, #13811, .F. ) ;
#21870 = CARTESIAN_POINT ( 'NONE',  ( -15.57524973202195184, -7.592253851314364255, 70.80978608612899450 ) ) ;
#21871 = DIRECTION ( 'NONE',  ( 0.2122660683108583690, -0.9772119095896469876, 7.504255179194988334E-08 ) ) ;
#21872 = ORIENTED_EDGE ( 'NONE', *, *, #15125, .F. ) ;
#21873 = DIRECTION ( 'NONE',  ( 3.413470714839332458E-33, -1.190614954331866791E-16, 1.000000000000000000 ) ) ;
#21874 = ORIENTED_EDGE ( 'NONE', *, *, #25705, .T. ) ;
#21875 = DIRECTION ( 'NONE',  ( -3.071710424422018668E-17, 6.404604876783312462E-16, 1.000000000000000000 ) ) ;
#21876 = ADVANCED_FACE ( 'NONE', ( #9723 ), #39992, .T. ) ;
#21877 = EDGE_CURVE ( 'NONE', #27679, #40722, #9483, .T. ) ;
#21878 = CARTESIAN_POINT ( 'NONE',  ( -24.87323499971020624, -14.68548341078430575, 62.85263093027649006 ) ) ;
#21879 = ORIENTED_EDGE ( 'NONE', *, *, #32110, .T. ) ;
#21880 = CARTESIAN_POINT ( 'NONE',  ( -22.41240261796999178, -19.79131148728009393, 69.46858230278321855 ) ) ;
#21881 = EDGE_CURVE ( 'NONE', #21727, #10431, #33087, .T. ) ;
#21882 = CARTESIAN_POINT ( 'NONE',  ( -11.47236213698566054, -10.32806074475630886, 74.55389686390628867 ) ) ;
#21883 = ORIENTED_EDGE ( 'NONE', *, *, #43703, .T. ) ;
#21884 = CARTESIAN_POINT ( 'NONE',  ( -17.42409385541305511, -14.80920654474410725, 45.99899999999998101 ) ) ;
#21885 = ADVANCED_FACE ( 'NONE', ( #47390 ), #36035, .T. ) ;
#21886 = B_SPLINE_CURVE_WITH_KNOTS ( 'NONE', 3,
 ( #3994, #16017, #26642, #23686, #26388, #41403, #19004, #34009, #306, #41657 ),
 .UNSPECIFIED., .F., .F.,
 ( 4, 2, 2, 2, 4 ),
 ( 0.6272669072877865570, 0.7522669073073026125, 0.8772669073268186679, 1.002266907346334612, 1.127266907365850779 ),
 .UNSPECIFIED. ) ;
#21887 = DIRECTION ( 'NONE',  ( 0.000000000000000000, 0.000000000000000000, 1.000000000000000000 ) ) ;
#21888 = CARTESIAN_POINT ( 'NONE',  ( -24.86170408668008847, -14.37683769452534222, 66.32146239653503983 ) ) ;
#21889 = ORIENTED_EDGE ( 'NONE', *, *, #2845, .T. ) ;
#21890 = CARTESIAN_POINT ( 'NONE',  ( -11.73296596577226936, -10.64774513788296417, 74.72412863062541533 ) ) ;
#21891 = EDGE_CURVE ( 'NONE', #45956, #15007, #48608, .T. ) ;
#21892 = ORIENTED_EDGE ( 'NONE', *, *, #39882, .F. ) ;
#21893 = ORIENTED_EDGE ( 'NONE', *, *, #9769, .T. ) ;
#21894 = FACE_OUTER_BOUND ( 'NONE', #21198, .T. ) ;
#21895 = CARTESIAN_POINT ( 'NONE',  ( -17.39742520082695165, -7.759256980592265762, 67.17039592192074338 ) ) ;
#21897 = CARTESIAN_POINT ( 'NONE',  ( -10.44916039635137039, -15.83526825291551177, 64.50771589744864798 ) ) ;
#21896 = AXIS2_PLACEMENT_3D ( 'NONE', #22255, #10932, #6752 ) ;
#21898 =( BOUNDED_SURFACE ( )  B_SPLINE_SURFACE ( 3, 1, ( 
 ( #11422, #40263 ),
 ( #36531, #32844 ),
 ( #47883, #3054 ),
 ( #18066, #33076 ),
 ( #14355, #29412 ),
 ( #19541, #11925 ),
 ( #4291, #38741 ) ),
 .UNSPECIFIED., .T., .F., .F. ) 
 B_SPLINE_SURFACE_WITH_KNOTS ( ( 4, 3, 4 ),
 ( 2, 2 ),
 ( 0.000000000000000000, 0.5000000000000000000, 1.000000000000000000 ),
 ( 0.000000000000000000, 1.000000000000000000 ),
 .UNSPECIFIED. ) 
 GEOMETRIC_REPRESENTATION_ITEM ( )  RATIONAL_B_SPLINE_SURFACE ( (
 ( 1.000000000000000000, 1.000000000000000000),
 ( 0.3333333333333335369, 0.3333333333333330373),
 ( 0.3333333333333335369, 0.3333333333333330373),
 ( 1.000000000000000000, 1.000000000000000000),
 ( 0.3333333333333333703, 0.3333333333333333703),
 ( 0.3333333333333333703, 0.3333333333333333703),
 ( 1.000000000000000000, 1.000000000000000000) ) ) 
 REPRESENTATION_ITEM ( '' )  SURFACE ( )  );
#21899 = CARTESIAN_POINT ( 'NONE',  ( -14.39909385759799143, -8.105421454601382081, 49.25000573077640098 ) ) ;
#21900 = CARTESIAN_POINT ( 'NONE',  ( -8.039996143071578061, -9.893874759132541996, 53.49999999999995026 ) ) ;
#21901 = MECHANICAL_DESIGN_GEOMETRIC_PRESENTATION_REPRESENTATION (  '', ( #41558 ), #48644 ) ;
#21902 = CARTESIAN_POINT ( 'NONE',  ( -15.48396703021662546, -7.615489166865526904, 70.72334449499163611 ) ) ;
#21903 = AXIS2_PLACEMENT_3D ( 'NONE', #8720, #38740, #8234 ) ;
#21904 = CIRCLE ( 'NONE', #13239, 5.249999999999998224 ) ;
#21905 = DIRECTION ( 'NONE',  ( 1.616182858256118783E-16, 0.003028072113822189229, -0.9999954153791275058 ) ) ;
#21906 = VERTEX_POINT ( 'NONE', #13856 ) ;
#21907 = CARTESIAN_POINT ( 'NONE',  ( -11.16720021946830244, -11.56054808309503557, 67.91864607954204303 ) ) ;
#21908 =( LENGTH_UNIT ( ) NAMED_UNIT ( * ) SI_UNIT ( .MILLI., .METRE. ) );
#21909 = VECTOR ( 'NONE', #41760, 999.9999999999998863 ) ;
#21910 = CARTESIAN_POINT ( 'NONE',  ( -24.72409385541305582, -14.90920654474416729, 63.03529411764704804 ) ) ;
#21911 = CARTESIAN_POINT ( 'NONE',  ( -17.72419722990865054, -21.80277058550420577, 58.40553378253839156 ) ) ;
#21912 = ORIENTED_EDGE ( 'NONE', *, *, #30299, .T. ) ;
#21913 = VERTEX_POINT ( 'NONE', #40242 ) ;
#21914 = LINE ( 'NONE', #36916, #10722 ) ;
#21915 = B_SPLINE_CURVE_WITH_KNOTS ( 'NONE', 1,
 ( #33695, #22160 ),
 .UNSPECIFIED., .F., .F.,
 ( 2, 2 ),
 ( 0.000000000000000000, 1.000000000000000000 ),
 .UNSPECIFIED. ) ;
#21916 = CYLINDRICAL_SURFACE ( 'NONE', #1670, 0.1500000000000071554 ) ;
#21917 = PLANE ( 'NONE',  #4436 ) ;
#21918 = EDGE_CURVE ( 'NONE', #14949, #9880, #38051, .T. ) ;
#21919 = VERTEX_POINT ( 'NONE', #43949 ) ;
#21920 = DIRECTION ( 'NONE',  ( 0.9687793358424821033, -0.2479245821708680464, 0.000000000000000000 ) ) ;
#21921 = DIRECTION ( 'NONE',  ( -1.000000000000000000, -0.000000000000000000, -0.000000000000000000 ) ) ;
#21922 = ADVANCED_FACE ( 'NONE', ( #28432 ), #18082, .F. ) ;
#21923 = ORIENTED_EDGE ( 'NONE', *, *, #1140, .T. ) ;
#21924 = CARTESIAN_POINT ( 'NONE',  ( -13.67308226471031141, -21.24601619275060571, 68.65636342939112069 ) ) ;
#21925 = CIRCLE ( 'NONE', #9364, 4.686499999999997890 ) ;
#21926 = CARTESIAN_POINT ( 'NONE',  ( -12.56747607676768830, -20.45877693976744638, 71.98370581712723038 ) ) ;
#21927 = CARTESIAN_POINT ( 'NONE',  ( -10.83447764080151643, -17.17455424171161482, 64.85569185657212188 ) ) ;
#21928 = ORIENTED_EDGE ( 'NONE', *, *, #10709, .T. ) ;
#21929 = CARTESIAN_POINT ( 'NONE',  ( -24.84449963183508459, -13.71944596863515464, 47.99999999999994316 ) ) ;
#21930 = AXIS2_PLACEMENT_3D ( 'NONE', #16812, #1564, #15846 ) ;
#21931 = AXIS2_PLACEMENT_3D ( 'NONE', #1063, #16061, #31102 ) ;
#21932 = ORIENTED_EDGE ( 'NONE', *, *, #5408, .T. ) ;
#21933 = DIRECTION ( 'NONE',  ( 0.8356905716187448263, -0.5492005722024783099, -7.728900804118361606E-08 ) ) ;
#21934 = CARTESIAN_POINT ( 'NONE',  ( -24.39025819466740685, -14.12117216163392186, 69.72563349076150985 ) ) ;
#21935 = ORIENTED_EDGE ( 'NONE', *, *, #18257, .F. ) ;
#21936 = CARTESIAN_POINT ( 'NONE',  ( -17.42409385541299471, -14.80920654474435594, 52.02966884056656482 ) ) ;
#21937 = DIRECTION ( 'NONE',  ( 1.000000000000000000, -4.164305804376849172E-17, 1.614929280266638808E-16 ) ) ;
#21938 = EDGE_CURVE ( 'NONE', #17399, #10862, #30784, .T. ) ;
#21939 = CARTESIAN_POINT ( 'NONE',  ( -22.49909385650551741, -8.114302828567740988, 52.18300498402516041 ) ) ;
#21940 = DIRECTION ( 'NONE',  ( 0.000000000000000000, 0.000000000000000000, -1.000000000000000000 ) ) ;
#21941 = CIRCLE ( 'NONE', #21187, 1.999999999999999778 ) ;
#21942 = EDGE_CURVE ( 'NONE', #21919, #12981, #41544, .T. ) ;
#21943 =( BOUNDED_SURFACE ( )  B_SPLINE_SURFACE ( 3, 1, ( 
 ( #24944, #39963 ),
 ( #6231, #2045 ),
 ( #47110, #6479 ),
 ( #40208, #17771 ),
 ( #17295, #6711 ),
 ( #36253, #43917 ),
 ( #36484, #46868 ) ),
 .UNSPECIFIED., .T., .F., .F. ) 
 B_SPLINE_SURFACE_WITH_KNOTS ( ( 4, 3, 4 ),
 ( 2, 2 ),
 ( 0.000000000000000000, 0.5000000000000000000, 1.000000000000000000 ),
 ( 0.000000000000000000, 1.000000000000000000 ),
 .UNSPECIFIED. ) 
 GEOMETRIC_REPRESENTATION_ITEM ( )  RATIONAL_B_SPLINE_SURFACE ( (
 ( 1.000000000000000000, 1.000000000000000000),
 ( 0.3333333333333335369, 0.3333333333333330373),
 ( 0.3333333333333335369, 0.3333333333333330373),
 ( 1.000000000000000000, 1.000000000000000000),
 ( 0.3333333333333333703, 0.3333333333333333703),
 ( 0.3333333333333333703, 0.3333333333333333703),
 ( 1.000000000000000000, 1.000000000000000000) ) ) 
 REPRESENTATION_ITEM ( '' )  SURFACE ( )  );
#21944 = CARTESIAN_POINT ( 'NONE',  ( -24.23636321612255173, -17.82529083293033167, 62.58865660992282898 ) ) ;
#21945 = CARTESIAN_POINT ( 'NONE',  ( -22.86460234468921016, -19.29871796126476013, 59.18410835798781022 ) ) ;
#21946 = CARTESIAN_POINT ( 'NONE',  ( -24.23267513707162379, -12.96582210470760543, 70.07243177896738473 ) ) ;
#21947 = ORIENTED_EDGE ( 'NONE', *, *, #38791, .T. ) ;
#21948 = CARTESIAN_POINT ( 'NONE',  ( -9.939267784769082681, -14.33236412611010913, 54.27966884056655061 ) ) ;
#21949 = FACE_OUTER_BOUND ( 'NONE', #16305, .T. ) ;
#21950 = DIRECTION ( 'NONE',  ( -1.000000000000000000, 4.164305804376849172E-17, -1.614929280266638808E-16 ) ) ;
#21951 = CARTESIAN_POINT ( 'NONE',  ( -10.44916060947156566, -15.83526976542894182, 64.65771589744088033 ) ) ;
#21952 = ADVANCED_FACE ( 'NONE', ( #17565 ), #46587, .T. ) ;
#21953 = CARTESIAN_POINT ( 'NONE',  ( -16.23263389423368963, -22.16407464444966280, 58.39930168947970657 ) ) ;
#21954 = DIRECTION ( 'NONE',  ( -3.071710424422018668E-17, 6.404604876783312462E-16, 1.000000000000000000 ) ) ;
#21955 = VERTEX_POINT ( 'NONE', #26189 ) ;
#21956 = ORIENTED_EDGE ( 'NONE', *, *, #30513, .F. ) ;
#21957 = CARTESIAN_POINT ( 'NONE',  ( -11.39216336840796373, -18.45920852072106300, 61.29182966166492719 ) ) ;
#21958 = ORIENTED_EDGE ( 'NONE', *, *, #45028, .F. ) ;
#21960 = CARTESIAN_POINT ( 'NONE',  ( -13.89284385650552167, -7.406986770994973490, 48.81910596585309747 ) ) ;
#21959 = DIRECTION ( 'NONE',  ( -0.2479245821708678799, -0.9687793358424819923, -2.626836608253746575E-18 ) ) ;
#21961 = CARTESIAN_POINT ( 'NONE',  ( -11.30083338927175873, -18.20384847608787027, 57.87884914278906479 ) ) ;
#21962 = CARTESIAN_POINT ( 'NONE',  ( -11.57425704488359841, -18.65360627554439077, 65.04707076833931012 ) ) ;
#21963 = CARTESIAN_POINT ( 'NONE',  ( -14.47717485532954029, -21.65240259781455023, 58.35273132940589136 ) ) ;
#21964 = EDGE_CURVE ( 'NONE', #12705, #6741, #33293, .T. ) ;
#21965 = B_SPLINE_CURVE_WITH_KNOTS ( 'NONE', 3,
 ( #6763, #43717, #25472, #20813, #17094, #9971, #40481, #32617, #6525, #2811 ),
 .UNSPECIFIED., .F., .F.,
 ( 4, 2, 2, 2, 4 ),
 ( 0.6272669072782678379, 0.7522669073001559958, 0.8772669073220440428, 1.002266907343932090, 1.127266907365820359 ),
 .UNSPECIFIED. ) ;
#21966 = FACE_BOUND ( 'NONE', #28281, .T. ) ;
#21967 = FACE_OUTER_BOUND ( 'NONE', #43637, .T. ) ;
#21968 =( BOUNDED_CURVE ( )  B_SPLINE_CURVE ( 3, ( #34880, #923, #38824, #30492 ),
 .UNSPECIFIED., .F., .F. ) 
 B_SPLINE_CURVE_WITH_KNOTS ( ( 4, 4 ),
 ( 0.9074455897393660653, 1.000000000000000000 ),
 .UNSPECIFIED. ) 
 CURVE ( )  GEOMETRIC_REPRESENTATION_ITEM ( )  RATIONAL_B_SPLINE_CURVE ( ( 0.6983129098260907330, 0.7760317562606962039, 0.8765941196519992928, 1.000000000000000000 ) ) 
 REPRESENTATION_ITEM ( '' )  );
#21969 = CARTESIAN_POINT ( 'NONE',  ( -23.41616298382994898, -18.52428493080399008, 72.77840375779385340 ) ) ;
#21970 = CARTESIAN_POINT ( 'NONE',  ( -16.74954815124876006, -21.77674055613599080, 68.99560679921106043 ) ) ;
#21971 = ORIENTED_EDGE ( 'NONE', *, *, #46580, .F. ) ;
#21972 = FACE_OUTER_BOUND ( 'NONE', #10842, .T. ) ;
#21973 = CARTESIAN_POINT ( 'NONE',  ( -38.65852941833841783, -27.10920654474410796, 78.99999999999998579 ) ) ;
#21974 = VECTOR ( 'NONE', #33194, 1000.000000000000000 ) ;
#21975 = CARTESIAN_POINT ( 'NONE',  ( -16.84878425383806189, -22.23771130781744532, 72.35198525528087998 ) ) ;
#21976 = CARTESIAN_POINT ( 'NONE',  ( -11.06177494515391757, -11.76359664285707574, 67.61864456584771688 ) ) ;
#21977 = CARTESIAN_POINT ( 'NONE',  ( -24.21572389103915413, -12.90431785807809639, 62.83263897504365048 ) ) ;
#21978 = CARTESIAN_POINT ( 'NONE',  ( -14.06084784944548716, -21.00867483325099982, 68.34136283933983691 ) ) ;
#21979 = CARTESIAN_POINT ( 'NONE',  ( -20.92409385541305511, -10.60920654474410618, 78.99999999999998579 ) ) ;
#21980 = CIRCLE ( 'NONE', #36892, 5.249999999999998224 ) ;
#21981 = AXIS2_PLACEMENT_3D ( 'NONE', #45001, #13989, #48663 ) ;
#21982 = ORIENTED_EDGE ( 'NONE', *, *, #17838, .T. ) ;
#21983 = ORIENTED_EDGE ( 'NONE', *, *, #8079, .T. ) ;
#21984 = CARTESIAN_POINT ( 'NONE',  ( -14.98659385541304268, -7.222650657624104298, 49.61879703869476543 ) ) ;
#21985 = ORIENTED_EDGE ( 'NONE', *, *, #46915, .F. ) ;
#21986 = CARTESIAN_POINT ( 'NONE',  ( -17.13206997002025389, -21.80311261865791295, 72.27429256327307883 ) ) ;
#21987 = B_SPLINE_CURVE_WITH_KNOTS ( 'NONE', 1,
 ( #10971, #26966 ),
 .UNSPECIFIED., .F., .F.,
 ( 2, 2 ),
 ( 0.000000000000000000, 1.000000000000000000 ),
 .UNSPECIFIED. ) ;
#21988 = CARTESIAN_POINT ( 'NONE',  ( 18.62590614458706995, 1.876518846661452411, 52.53023010607846288 ) ) ;
#21989 = AXIS2_PLACEMENT_3D ( 'NONE', #9439, #9914, #36473 ) ;
#21990 = ADVANCED_FACE ( 'NONE', ( #33795 ), #18788, .T. ) ;
#21991 = CARTESIAN_POINT ( 'NONE',  ( -17.42409385541299471, -14.80920654474435594, 52.02966884056656482 ) ) ;
#21992 = DIRECTION ( 'NONE',  ( 0.6380325334150263039, -0.7700094066334535192, 0.000000000000000000 ) ) ;
#21993 = VECTOR ( 'NONE', #22144, 1000.000000000000114 ) ;
#21994 = ORIENTED_EDGE ( 'NONE', *, *, #39390, .T. ) ;
#21995 = DIRECTION ( 'NONE',  ( -0.6105870317843966610, -0.7919491628991827126, 6.540688078712155195E-08 ) ) ;
#21996 = CARTESIAN_POINT ( 'NONE',  ( -46.47622156840087371, -14.20920654474410760, 70.13000000000000966 ) ) ;
#21997 = ORIENTED_EDGE ( 'NONE', *, *, #5265, .T. ) ;
#21998 = CARTESIAN_POINT ( 'NONE',  ( -21.49815937814055999, -9.116931945208399668, 70.43132539264750847 ) ) ;
#21999 = DIRECTION ( 'NONE',  ( 2.866981220435666553E-17, -1.000000000000000000, -1.190614954331866791E-16 ) ) ;
#22000 = ORIENTED_EDGE ( 'NONE', *, *, #47856, .F. ) ;
#22001 = CARTESIAN_POINT ( 'NONE',  ( -10.55090139406780558, -17.68373120125836806, 68.14076041135473361 ) ) ;
#22002 = DIRECTION ( 'NONE',  ( 0.9687793358424821033, -0.2479245821708679631, 1.885439946533205044E-16 ) ) ;
#22003 = CARTESIAN_POINT ( 'NONE',  ( -23.00454255336054743, -10.50046069577333263, 59.88731295783226471 ) ) ;
#22004 = VERTEX_POINT ( 'NONE', #34042 ) ;
#22005 = CARTESIAN_POINT ( 'NONE',  ( -11.22470860480879118, -11.43539691024457206, 71.23293728648457090 ) ) ;
#22006 = EDGE_CURVE ( 'NONE', #5056, #18999, #36802, .T. ) ;
#22007 = CARTESIAN_POINT ( 'NONE',  ( -23.36642234765754367, -18.50986368505970958, 72.77984929533243985 ) ) ;
#22008 = VECTOR ( 'NONE', #44914, 1000.000000000000000 ) ;
#22009 = EDGE_CURVE ( 'NONE', #33660, #44249, #46270, .T. ) ;
#22010 = CARTESIAN_POINT ( 'NONE',  ( -10.76763519559319882, -17.13171766695033327, 61.15743118826002700 ) ) ;
#22011 = CARTESIAN_POINT ( 'NONE',  ( -21.99213670719075253, -20.17946569659695655, 59.04970794435396897 ) ) ;
#22012 = ORIENTED_EDGE ( 'NONE', *, *, #44965, .T. ) ;
#22013 = DIRECTION ( 'NONE',  ( 1.616182858256118536E-16, 0.003028072113822188795, -0.9999954153791273948 ) ) ;
#22014 = CARTESIAN_POINT ( 'NONE',  ( -15.48424252676649182, -21.53505049348036948, 72.34575460973682937 ) ) ;
#22015 = CARTESIAN_POINT ( 'NONE',  ( -21.92674792687542862, -8.873837487361237564, 66.81149990064047017 ) ) ;
#22016 = ADVANCED_FACE ( 'NONE', ( #14568 ), #19275, .T. ) ;
#22017 = CARTESIAN_POINT ( 'NONE',  ( -22.58034385650552167, -6.424090610841176385, 49.80797279389978627 ) ) ;
#22018 = ORIENTED_EDGE ( 'NONE', *, *, #12128, .F. ) ;
#22019 = CARTESIAN_POINT ( 'NONE',  ( -24.66730423131801331, -13.06573828131289616, 62.94768895321241331 ) ) ;
#22020 = CARTESIAN_POINT ( 'NONE',  ( -20.98034385759799036, -9.360768649639304329, 51.01397948905922419 ) ) ;
#22021 = EDGE_LOOP ( 'NONE', ( #26279, #15496, #33617, #34657, #10283 ) ) ;
#22022 = CARTESIAN_POINT ( 'NONE',  ( -17.91839958824308709, -21.79173199888728263, 61.87535923606637311 ) ) ;
#22023 = AXIS2_PLACEMENT_3D ( 'NONE', #33683, #48732, #45064 ) ;
#22024 = ADVANCED_FACE ( 'NONE', ( #22487, #37485 ), #29629, .F. ) ;
#22025 = CARTESIAN_POINT ( 'NONE',  ( -24.43362360091611052, -14.05489060867666673, 73.42271507725003232 ) ) ;
#22026 = CARTESIAN_POINT ( 'NONE',  ( -11.70231104532641631, -10.03806069876099727, 67.69885649244250203 ) ) ;
#22027 = EDGE_LOOP ( 'NONE', ( #36407, #8677, #8195, #12654, #69 ) ) ;
#22028 = LINE ( 'NONE', #21314, #41211 ) ;
#22029 = ORIENTED_EDGE ( 'NONE', *, *, #14781, .T. ) ;
#22030 = VERTEX_POINT ( 'NONE', #3777 ) ;
#22031 = ORIENTED_EDGE ( 'NONE', *, *, #48438, .T. ) ;
#22032 = CIRCLE ( 'NONE', #30695, 1.999999999999999556 ) ;
#22033 = CARTESIAN_POINT ( 'NONE',  ( -13.97409385650551528, -9.792211528768506312, 50.49490371617623197 ) ) ;
#22034 = CARTESIAN_POINT ( 'NONE',  ( -50.42609385541305755, -14.90920654474412643, 59.91176470588234793 ) ) ;
#22035 = CARTESIAN_POINT ( 'NONE',  ( -17.42409385541300182, -14.80920654474440745, 52.02966884056655061 ) ) ;
#22036 = CARTESIAN_POINT ( 'NONE',  ( -14.05958695725781915, -8.162196217632502027, 70.82934004658783067 ) ) ;
#22037 = ADVANCED_FACE ( 'NONE', ( #41434 ), #44662, .F. ) ;
#22038 = CARTESIAN_POINT ( 'NONE',  ( -13.18494979104506015, -8.682762004662409439, 60.48304321394137162 ) ) ;
#22039 = B_SPLINE_CURVE_WITH_KNOTS ( 'NONE', 3,
 ( #44779, #21628, #3387, #44292, #14203, #18397, #33402, #14433, #3634, #48443 ),
 .UNSPECIFIED., .F., .F.,
 ( 4, 2, 2, 2, 4 ),
 ( 0.000000000000000000, 0.2500000000000000000, 0.5000000000000000000, 0.7500000000000000000, 1.000000000000000000 ),
 .UNSPECIFIED. ) ;
#22040 = EDGE_CURVE ( 'NONE', #39442, #32446, #37236, .T. ) ;
#22041 = ORIENTED_EDGE ( 'NONE', *, *, #10495, .T. ) ;
#22042 = ORIENTED_EDGE ( 'NONE', *, *, #12402, .T. ) ;
#22043 = CARTESIAN_POINT ( 'NONE',  ( -14.11784385650551954, -9.790100578890868377, 49.79778022625163203 ) ) ;
#22044 = EDGE_CURVE ( 'NONE', #7471, #21408, #33537, .T. ) ;
#22045 = CARTESIAN_POINT ( 'NONE',  ( -11.47653751526730304, -10.32245935128858427, 74.61697868304008807 ) ) ;
#22046 = CYLINDRICAL_SURFACE ( 'NONE', #8007, 0.1500000000000003553 ) ;
#22047 = AXIS2_PLACEMENT_3D ( 'NONE', #9897, #39924, #47563 ) ;
#22048 = CARTESIAN_POINT ( 'NONE',  ( -18.84284385650551386, -8.811426318492348031, 52.18089403414751359 ) ) ;
#22049 = PRODUCT_DEFINITION_SHAPE ( 'NONE', 'NONE',  #48737 ) ;
#22050 = ORIENTED_EDGE ( 'NONE', *, *, #32515, .F. ) ;
#22051 = CARTESIAN_POINT ( 'NONE',  ( -16.71957921250844592, -21.82421608262117729, 68.71032757591046902 ) ) ;
#22052 = DIRECTION ( 'NONE',  ( -3.071710424422018668E-17, 6.404604876783312462E-16, 1.000000000000000000 ) ) ;
#22053 = VECTOR ( 'NONE', #43246, 1000.000000000000000 ) ;
#22054 = ORIENTED_EDGE ( 'NONE', *, *, #1561, .T. ) ;
#22055 = DIRECTION ( 'NONE',  ( 0.9687793358424821033, -0.2479245821708677133, 0.000000000000000000 ) ) ;
#22056 = EDGE_LOOP ( 'NONE', ( #29186, #9143 ) ) ;
#22057 = CARTESIAN_POINT ( 'NONE',  ( -13.07136565370527315, -8.762923774744256988, 64.02451247989536398 ) ) ;
#22058 = CARTESIAN_POINT ( 'NONE',  ( -20.28184570768963013, -8.419050735858720103, 66.79606545271752793 ) ) ;
#22059 = CARTESIAN_POINT ( 'NONE',  ( -18.56294508348570460, -7.902357773425570997, 73.84064450189322315 ) ) ;
#22060 = CARTESIAN_POINT ( 'NONE',  ( -10.39641337496300544, -12.33600653425179416, 57.48890720123886666 ) ) ;
#22061 = ORIENTED_EDGE ( 'NONE', *, *, #33653, .T. ) ;
#22062 = CARTESIAN_POINT ( 'NONE',  ( -11.09546941031917378, -10.87811254196722111, 57.34756656758956694 ) ) ;
#22063 = CARTESIAN_POINT ( 'NONE',  ( -24.42531086868747892, -14.77968181448406426, 62.78466667327232642 ) ) ;
#22064 = B_SPLINE_CURVE_WITH_KNOTS ( 'NONE', 1,
 ( #21699, #47086 ),
 .UNSPECIFIED., .F., .F.,
 ( 2, 2 ),
 ( 0.000000000000000000, 1.000000000000000000 ),
 .UNSPECIFIED. ) ;
#22065 = CARTESIAN_POINT ( 'NONE',  ( -42.79688797306012304, -14.90920654474413709, 60.01764705882352047 ) ) ;
#22066 = CARTESIAN_POINT ( 'NONE',  ( -19.28352822169459202, -22.07505156356299381, 47.99999999999994316 ) ) ;
#22067 = ORIENTED_EDGE ( 'NONE', *, *, #18454, .F. ) ;
#22068 = CARTESIAN_POINT ( 'NONE',  ( -16.26183769579148475, -7.855670737815882099, 60.50028478907628937 ) ) ;
#22069 = CARTESIAN_POINT ( 'NONE',  ( -17.21153000696512336, -19.50285887057015088, 52.02966884056656482 ) ) ;
#22070 = DIRECTION ( 'NONE',  ( -0.003782665018460030538, -0.9999928456970870183, -9.532993539451315208E-09 ) ) ;
#22071 = VERTEX_POINT ( 'NONE', #19037 ) ;
#22072 = FACE_BOUND ( 'NONE', #47254, .T. ) ;
#22074 = ORIENTED_EDGE ( 'NONE', *, *, #2957, .T. ) ;
#22073 = EDGE_CURVE ( 'NONE', #36314, #8953, #13376, .T. ) ;
#22075 = DIRECTION ( 'NONE',  ( 2.866981220435666553E-17, -1.000000000000000000, -1.190614954331866791E-16 ) ) ;
#22076 = DIRECTION ( 'NONE',  ( 0.000000000000000000, 0.007114381193220190198, -0.9999746924698832418 ) ) ;
#22077 = ADVANCED_FACE ( 'NONE', ( #38714 ), #9185, .T. ) ;
#22078 = VECTOR ( 'NONE', #47744, 1000.000000000000000 ) ;
#22079 = DIRECTION ( 'NONE',  ( -0.000000000000000000, -1.000000000000000000, -0.000000000000000000 ) ) ;
#22080 = ORIENTED_EDGE ( 'NONE', *, *, #31742, .F. ) ;
#22081 = LINE ( 'NONE', #48413, #32359 ) ;
#22082 = ORIENTED_EDGE ( 'NONE', *, *, #20662, .F. ) ;
#22083 = CARTESIAN_POINT ( 'NONE',  ( -21.57946453887431204, -8.565578233975859490, 54.27966884056655061 ) ) ;
#22084 = PLANE ( 'NONE',  #5466 ) ;
#22085 = VERTEX_POINT ( 'NONE', #27392 ) ;
#22086 = CARTESIAN_POINT ( 'NONE',  ( -9.979603264230430426, -14.52052340097724148, 68.04295441848455539 ) ) ;
#22087 = AXIS2_PLACEMENT_3D ( 'NONE', #20612, #35605, #1389 ) ;
#22088 = CARTESIAN_POINT ( 'NONE',  ( -18.39951368268757648, -22.19516171751901368, 69.00010101991060196 ) ) ;
#22089 = ORIENTED_EDGE ( 'NONE', *, *, #7, .F. ) ;
#22090 = ORIENTED_EDGE ( 'NONE', *, *, #19161, .F. ) ;
#22091 = CYLINDRICAL_SURFACE ( 'NONE', #10773, 0.1500000000000054345 ) ;
#22092 = DIRECTION ( 'NONE',  ( 1.590464103011092396E-07, -3.579926632912963412E-07, 0.9999999999999231726 ) ) ;
#22093 = AXIS2_PLACEMENT_3D ( 'NONE', #29987, #37341, #47960 ) ;
#22094 = CARTESIAN_POINT ( 'NONE',  ( -23.45365590349393869, -19.18493892615664365, 62.45383243984888111 ) ) ;
#22095 = CARTESIAN_POINT ( 'NONE',  ( -10.02995815481606634, -13.89786978184575794, 57.63320425522585566 ) ) ;
#22096 =( BOUNDED_CURVE ( )  B_SPLINE_CURVE ( 3, ( #28761, #29484, #2654, #44284 ),
 .UNSPECIFIED., .F., .F. ) 
 B_SPLINE_CURVE_WITH_KNOTS ( ( 4, 4 ),
 ( 0.000000000000000000, 0.4074455897393662318 ),
 .UNSPECIFIED. ) 
 CURVE ( )  GEOMETRIC_REPRESENTATION_ITEM ( )  RATIONAL_B_SPLINE_CURVE ( ( 1.000000000000000000, 0.4567392136813306358, 0.3561768502900297673, 0.6983129098260973944 ) ) 
 REPRESENTATION_ITEM ( '' )  );
#22097 = CARTESIAN_POINT ( 'NONE',  ( -11.67943375510494874, -18.89645239624664796, 68.50217487844219022 ) ) ;
#22098 = CARTESIAN_POINT ( 'NONE',  ( -13.95122194917832914, -8.664767797030865637, 70.88524802578001527 ) ) ;
#22099 = CARTESIAN_POINT ( 'NONE',  ( -22.87929373774275632, -19.88409160966729772, 72.75745300618787326 ) ) ;
#22100 = EDGE_CURVE ( 'NONE', #18877, #22777, #40954, .T. ) ;
#22101 = ORIENTED_EDGE ( 'NONE', *, *, #34512, .F. ) ;
#22102 = ORIENTED_EDGE ( 'NONE', *, *, #12679, .F. ) ;
#22103 = DIRECTION ( 'NONE',  ( -0.3636930986378154040, -0.9315188296557533887, 1.850371887917986020E-09 ) ) ;
#22104 = EDGE_CURVE ( 'NONE', #6106, #20133, #28030, .T. ) ;
#22105 = ADVANCED_FACE ( 'NONE', ( #42671 ), #19775, .T. ) ;
#22106 = EDGE_CURVE ( 'NONE', #45116, #33352, #1052, .T. ) ;
#22107 =( GEOMETRIC_REPRESENTATION_CONTEXT ( 3 ) GLOBAL_UNCERTAINTY_ASSIGNED_CONTEXT ( ( #13460 ) ) GLOBAL_UNIT_ASSIGNED_CONTEXT ( ( #5412, #33349, #47260 ) ) REPRESENTATION_CONTEXT ( 'NONE', 'WORKASPACE' ) );
#22108 = CARTESIAN_POINT ( 'NONE',  ( -24.72409385541305582, -14.80920654474413745, 60.91764705882351905 ) ) ;
#22109 = DIRECTION ( 'NONE',  ( -1.487365705136564946E-06, 6.376425429333053644E-07, 0.9999999999986904919 ) ) ;
#22110 = CARTESIAN_POINT ( 'NONE',  ( -46.47622156840087371, -14.20920654474410760, 70.13000000000000966 ) ) ;
#22111 = LINE ( 'NONE', #22592, #200 ) ;
#22112 = EDGE_LOOP ( 'NONE', ( #39386, #22661, #22889, #21510, #14628 ) ) ;
#22113 =( BOUNDED_SURFACE ( )  B_SPLINE_SURFACE ( 3, 1, ( 
 ( #3785, #11407 ),
 ( #33065, #44670 ),
 ( #10929, #40966 ),
 ( #29894, #44925 ),
 ( #31337, #12376 ),
 ( #20017, #26682 ),
 ( #340, #27400 ) ),
 .UNSPECIFIED., .T., .F., .F. ) 
 B_SPLINE_SURFACE_WITH_KNOTS ( ( 4, 3, 4 ),
 ( 2, 2 ),
 ( 0.000000000000000000, 0.5000000000000000000, 1.000000000000000000 ),
 ( 0.000000000000000000, 1.000000000000000000 ),
 .UNSPECIFIED. ) 
 GEOMETRIC_REPRESENTATION_ITEM ( )  RATIONAL_B_SPLINE_SURFACE ( (
 ( 1.000000000000000000, 1.000000000000000000),
 ( 0.3333333333333335369, 0.3333333333333330373),
 ( 0.3333333333333335369, 0.3333333333333330373),
 ( 1.000000000000000000, 1.000000000000000000),
 ( 0.3333333333333333703, 0.3333333333333333703),
 ( 0.3333333333333333703, 0.3333333333333333703),
 ( 1.000000000000000000, 1.000000000000000000) ) ) 
 REPRESENTATION_ITEM ( '' )  SURFACE ( )  );
#22114 = CARTESIAN_POINT ( 'NONE',  ( -18.69909385650551670, -8.114302828567740988, 52.18300498402516041 ) ) ;
#22115 =( BOUNDED_CURVE ( )  B_SPLINE_CURVE ( 3, ( #41600, #19188, #4910, #46751 ),
 .UNSPECIFIED., .F., .F. ) 
 B_SPLINE_CURVE_WITH_KNOTS ( ( 4, 4 ),
 ( 0.9074455897393582937, 1.000000000000000000 ),
 .UNSPECIFIED. ) 
 CURVE ( )  GEOMETRIC_REPRESENTATION_ITEM ( )  RATIONAL_B_SPLINE_CURVE ( ( 0.6983129098260780765, 0.7760317562606853237, 0.8765941196519926315, 1.000000000000000000 ) ) 
 REPRESENTATION_ITEM ( '' )  );
#22116 = ORIENTED_EDGE ( 'NONE', *, *, #27519, .F. ) ;
#22117 = PRESENTATION_LAYER_ASSIGNMENT (  '', '', ( #4064 ) ) ;
#22118 = CARTESIAN_POINT ( 'NONE',  ( -16.91478550490786859, -21.84108428878278119, 72.18015306840750611 ) ) ;
#22119 = CARTESIAN_POINT ( 'NONE',  ( -12.00910550946480093, -19.92697606054074910, 58.04027092519303466 ) ) ;
#22120 = CIRCLE ( 'NONE', #23715, 5.249999999999998224 ) ;
#22121 = CARTESIAN_POINT ( 'NONE',  ( -10.52422430310768320, -17.61911375464911700, 68.21226508126260057 ) ) ;
#22122 = VERTEX_POINT ( 'NONE', #12850 ) ;
#22123 = AXIS2_PLACEMENT_3D ( 'NONE', #40758, #14148, #25026 ) ;
#22124 =( BOUNDED_CURVE ( )  B_SPLINE_CURVE ( 3, ( #44131, #29082, #6195, #2501 ),
 .UNSPECIFIED., .F., .F. ) 
 B_SPLINE_CURVE_WITH_KNOTS ( ( 4, 4 ),
 ( 0.4074455897393659543, 0.5000000000000000000 ),
 .UNSPECIFIED. ) 
 CURVE ( )  GEOMETRIC_REPRESENTATION_ITEM ( )  RATIONAL_B_SPLINE_CURVE ( ( 0.6983129098260879575, 0.7760317562606924291, 0.8765941196519958512, 0.9999999999999976685 ) ) 
 REPRESENTATION_ITEM ( '' )  );
#22125 = CARTESIAN_POINT ( 'NONE',  ( -15.47038646904106507, -21.58309222549749506, 72.34575460768671462 ) ) ;
#22126 = DIRECTION ( 'NONE',  ( -0.9840843158728899143, 0.1445225939548007710, 0.1033986416233888955 ) ) ;
#22127 = ADVANCED_FACE ( 'NONE', ( #38956 ), #5231, .F. ) ;
#22128 = ORIENTED_EDGE ( 'NONE', *, *, #10177, .T. ) ;
#22129 = VECTOR ( 'NONE', #33781, 1000.000000000000000 ) ;
#22130 = CARTESIAN_POINT ( 'NONE',  ( -18.72680718162379065, -7.880610904852765053, 70.67068030199192208 ) ) ;
#22131 = CARTESIAN_POINT ( 'NONE',  ( -10.43972881942000086, -15.77115500203794873, 64.52243715390834211 ) ) ;
#22132 = ORIENTED_EDGE ( 'NONE', *, *, #23533, .F. ) ;
#22133 = CARTESIAN_POINT ( 'NONE',  ( -21.99178500617274779, -9.439039195359631762, 59.72171213140594404 ) ) ;
#22134 = ORIENTED_EDGE ( 'NONE', *, *, #34280, .F. ) ;
#22135 = CARTESIAN_POINT ( 'NONE',  ( -15.35953700001868683, -21.96742592204022770, 72.19575459128920158 ) ) ;
#22136 = CARTESIAN_POINT ( 'NONE',  ( -11.53125565324743107, -18.58817318659712114, 65.03090579962859863 ) ) ;
#22137 = ORIENTED_EDGE ( 'NONE', *, *, #23870, .T. ) ;
#22138 = CARTESIAN_POINT ( 'NONE',  ( -13.17078218117215549, -9.186392337449538203, 67.39414915108072535 ) ) ;
#22139 = AXIS2_PLACEMENT_3D ( 'NONE', #41258, #33356, #48161 ) ;
#22140 = CARTESIAN_POINT ( 'NONE',  ( -18.62018691191416764, -22.16273284384092079, 72.42364395285933654 ) ) ;
#22141 = EDGE_CURVE ( 'NONE', #39613, #22485, #46880, .T. ) ;
#22142 = ORIENTED_EDGE ( 'NONE', *, *, #33234, .F. ) ;
#22143 = CARTESIAN_POINT ( 'NONE',  ( -12.00971705810820467, -9.691755786776280246, 60.67422651510300113 ) ) ;
#22144 = DIRECTION ( 'NONE',  ( -0.1240347345892086062, 1.145860353393066553E-16, -0.9922778767136676281 ) ) ;
#22145 = CARTESIAN_POINT ( 'NONE',  ( -21.61813339613238227, -8.651787399021619862, 73.71633365192373333 ) ) ;
#22146 = ORIENTED_EDGE ( 'NONE', *, *, #24826, .F. ) ;
#22147 = CARTESIAN_POINT ( 'NONE',  ( -12.53474317923432224, -20.43030517998690954, 71.95653676292567980 ) ) ;
#22148 = CARTESIAN_POINT ( 'NONE',  ( -11.33335366867738259, -11.35902659219953748, 60.90559029689631387 ) ) ;
#22149 = FACE_OUTER_BOUND ( 'NONE', #20180, .T. ) ;
#22150 = ORIENTED_EDGE ( 'NONE', *, *, #4784, .T. ) ;
#22151 = ORIENTED_EDGE ( 'NONE', *, *, #14607, .F. ) ;
#22152 = CIRCLE ( 'NONE', #924, 3.250000000000002220 ) ;
#22153 = CARTESIAN_POINT ( 'NONE',  ( -22.79960313759534074, -9.650943445293346912, 73.66656413195866548 ) ) ;
#22154 = CARTESIAN_POINT ( 'NONE',  ( -18.05440415122280839, -21.83127237841607027, 65.36004252941745563 ) ) ;
#22155 = DIRECTION ( 'NONE',  ( -3.071710424422018668E-17, 6.404604876783312462E-16, 1.000000000000000000 ) ) ;
#22156 = CARTESIAN_POINT ( 'NONE',  ( -14.34284385759799108, -7.587656875400194068, 49.25157356644813689 ) ) ;
#22157 = LINE ( 'NONE', #44819, #8520 ) ;
#22158 = CARTESIAN_POINT ( 'NONE',  ( -12.84691039585993444, -8.931012183600500975, 67.56438067310742213 ) ) ;
#22159 = CARTESIAN_POINT ( 'NONE',  ( -19.17247849636888901, -7.567181371456696226, 63.61584626116109575 ) ) ;
#22160 = CARTESIAN_POINT ( 'NONE',  ( -23.42409385541304090, -9.359200813967568422, 50.49621490985803263 ) ) ;
#22161 = ORIENTED_EDGE ( 'NONE', *, *, #1768, .T. ) ;
#22162 = CARTESIAN_POINT ( 'NONE',  ( -24.45201639769885205, -14.25170802724723451, 69.80275273439818307 ) ) ;
#22163 = EDGE_CURVE ( 'NONE', #35531, #11465, #37184, .T. ) ;
#22164 = EDGE_CURVE ( 'NONE', #18995, #42817, #25671, .T. ) ;
#22165 = AXIS2_PLACEMENT_3D ( 'NONE', #12417, #21023, #1323 ) ;
#22166 = DIRECTION ( 'NONE',  ( -3.071710424422018668E-17, 6.404604876783312462E-16, 1.000000000000000000 ) ) ;
#22167 = DIRECTION ( 'NONE',  ( 3.071710424422018668E-17, -6.404604876783312462E-16, -1.000000000000000000 ) ) ;
#22168 = ORIENTED_EDGE ( 'NONE', *, *, #26234, .F. ) ;
#22169 = EDGE_CURVE ( 'NONE', #46048, #30823, #32058, .T. ) ;
#22170 = EDGE_CURVE ( 'NONE', #28666, #32577, #42263, .T. ) ;
#22171 = ORIENTED_EDGE ( 'NONE', *, *, #26217, .F. ) ;
#22172 = CARTESIAN_POINT ( 'NONE',  ( -20.70232472158584969, -8.624289250480600799, 59.84125250310036392 ) ) ;
#22173 = CYLINDRICAL_SURFACE ( 'NONE', #25272, 0.1500000000000020484 ) ;
#22174 = CARTESIAN_POINT ( 'NONE',  ( -13.35819042472069107, -21.05197888995676436, 61.70141705377209007 ) ) ;
#22175 = CARTESIAN_POINT ( 'NONE',  ( -11.55573855159262386, -10.21941529800896653, 71.15388400389697665 ) ) ;
#22176 = EDGE_LOOP ( 'NONE', ( #1155, #24076 ) ) ;
#22177 = DIRECTION ( 'NONE',  ( -0.9660698163281070672, -0.2582810677919976095, 5.363434502754640132E-08 ) ) ;
#22178 = CARTESIAN_POINT ( 'NONE',  ( -11.42264205816738176, -11.09470156419723708, 64.29315101522172426 ) ) ;
#22179 = EDGE_CURVE ( 'NONE', #10355, #15076, #25560, .T. ) ;
#22180 = EDGE_LOOP ( 'NONE', ( #21994, #6002 ) ) ;
#22181 = CARTESIAN_POINT ( 'NONE',  ( -22.27803375191225399, -20.46189896727856095, 62.42094464928214848 ) ) ;
#22182 = CARTESIAN_POINT ( 'NONE',  ( -38.65852941833841783, -27.10920654474410796, 76.99999999999998579 ) ) ;
#22183 = LINE ( 'NONE', #26121, #588 ) ;
#22184 = EDGE_LOOP ( 'NONE', ( #7153, #31699, #6311, #18857, #15205 ) ) ;
#22185 = DIRECTION ( 'NONE',  ( 0.000000000000000000, 1.000000000000000000, -0.000000000000000000 ) ) ;
#22186 = ORIENTED_EDGE ( 'NONE', *, *, #36273, .T. ) ;
#22187 = CARTESIAN_POINT ( 'NONE',  ( -10.45186911607087943, -17.43433898691305473, 64.82077674941292855 ) ) ;
#22188 = CARTESIAN_POINT ( 'NONE',  ( -19.94733193681641481, -19.41309290135173526, 49.52966884056656482 ) ) ;
#22189 = VERTEX_POINT ( 'NONE', #9666 ) ;
#22190 = CARTESIAN_POINT ( 'NONE',  ( -23.71751471349159601, -11.63122711669449494, 63.23746208799618529 ) ) ;
#22191 = CARTESIAN_POINT ( 'NONE',  ( -50.42609385541305755, -14.80920654474412679, 59.01176470588234224 ) ) ;
#22192 = CARTESIAN_POINT ( 'NONE',  ( -21.43034385650551599, -9.794322478646142471, 51.19202720610083190 ) ) ;
#22193 = FACE_OUTER_BOUND ( 'NONE', #48454, .T. ) ;
#22194 = CARTESIAN_POINT ( 'NONE',  ( -24.48201381491371009, -14.78211897600973934, 66.32725479646262556 ) ) ;
#22195 = CARTESIAN_POINT ( 'NONE',  ( -12.89447938415233175, -16.05746464591689104, 49.52966884056655772 ) ) ;
#22196 = CYLINDRICAL_SURFACE ( 'NONE', #42368, 0.1499999999999988287 ) ;
#22197 = ORIENTED_EDGE ( 'NONE', *, *, #2049, .F. ) ;
#22198 = CARTESIAN_POINT ( 'NONE',  ( -10.41614636368765900, -13.97037319380632248, 64.53236772669211518 ) ) ;
#22199 = DIRECTION ( 'NONE',  ( 0.3964226963016398431, 0.9180681052388965924, 0.000000000000000000 ) ) ;
#22200 = CARTESIAN_POINT ( 'NONE',  ( -11.92015382652974154, -10.40338788426078587, 70.97452903744414243 ) ) ;
#22201 = CARTESIAN_POINT ( 'NONE',  ( -10.79744568551467587, -12.55229167313659921, 60.81470185434422859 ) ) ;
#22202 = CARTESIAN_POINT ( 'NONE',  ( -17.06612543921954028, -7.818304145033148522, 70.71709262193978418 ) ) ;
#22203 = ORIENTED_EDGE ( 'NONE', *, *, #20716, .F. ) ;
#22204 = EDGE_LOOP ( 'NONE', ( #23024, #29743, #13715, #30686, #37997 ) ) ;
#22205 = CARTESIAN_POINT ( 'NONE',  ( -11.06712688165958269, -18.69414528815109477, 61.39215548186584215 ) ) ;
#22206 = CARTESIAN_POINT ( 'NONE',  ( -45.55409385541305767, -13.24559821555319061, 69.99777223794900749 ) ) ;
#22207 = ORIENTED_EDGE ( 'NONE', *, *, #48001, .T. ) ;
#22208 = B_SPLINE_CURVE_WITH_KNOTS ( 'NONE', 1,
 ( #13226, #43549 ),
 .UNSPECIFIED., .F., .F.,
 ( 2, 2 ),
 ( 0.000000000000000000, 1.000000000000000000 ),
 .UNSPECIFIED. ) ;
#22209 = DIRECTION ( 'NONE',  ( -3.071710424422018668E-17, 6.404604876783312462E-16, 1.000000000000000000 ) ) ;
#22210 = CARTESIAN_POINT ( 'NONE',  ( -10.71495554099518088, -12.81234323494808436, 64.56836111193433680 ) ) ;
#22211 = CARTESIAN_POINT ( 'NONE',  ( -20.68242297322939649, -8.109334927485972955, 63.44975001546675486 ) ) ;
#22212 = CARTESIAN_POINT ( 'NONE',  ( -12.60165769527841384, -19.96275654529059906, 61.55245915020547898 ) ) ;
#22213 = FACE_BOUND ( 'NONE', #37518, .T. ) ;
#22214 = DIRECTION ( 'NONE',  ( -3.071710424422018668E-17, 6.404604876783312462E-16, 1.000000000000000000 ) ) ;
#22215 = DIRECTION ( 'NONE',  ( 0.9918916210775228226, 0.1270866320121812332, -6.503929235867083869E-08 ) ) ;
#22216 = B_SPLINE_CURVE_WITH_KNOTS ( 'NONE', 3,
 ( #38323, #31198, #45983, #9045, #4612, #19635, #24062, #5105, #16653, #46709 ),
 .UNSPECIFIED., .F., .F.,
 ( 4, 2, 2, 2, 4 ),
 ( 0.1272669073658303229, 0.2522669073463129630, 0.3772669073267956863, 0.5022669073072782986, 0.6272669072877610219 ),
 .UNSPECIFIED. ) ;
#22217 = CYLINDRICAL_SURFACE ( 'NONE', #9454, 0.1500000000000013267 ) ;
#22218 = EDGE_CURVE ( 'NONE', #20093, #44110, #20476, .T. ) ;
#22219 = VERTEX_POINT ( 'NONE', #5728 ) ;
#22220 = CYLINDRICAL_SURFACE ( 'NONE', #13271, 1.999999999999999556 ) ;
#22221 = CARTESIAN_POINT ( 'NONE',  ( -11.60479079619936371, -10.15731510490028100, 71.09176221476478474 ) ) ;
#22222 = CARTESIAN_POINT ( 'NONE',  ( -19.83021750621371737, -21.38439240218873039, 72.58761523121964387 ) ) ;
#22223 = CARTESIAN_POINT ( 'NONE',  ( -17.42558057905623059, -9.559206755253617516, 52.02966884056656482 ) ) ;
#22224 = CARTESIAN_POINT ( 'NONE',  ( -15.43182990062313564, -8.046249867383863830, 74.36513541778452918 ) ) ;
#22225 = CARTESIAN_POINT ( 'NONE',  ( -10.42496409799848323, -14.69883155267435626, 71.62782692796884021 ) ) ;
#22226 = EDGE_LOOP ( 'NONE', ( #6285, #48012, #42560, #8356 ) ) ;
#22227 = ORIENTED_EDGE ( 'NONE', *, *, #4641, .F. ) ;
#22228 = CARTESIAN_POINT ( 'NONE',  ( -14.48034385541304125, -9.360768649639302552, 51.01397948905922419 ) ) ;
#22229 = EDGE_CURVE ( 'NONE', #40825, #36429, #12, .T. ) ;
#22230 = VERTEX_POINT ( 'NONE', #17505 ) ;
#22231 = DIRECTION ( 'NONE',  ( -4.115385489419834812E-17, -0.9999954153791275058, -0.003028072113822189229 ) ) ;
#22232 = ADVANCED_FACE ( 'NONE', ( #28608 ), #13320, .T. ) ;
#22233 = CARTESIAN_POINT ( 'NONE',  ( -20.13067905174874639, -8.351893152775456741, 73.83169569948991295 ) ) ;
#22234 = ADVANCED_FACE ( 'NONE', ( #32536 ), #14035, .T. ) ;
#22235 = CARTESIAN_POINT ( 'NONE',  ( -20.47409385759799250, -6.859212275519751323, 50.50378509014259265 ) ) ;
#22236 = CARTESIAN_POINT ( 'NONE',  ( -24.72409385541305582, -14.80920654474413745, 60.91764705882351905 ) ) ;
#22237 = ORIENTED_EDGE ( 'NONE', *, *, #48263, .T. ) ;
#22238 = CARTESIAN_POINT ( 'NONE',  ( -24.38143503755601316, -15.58083059521001168, 73.30303748419844112 ) ) ;
#22239 = PLANE ( 'NONE',  #13935 ) ;
#22240 = EDGE_LOOP ( 'NONE', ( #15749, #41532, #16639, #13571 ) ) ;
#22241 =( BOUNDED_CURVE ( )  B_SPLINE_CURVE ( 3, ( #31836, #13098, #43163, #24462 ),
 .UNSPECIFIED., .F., .F. ) 
 B_SPLINE_CURVE_WITH_KNOTS ( ( 4, 4 ),
 ( 0.5000000000000000000, 0.9074455897393643999 ),
 .UNSPECIFIED. ) 
 CURVE ( )  GEOMETRIC_REPRESENTATION_ITEM ( )  RATIONAL_B_SPLINE_CURVE ( ( 1.000000000000017542, 0.4567392136813297476, 0.3561768502900171107, 0.6983129098260985046 ) ) 
 REPRESENTATION_ITEM ( '' )  );
#22242 = LINE ( 'NONE', #3514, #39873 ) ;
#22243 = CARTESIAN_POINT ( 'NONE',  ( -11.53247150430815715, -18.68106468654471541, 64.89707076448696910 ) ) ;
#22244 = VERTEX_POINT ( 'NONE', #39684 ) ;
#22245 = CARTESIAN_POINT ( 'NONE',  ( -17.76182844141538553, -7.366698643885237985, 60.21914265551018275 ) ) ;
#22246 = CARTESIAN_POINT ( 'NONE',  ( -21.36284888653444725, -21.13297021396988384, 69.16954901539321554 ) ) ;
#22247 = FACE_OUTER_BOUND ( 'NONE', #24378, .T. ) ;
#22248 = ORIENTED_EDGE ( 'NONE', *, *, #13877, .F. ) ;
#22249 = CARTESIAN_POINT ( 'NONE',  ( -10.70297003644833644, -11.59513240183115279, 71.27356180636090244 ) ) ;
#22250 = DIRECTION ( 'NONE',  ( 0.9584484254710482487, 0.2852658684667118694, -3.516456353195806577E-08 ) ) ;
#22251 = CARTESIAN_POINT ( 'NONE',  ( -15.11195812866605692, -21.41632606413040918, 65.10596681519622564 ) ) ;
#22252 = CARTESIAN_POINT ( 'NONE',  ( -22.22496508270376481, -20.50616197626463233, 58.80796965402809917 ) ) ;
#22253 = ORIENTED_EDGE ( 'NONE', *, *, #26053, .F. ) ;
#22254 = CARTESIAN_POINT ( 'NONE',  ( -24.68275079258767235, -16.48720463981601370, 59.23837148777906236 ) ) ;
#22255 = CARTESIAN_POINT ( 'NONE',  ( 8.575906144586951996, -6.109215713985405749, 50.50605614422795497 ) ) ;
#22257 =( BOUNDED_CURVE ( )  B_SPLINE_CURVE ( 3, ( #6179, #21201, #35957, #47312 ),
 .UNSPECIFIED., .F., .F. ) 
 B_SPLINE_CURVE_WITH_KNOTS ( ( 4, 4 ),
 ( 0.000000000000000000, 0.4074455897393615689 ),
 .UNSPECIFIED. ) 
 CURVE ( )  GEOMETRIC_REPRESENTATION_ITEM ( )  RATIONAL_B_SPLINE_CURVE ( ( 1.000000000000000000, 0.4567392136813364090, 0.3561768502900319322, 0.6983129098260865142 ) ) 
 REPRESENTATION_ITEM ( '' )  );
#22256 = CARTESIAN_POINT ( 'NONE',  ( -20.16691314815865255, -21.73601827195274794, 72.58974169946205279 ) ) ;
#22258 = CARTESIAN_POINT ( 'NONE',  ( -16.45566506110110438, -21.79267588865899086, 62.04095995016087528 ) ) ;
#22259 = CARTESIAN_POINT ( 'NONE',  ( -21.28659385650551528, -9.302874398569244363, 51.68646062012417985 ) ) ;
#22260 = ORIENTED_EDGE ( 'NONE', *, *, #5099, .F. ) ;
#22261 = CARTESIAN_POINT ( 'NONE',  ( -20.72573962529263625, -8.580110715261016097, 59.99125250080121674 ) ) ;
#22262 = CARTESIAN_POINT ( 'NONE',  ( -24.32852063849251323, -13.38246526728995001, 59.37740068604990995 ) ) ;
#22263 = VERTEX_POINT ( 'NONE', #28115 ) ;
#22264 = CARTESIAN_POINT ( 'NONE',  ( -16.98991614605047218, -22.24663000551990777, 72.35038637723081933 ) ) ;
#22265 = LINE ( 'NONE', #29652, #3020 ) ;
#22266 = DIRECTION ( 'NONE',  ( 0.000000000000000000, -0.9999954153791273948, -0.003028072113819836944 ) ) ;
#22267 = ADVANCED_FACE ( 'NONE', ( #21463 ), #21221, .T. ) ;
#22268 = ORIENTED_EDGE ( 'NONE', *, *, #35505, .T. ) ;
#22269 = CARTESIAN_POINT ( 'NONE',  ( -17.96784385541291940, -9.357632978295868043, 49.97845033065662790 ) ) ;
#22270 = DIRECTION ( 'NONE',  ( -5.731567514496413899E-31, -1.020425574103664789E-16, -1.000000000000000000 ) ) ;
#22271 = ORIENTED_EDGE ( 'NONE', *, *, #47313, .F. ) ;
#22272 = VERTEX_POINT ( 'NONE', #46834 ) ;
#22273 = AXIS2_PLACEMENT_3D ( 'NONE', #21024, #1579, #43690 ) ;
#22274 = CARTESIAN_POINT ( 'NONE',  ( -15.04284385650551670, -8.811426318492348031, 52.18089403414752070 ) ) ;
#22275 = DIRECTION ( 'NONE',  ( -0.5420872618288282707, -0.8403222004463035688, 7.592316861452269267E-08 ) ) ;
#22276 = CARTESIAN_POINT ( 'NONE',  ( -46.29409385541305255, -14.20920654474410760, 70.08498674719956512 ) ) ;
#22277 = CARTESIAN_POINT ( 'NONE',  ( -10.72552546848295485, -12.61109793159036485, 61.09853568372136579 ) ) ;
#22278 = CARTESIAN_POINT ( 'NONE',  ( -45.92409385541306222, -14.20920654474410760, 70.50000000000000000 ) ) ;
#22279 = ORIENTED_EDGE ( 'NONE', *, *, #15124, .F. ) ;
#22280 = VERTEX_POINT ( 'NONE', #28839 ) ;
#22281 = CARTESIAN_POINT ( 'NONE',  ( -14.17409385650551457, -9.792211528768504536, 50.49490371617623197 ) ) ;
#22282 = EDGE_CURVE ( 'NONE', #30016, #20100, #22124, .T. ) ;
#22283 = FACE_OUTER_BOUND ( 'NONE', #11490, .T. ) ;
#22284 = CARTESIAN_POINT ( 'NONE',  ( -12.96596342764269316, -9.347744029417796696, 71.14925352873375175 ) ) ;
#22285 = EDGE_CURVE ( 'NONE', #46722, #12016, #13081, .T. ) ;
#22286 = CARTESIAN_POINT ( 'NONE',  ( -16.48034385650551670, -6.424090610841176385, 49.80797279389977916 ) ) ;
#22287 = ORIENTED_EDGE ( 'NONE', *, *, #26839, .T. ) ;
#22288 = EDGE_CURVE ( 'NONE', #44188, #21060, #40914, .T. ) ;
#22289 = DIRECTION ( 'NONE',  ( 0.9687793358424821033, -0.2479245821708677133, 0.000000000000000000 ) ) ;
#22290 = DIRECTION ( 'NONE',  ( 6.517531090241554163E-16, 1.000000000000000000, 1.799495156056576137E-30 ) ) ;
#22291 = CARTESIAN_POINT ( 'NONE',  ( -16.16379449968008331, -22.15191876840708929, 58.47080954035841671 ) ) ;
#22292 = ADVANCED_FACE ( 'NONE', ( #10135 ), #29014, .T. ) ;
#22293 = ORIENTED_EDGE ( 'NONE', *, *, #13746, .T. ) ;
#22294 = CARTESIAN_POINT ( 'NONE',  ( -24.41897151118743636, -17.37347349776957017, 69.59835227440868266 ) ) ;
#22295 = EDGE_CURVE ( 'NONE', #10862, #23394, #3158, .T. ) ;
#22296 = B_SPLINE_CURVE_WITH_KNOTS ( 'NONE', 1,
 ( #17778, #21733 ),
 .UNSPECIFIED., .F., .F.,
 ( 2, 2 ),
 ( 0.000000000000000000, 1.000000000000000000 ),
 .UNSPECIFIED. ) ;
#22297 = ORIENTED_EDGE ( 'NONE', *, *, #27763, .F. ) ;
#22298 = CARTESIAN_POINT ( 'NONE',  ( -12.52591642561268515, -9.195683996340104471, 74.50418400381258266 ) ) ;
#22299 = CARTESIAN_POINT ( 'NONE',  ( -24.30048628764226137, -16.36411057843138650, 59.27332431757403697 ) ) ;
#22300 = FACE_OUTER_BOUND ( 'NONE', #42492, .T. ) ;
#22301 = CARTESIAN_POINT ( 'NONE',  ( -9.990123186454296089, -14.31889395325652714, 64.50991104586785241 ) ) ;
#22302 = CIRCLE ( 'NONE', #27052, 2.000000000000001776 ) ;
#22303 = ORIENTED_EDGE ( 'NONE', *, *, #37086, .T. ) ;
#22304 = DIRECTION ( 'NONE',  ( 0.9687793358424817702, -0.2479245821708684905, 0.000000000000000000 ) ) ;
#22305 = CARTESIAN_POINT ( 'NONE',  ( -24.19823205308740910, -11.70861652093786454, 59.68246929106484799 ) ) ;
#22306 = DIRECTION ( 'NONE',  ( -0.7437128929774847741, 0.6684991644116393683, -1.736198598217016398E-08 ) ) ;
#22307 = DIRECTION ( 'NONE',  ( 2.671295499615842957E-06, 1.272698189891367967E-05, 0.9999999999154439712 ) ) ;
#22308 = ORIENTED_EDGE ( 'NONE', *, *, #12879, .F. ) ;
#22309 = DIRECTION ( 'NONE',  ( 0.4461977533475104396, 0.8949343913984053600, 0.000000000000000000 ) ) ;
#22310 = DIRECTION ( 'NONE',  ( -1.000000000000000000, 0.000000000000000000, 0.000000000000000000 ) ) ;
#22311 = ORIENTED_EDGE ( 'NONE', *, *, #1916, .F. ) ;
#22312 = FACE_BOUND ( 'NONE', #25395, .T. ) ;
#22313 = ORIENTED_EDGE ( 'NONE', *, *, #8674, .T. ) ;
#22314 = DIRECTION ( 'NONE',  ( 0.9180681052388952601, -0.3964226963016432292, 0.000000000000000000 ) ) ;
#22315 = CARTESIAN_POINT ( 'NONE',  ( -13.61033894779295395, -20.67921429907312003, 61.81646270068954152 ) ) ;
#22316 = FACE_OUTER_BOUND ( 'NONE', #9779, .T. ) ;
#22317 = DIRECTION ( 'NONE',  ( -3.071710424422018668E-17, 6.404604876783312462E-16, 1.000000000000000000 ) ) ;
#22318 = ORIENTED_EDGE ( 'NONE', *, *, #23198, .T. ) ;
#22319 = CARTESIAN_POINT ( 'NONE',  ( -10.45160180800373873, -14.17496150716750769, 64.45974129894086957 ) ) ;
#22320 = VERTEX_POINT ( 'NONE', #48036 ) ;
#22321 = PLANE ( 'NONE',  #46313 ) ;
#22322 = CARTESIAN_POINT ( 'NONE',  ( -10.97344478688443914, -18.53636807463781722, 58.00725798456583959 ) ) ;
#22323 = EDGE_CURVE ( 'NONE', #8916, #36242, #39095, .T. ) ;
#22324 = CARTESIAN_POINT ( 'NONE',  ( -10.61330328728660533, -12.98831903967553814, 67.73832347272892207 ) ) ;
#22325 = ORIENTED_EDGE ( 'NONE', *, *, #28446, .T. ) ;
#22326 = CARTESIAN_POINT ( 'NONE',  ( -13.47643240338711124, -20.58993545956319338, 58.33184665923734968 ) ) ;
#22327 = VERTEX_POINT ( 'NONE', #11583 ) ;
#22328 = ORIENTED_EDGE ( 'NONE', *, *, #38370, .F. ) ;
#22329 = LINE ( 'NONE', #47948, #17818 ) ;
#22330 = FACE_OUTER_BOUND ( 'NONE', #42285, .T. ) ;
#22331 = CARTESIAN_POINT ( 'NONE',  ( -21.93774155219031385, -8.882177397035567523, 66.76175749538603554 ) ) ;
#22332 = CARTESIAN_POINT ( 'NONE',  ( -20.69509252757554307, -8.115601716887088202, 63.49616818922779515 ) ) ;
#22333 = DIRECTION ( 'NONE',  ( 0.2664710960620865210, -0.9638429098994647504, 4.833213314675751572E-08 ) ) ;
#22334 = CARTESIAN_POINT ( 'NONE',  ( -14.23114477490021379, -8.578028806345869839, 74.38881623979730762 ) ) ;
#22335 = EDGE_CURVE ( 'NONE', #23362, #27190, #22725, .T. ) ;
#22336 = CARTESIAN_POINT ( 'NONE',  ( -17.85497298213014261, -7.371550647135725498, 60.20343865544412409 ) ) ;
#22337 = ORIENTED_EDGE ( 'NONE', *, *, #30293, .F. ) ;
#22338 = ORIENTED_EDGE ( 'NONE', *, *, #24628, .F. ) ;
#22339 = VECTOR ( 'NONE', #29288, 1000.000000000000000 ) ;
#22340 = CARTESIAN_POINT ( 'NONE',  ( -12.15423770757536026, -10.20156791825057496, 64.32914322081802538 ) ) ;
#22341 = AXIS2_PLACEMENT_3D ( 'NONE', #22498, #33303, #33807 ) ;
#22342 = CARTESIAN_POINT ( 'NONE',  ( -22.53028194631272640, -20.23415643105539274, 65.81083435350976174 ) ) ;
#22343 = FACE_OUTER_BOUND ( 'NONE', #7294, .T. ) ;
#22344 = CARTESIAN_POINT ( 'NONE',  ( -16.22409385541304871, -9.359200813967568422, 50.49621490985801842 ) ) ;
#22345 = EDGE_LOOP ( 'NONE', ( #15147, #23243, #44616, #47145, #32487, #30035, #36173 ) ) ;
#22346 = CARTESIAN_POINT ( 'NONE',  ( -15.26784385650551989, -6.428312510596451368, 51.20221977374900035 ) ) ;
#22347 = ORIENTED_EDGE ( 'NONE', *, *, #226, .F. ) ;
#22348 = ADVANCED_FACE ( 'NONE', ( #37417 ), #11102, .T. ) ;
#22349 = FACE_OUTER_BOUND ( 'NONE', #33563, .T. ) ;
#22350 = CARTESIAN_POINT ( 'NONE',  ( -23.98474789688958353, -17.25007084823549874, 69.71339792561613535 ) ) ;
#22351 = EDGE_CURVE ( 'NONE', #40523, #17101, #10245, .T. ) ;
#22352 = CARTESIAN_POINT ( 'NONE',  ( -10.03016176022630646, -13.89628074529801438, 57.49179087295118507 ) ) ;
#22353 = ADVANCED_FACE ( 'NONE', ( #10612 ), #26, .T. ) ;
#22354 = VERTEX_POINT ( 'NONE', #40888 ) ;
#22355 = DIRECTION ( 'NONE',  ( -0.9687793358424822143, 0.2479245821708672415, 0.000000000000000000 ) ) ;
#22356 = CARTESIAN_POINT ( 'NONE',  ( -24.18470913683765389, -12.80901137141652768, 69.78715111652664405 ) ) ;
#22357 = ORIENTED_EDGE ( 'NONE', *, *, #43794, .T. ) ;
#22358 = CARTESIAN_POINT ( 'NONE',  ( -15.25439996314754509, -21.46446225238890904, 65.29699935524728005 ) ) ;
#22359 = ADVANCED_FACE ( 'NONE', ( #3966 ), #40379, .T. ) ;
#22360 = FACE_OUTER_BOUND ( 'NONE', #16987, .T. ) ;
#22361 = DIRECTION ( 'NONE',  ( 0.000000000000000000, 1.000000000000000000, 0.000000000000000000 ) ) ;
#22362 = ORIENTED_EDGE ( 'NONE', *, *, #1459, .T. ) ;
#22363 = B_SPLINE_CURVE_WITH_KNOTS ( 'NONE', 3,
 ( #24195, #39452, #39202, #30683, #30441, #45708, #38961, #1784, #2018, #41997 ),
 .UNSPECIFIED., .F., .F.,
 ( 4, 2, 2, 2, 4 ),
 ( 0.1272669073658251604, 0.2522669073463064682, 0.3772669073267878037, 0.5022669073072690837, 0.6272669072877503638 ),
 .UNSPECIFIED. ) ;
#22364 = CARTESIAN_POINT ( 'NONE',  ( -24.69852204723760281, -16.41745771733451775, 59.30827817708741634 ) ) ;
#22365 = EDGE_CURVE ( 'NONE', #1410, #47208, #31515, .T. ) ;
#22366 = ORIENTED_EDGE ( 'NONE', *, *, #41940, .F. ) ;
#22367 = AXIS2_PLACEMENT_3D ( 'NONE', #18068, #13645, #44220 ) ;
#22368 = CARTESIAN_POINT ( 'NONE',  ( -10.31133302210429470, -17.02573883484783579, 57.81043661216028084 ) ) ;
#22369 = CARTESIAN_POINT ( 'NONE',  ( -11.57425704488359841, -18.65360627554439077, 65.04707076833931012 ) ) ;
#22370 = ORIENTED_EDGE ( 'NONE', *, *, #39278, .T. ) ;
#22371 = EDGE_CURVE ( 'NONE', #3267, #19390, #816, .T. ) ;
#22372 = ADVANCED_FACE ( 'NONE', ( #15989 ), #8381, .F. ) ;
#22373 = PLANE ( 'NONE',  #13198 ) ;
#22374 = AXIS2_PLACEMENT_3D ( 'NONE', #13520, #28065, #24144 ) ;
#22375 = CARTESIAN_POINT ( 'NONE',  ( -18.59773863799375349, -22.16623006980740129, 72.39172614962501484 ) ) ;
#22376 = ORIENTED_EDGE ( 'NONE', *, *, #4529, .T. ) ;
#22377 = CARTESIAN_POINT ( 'NONE',  ( -22.92319923916556235, -10.39759239192951590, 63.07185995337423634 ) ) ;
#22378 =( BOUNDED_SURFACE ( )  B_SPLINE_SURFACE ( 3, 1, ( 
 ( #20094, #46450 ),
 ( #34618, #35100 ),
 ( #23561, #20343 ),
 ( #31419, #5085 ),
 ( #42755, #24045 ),
 ( #904, #1366 ),
 ( #15902, #42268 ) ),
 .UNSPECIFIED., .T., .F., .F. ) 
 B_SPLINE_SURFACE_WITH_KNOTS ( ( 4, 3, 4 ),
 ( 2, 2 ),
 ( 0.000000000000000000, 0.5000000000000000000, 1.000000000000000000 ),
 ( 0.000000000000000000, 1.000000000000000000 ),
 .UNSPECIFIED. ) 
 GEOMETRIC_REPRESENTATION_ITEM ( )  RATIONAL_B_SPLINE_SURFACE ( (
 ( 1.000000000000000000, 1.000000000000000000),
 ( 0.3333333333333335369, 0.3333333333333330373),
 ( 0.3333333333333335369, 0.3333333333333330373),
 ( 1.000000000000000000, 1.000000000000000000),
 ( 0.3333333333333333703, 0.3333333333333333703),
 ( 0.3333333333333333703, 0.3333333333333333703),
 ( 1.000000000000000000, 1.000000000000000000) ) ) 
 REPRESENTATION_ITEM ( '' )  SURFACE ( )  );
#22379 = CARTESIAN_POINT ( 'NONE',  ( -16.00544582274271477, -7.903112417841744453, 63.95538887075813506 ) ) ;
#22380 = CARTESIAN_POINT ( 'NONE',  ( -24.41485939984550058, -14.44976655980182834, 66.48292729254383460 ) ) ;
#22381 = ORIENTED_EDGE ( 'NONE', *, *, #26179, .T. ) ;
#22382 = CARTESIAN_POINT ( 'NONE',  ( -19.17551372071283922, -8.031400147991478278, 63.44705914822644388 ) ) ;
#22383 = LINE ( 'NONE', #18186, #45927 ) ;
#22384 = EDGE_LOOP ( 'NONE', ( #4322, #47150, #24531, #41254 ) ) ;
#22385 = ORIENTED_EDGE ( 'NONE', *, *, #16524, .F. ) ;
#22386 = DIRECTION ( 'NONE',  ( -2.867370864192053523E-15, -0.4461977533475100510, 0.8949343913984055821 ) ) ;
#22387 = CARTESIAN_POINT ( 'NONE',  ( -50.42609385541305755, -14.80920654474418008, 64.04117647058822627 ) ) ;
#22388 = CARTESIAN_POINT ( 'NONE',  ( 7.325906144586953772, -0.1092432217106413528, 50.52422457691088908 ) ) ;
#22389 = DIRECTION ( 'NONE',  ( 1.000000000000000000, 1.669677910507523057E-21, 6.493791346278465266E-22 ) ) ;
#22390 = CARTESIAN_POINT ( 'NONE',  ( -15.18659385759799108, -7.222650657624104298, 49.61879703869476543 ) ) ;
#22391 = CARTESIAN_POINT ( 'NONE',  ( -19.88388893082392528, -8.193741602349351894, 70.40667630031393287 ) ) ;
#22392 = CARTESIAN_POINT ( 'NONE',  ( -12.40538917401127961, -20.31523793222865493, 68.52152763170285255 ) ) ;
#22393 = CARTESIAN_POINT ( 'NONE',  ( -24.31823774515246939, -17.63313259158020685, 66.05861911469568781 ) ) ;
#22394 =( BOUNDED_CURVE ( )  B_SPLINE_CURVE ( 3, ( #41904, #42146, #8182, #8410 ),
 .UNSPECIFIED., .F., .F. ) 
 B_SPLINE_CURVE_WITH_KNOTS ( ( 4, 4 ),
 ( 0.4074455897393676751, 0.5000000000000000000 ),
 .UNSPECIFIED. ) 
 CURVE ( )  GEOMETRIC_REPRESENTATION_ITEM ( )  RATIONAL_B_SPLINE_CURVE ( ( 0.6983129098260865142, 0.7760317562606877662, 0.8765941196519909662, 0.9999999999999924505 ) ) 
 REPRESENTATION_ITEM ( '' )  );
#22395 = CYLINDRICAL_SURFACE ( 'NONE', #29207, 5.249999999999998224 ) ;
#22396 = ORIENTED_EDGE ( 'NONE', *, *, #16694, .F. ) ;
#22397 = CARTESIAN_POINT ( 'NONE',  ( -12.76547314785493192, -9.517330534081262172, 74.60450883341005124 ) ) ;
#22398 = ADVANCED_FACE ( 'NONE', ( #41879 ), #34720, .T. ) ;
#22399 = DIRECTION ( 'NONE',  ( 0.2122660683108583690, -0.9772119095896469876, 7.504255179194988334E-08 ) ) ;
#22400 = DIRECTION ( 'NONE',  ( 7.404863042181874502E-06, -6.320720312887485007E-06, 0.9999999999526082428 ) ) ;
#22401 = ORIENTED_EDGE ( 'NONE', *, *, #24897, .T. ) ;
#22402 =( BOUNDED_CURVE ( )  B_SPLINE_CURVE ( 3, ( #6901, #25608, #44347, #10599 ),
 .UNSPECIFIED., .F., .F. ) 
 B_SPLINE_CURVE_WITH_KNOTS ( ( 4, 4 ),
 ( 0.9074455897393601811, 1.000000000000000000 ),
 .UNSPECIFIED. ) 
 CURVE ( )  GEOMETRIC_REPRESENTATION_ITEM ( )  RATIONAL_B_SPLINE_CURVE ( ( 0.6983129098260714152, 0.7760317562606795505, 0.8765941196519890788, 1.000000000000000000 ) ) 
 REPRESENTATION_ITEM ( '' )  );
#22403 = AXIS2_PLACEMENT_3D ( 'NONE', #27765, #2140, #5620 ) ;
#22404 = EDGE_LOOP ( 'NONE', ( #36146, #44483 ) ) ;
#22405 = ADVANCED_FACE ( 'NONE', ( #20185 ), #1221, .T. ) ;
#22406 = DIRECTION ( 'NONE',  ( 1.000000000000000000, 0.000000000000000000, 0.000000000000000000 ) ) ;
#22407 = VECTOR ( 'NONE', #48539, 1000.000000000000000 ) ;
#22408 = CARTESIAN_POINT ( 'NONE',  ( -10.61357140615669792, -13.19155887971477448, 71.50828586566468914 ) ) ;
#22409 = CARTESIAN_POINT ( 'NONE',  ( -15.33251096848727002, -21.95963115018486533, 72.15301311573767862 ) ) ;
#22410 = LINE ( 'NONE', #4197, #21736 ) ;
#22411 = B_SPLINE_CURVE_WITH_KNOTS ( 'NONE', 3,
 ( #30287, #30044, #45550, #965, #19680, #15467, #22903, #26830, #41850, #37641 ),
 .UNSPECIFIED., .F., .F.,
 ( 4, 2, 2, 2, 4 ),
 ( 0.1272669073658187489, 0.2522669073463080780, 0.3772669073267974627, 0.5022669073072867363, 0.6272669072877761209 ),
 .UNSPECIFIED. ) ;
#22412 = ORIENTED_EDGE ( 'NONE', *, *, #10241, .F. ) ;
#22413 = CARTESIAN_POINT ( 'NONE',  ( -17.42409385541299471, -14.80920654474435594, 52.02966884056656482 ) ) ;
#22414 = EDGE_LOOP ( 'NONE', ( #8164, #8290, #3698, #2001 ) ) ;
#22415 = CARTESIAN_POINT ( 'NONE',  ( -22.14090652532222236, -20.04928072148792495, 62.51967078134249078 ) ) ;
#22416 = DIRECTION ( 'NONE',  ( 4.115385489419721413E-17, 0.9999954153791273948, 0.003028072113829171491 ) ) ;
#22417 = CARTESIAN_POINT ( 'NONE',  ( -24.41089624436030547, -15.77327213725850719, 65.94836039739031719 ) ) ;
#22418 = ORIENTED_EDGE ( 'NONE', *, *, #43731, .T. ) ;
#22419 = DIRECTION ( 'NONE',  ( -2.866981220435666553E-17, 1.000000000000000000, 1.190614954331866791E-16 ) ) ;
#22420 = ADVANCED_FACE ( 'NONE', ( #31037 ), #46051, .T. ) ;
#22421 = ORIENTED_EDGE ( 'NONE', *, *, #8427, .F. ) ;
#22422 = CARTESIAN_POINT ( 'NONE',  ( -23.77946760588002562, -10.92150643066187143, 73.50046759018312059 ) ) ;
#22423 = DIRECTION ( 'NONE',  ( -3.071710424422018668E-17, 6.404604876783312462E-16, 1.000000000000000000 ) ) ;
#22424 = ORIENTED_EDGE ( 'NONE', *, *, #35235, .F. ) ;
#22425 = CARTESIAN_POINT ( 'NONE',  ( -13.54792730259346456, -8.920061342218058797, 57.25495614889487683 ) ) ;
#22426 = EDGE_CURVE ( 'NONE', #19220, #34107, #10328, .T. ) ;
#22427 = EDGE_CURVE ( 'NONE', #20224, #3327, #1583, .T. ) ;
#22428 = CARTESIAN_POINT ( 'NONE',  ( -24.40658474706614101, -15.78251040532600769, 69.68307488409816131 ) ) ;
#22429 = CARTESIAN_POINT ( 'NONE',  ( -21.71159385650551599, -6.922745924619793101, 51.69366785382590024 ) ) ;
#22430 = CARTESIAN_POINT ( 'NONE',  ( -21.42336380182764088, -21.09487415076890215, 69.23945570945444672 ) ) ;
#22431 = CARTESIAN_POINT ( 'NONE',  ( -6.424093855413058662, -6.359206544744109735, 52.99999999999998579 ) ) ;
#22432 = DIRECTION ( 'NONE',  ( -0.6621635203543606574, -0.7493593746073508033, -2.316976118889527729E-08 ) ) ;
#22433 = ORIENTED_EDGE ( 'NONE', *, *, #9889, .F. ) ;
#22434 = CARTESIAN_POINT ( 'NONE',  ( -12.16006207029921171, -10.11953296189675733, 64.02914329232321222 ) ) ;
#22435 = DIRECTION ( 'NONE',  ( -0.8743548079231422410, -0.4852872034802500067, 5.778319183281968808E-08 ) ) ;
#22436 = CARTESIAN_POINT ( 'NONE',  ( -18.26342096751342581, -21.75870509638779993, 65.53635344041087762 ) ) ;
#22437 = CIRCLE ( 'NONE', #10629, 4.686499999999998778 ) ;
#22438 = ADVANCED_FACE ( 'NONE', ( #45820 ), #509, .T. ) ;
#22439 = EDGE_CURVE ( 'NONE', #19879, #3652, #35346, .T. ) ;
#22440 = PLANE ( 'NONE',  #13209 ) ;
#22441 = DIRECTION ( 'NONE',  ( -5.731567514496413899E-31, -1.020425574103664789E-16, -1.000000000000000000 ) ) ;
#22442 = FACE_OUTER_BOUND ( 'NONE', #10038, .T. ) ;
#22443 = AXIS2_PLACEMENT_3D ( 'NONE', #30033, #42262, #4583 ) ;
#22444 = EDGE_LOOP ( 'NONE', ( #22698, #3351, #33346, #26202 ) ) ;
#22445 = ORIENTED_EDGE ( 'NONE', *, *, #31345, .T. ) ;
#22446 = CARTESIAN_POINT ( 'NONE',  ( -23.96044199021409327, -11.23292130238350772, 66.53559200982742539 ) ) ;
#22447 = CARTESIAN_POINT ( 'NONE',  ( -16.94712425470457973, -14.65920654474411045, 48.99999999999997868 ) ) ;
#22448 = ORIENTED_EDGE ( 'NONE', *, *, #32541, .F. ) ;
#22449 = B_SPLINE_CURVE_WITH_KNOTS ( 'NONE', 3,
 ( #2052, #25198, #32805, #21263, #2546, #44175, #10424, #17051, #24950, #36013 ),
 .UNSPECIFIED., .F., .F.,
 ( 4, 2, 2, 2, 4 ),
 ( 0.1272669073658731220, 0.2522669073439754439, 0.3772669073220777936, 0.5022669073001800877, 0.6272669072782823818 ),
 .UNSPECIFIED. ) ;
#22451 = CARTESIAN_POINT ( 'NONE',  ( -18.01624426275133217, -7.780493777692311319, 60.17240823276083006 ) ) ;
#22450 = CARTESIAN_POINT ( 'NONE',  ( -15.35027035934970918, -7.653577032698213323, 74.26481056556292515 ) ) ;
#22452 = DIRECTION ( 'NONE',  ( 0.000000000000000000, 0.000000000000000000, 1.000000000000000000 ) ) ;
#22453 = CARTESIAN_POINT ( 'NONE',  ( -21.82220603157065497, -9.299244845878236632, 63.49153740581677141 ) ) ;
#22454 = CARTESIAN_POINT ( 'NONE',  ( -14.54324430907851173, -21.67975036377454501, 58.42263788831355953 ) ) ;
#22455 = FACE_BOUND ( 'NONE', #4268, .T. ) ;
#22456 = CARTESIAN_POINT ( 'NONE',  ( -19.56876505180931147, -21.94388403446443903, 62.10165325708241113 ) ) ;
#22457 = CARTESIAN_POINT ( 'NONE',  ( -23.33263663379104713, -18.66181210963279469, 72.85548507352433489 ) ) ;
#22458 = CARTESIAN_POINT ( 'NONE',  ( -19.36557164464469594, -19.08778335711046026, 49.52966884056656482 ) ) ;
#22459 = DIRECTION ( 'NONE',  ( 0.09332174201254166135, 0.9956360040033429559, 0.000000000000000000 ) ) ;
#22460 = ADVANCED_FACE ( 'NONE', ( #22935 ), #42361, .T. ) ;
#22461 = ORIENTED_EDGE ( 'NONE', *, *, #30013, .F. ) ;
#22462 = DIRECTION ( 'NONE',  ( -0.9687793358424819923, 0.2479245821708677688, 0.000000000000000000 ) ) ;
#22463 = CARTESIAN_POINT ( 'NONE',  ( -15.54561766592941119, -8.065849124998859310, 74.07985694182616498 ) ) ;
#22464 = CARTESIAN_POINT ( 'NONE',  ( -20.47409385759799250, -6.859212275519751323, 50.50378509014259265 ) ) ;
#22465 = FACE_OUTER_BOUND ( 'NONE', #34808, .T. ) ;
#22466 = DIRECTION ( 'NONE',  ( -2.866981220435666553E-17, 1.000000000000000000, 1.190614954331866791E-16 ) ) ;
#22467 = CARTESIAN_POINT ( 'NONE',  ( -23.63568631841604883, -11.45792465866591137, 73.50626392806049125 ) ) ;
#22468 = ORIENTED_EDGE ( 'NONE', *, *, #36200, .T. ) ;
#22469 = ORIENTED_EDGE ( 'NONE', *, *, #7382, .T. ) ;
#22470 = FILL_AREA_STYLE ('',( #11627 ) ) ;
#22471 = VERTEX_POINT ( 'NONE', #4439 ) ;
#22472 = EDGE_CURVE ( 'NONE', #5607, #19438, #18557, .T. ) ;
#22473 = CARTESIAN_POINT ( 'NONE',  ( -23.56007973304975422, -19.03440283107118347, 66.02400637107398040 ) ) ;
#22474 = DIRECTION ( 'NONE',  ( 0.9687793358424821033, -0.2479245821708677133, 0.000000000000000000 ) ) ;
#22475 = VECTOR ( 'NONE', #21196, 1000.000000000000000 ) ;
#22476 = CARTESIAN_POINT ( 'NONE',  ( -10.81484411697162962, -17.11524594140972155, 61.15743118925659161 ) ) ;
#22477 = CARTESIAN_POINT ( 'NONE',  ( -15.86788899160417721, -21.69347836327019863, 58.43018749706013182 ) ) ;
#22478 = ORIENTED_EDGE ( 'NONE', *, *, #19034, .T. ) ;
#22479 = FACE_OUTER_BOUND ( 'NONE', #20854, .T. ) ;
#22480 = CARTESIAN_POINT ( 'NONE',  ( -21.87646569334848579, -9.342856855644162906, 63.19713549603849145 ) ) ;
#22481 = VERTEX_POINT ( 'NONE', #15497 ) ;
#22482 = B_SPLINE_CURVE_WITH_KNOTS ( 'NONE', 3,
 ( #3811, #14601, #4301, #26460, #41228, #18826, #15599, #22781, #11682, #367 ),
 .UNSPECIFIED., .F., .F.,
 ( 4, 2, 2, 2, 4 ),
 ( 0.1272669073658803385, 0.2522669073463614797, 0.3772669073268426487, 0.5022669073073238177, 0.6272669072878049867 ),
 .UNSPECIFIED. ) ;
#22483 = CARTESIAN_POINT ( 'NONE',  ( -15.12068013687281187, -21.47611964231171200, 61.84420477127756044 ) ) ;
#22484 = CARTESIAN_POINT ( 'NONE',  ( -23.93244371613987553, -17.39065613319298009, 69.52412788448918946 ) ) ;
#22485 = VERTEX_POINT ( 'NONE', #34464 ) ;
#22486 = FACE_OUTER_BOUND ( 'NONE', #47450, .T. ) ;
#22487 = FACE_BOUND ( 'NONE', #21160, .T. ) ;
#22488 = CARTESIAN_POINT ( 'NONE',  ( -16.65185932245351452, -21.81708442718849383, 65.51092266128213737 ) ) ;
#22489 = ORIENTED_EDGE ( 'NONE', *, *, #41877, .T. ) ;
#22490 = CARTESIAN_POINT ( 'NONE',  ( -10.61330258792943226, -12.98832159324075874, 68.03832347271723791 ) ) ;
#22491 = EDGE_CURVE ( 'NONE', #38900, #9803, #29612, .T. ) ;
#22492 = CARTESIAN_POINT ( 'NONE',  ( -24.45201643071094111, -14.25170847814747255, 69.65275273439885950 ) ) ;
#22493 = CARTESIAN_POINT ( 'NONE',  ( -11.77169535943213319, -10.59578862612641714, 74.73885051658085388 ) ) ;
#22494 = CARTESIAN_POINT ( 'NONE',  ( -23.92991418586306906, -17.39300562425996333, 65.94357246486060831 ) ) ;
#22495 = VERTEX_POINT ( 'NONE', #15750 ) ;
#22496 = CARTESIAN_POINT ( 'NONE',  ( -10.61707248396235315, -11.78131495581930999, 74.60194320761131337 ) ) ;
#22497 = CARTESIAN_POINT ( 'NONE',  ( -45.92409385541305511, -17.80920654474410370, 69.24999999999998579 ) ) ;
#22498 = CARTESIAN_POINT ( 'NONE',  ( -18.50932031946840439, -21.77517977232111690, 72.43510940650374152 ) ) ;
#22499 = EDGE_CURVE ( 'NONE', #6775, #2848, #5175, .T. ) ;
#22500 = EDGE_CURVE ( 'NONE', #2504, #27510, #1702, .T. ) ;
#22501 = CARTESIAN_POINT ( 'NONE',  ( -21.39909385650551599, -8.114302828567740988, 52.18300498402516041 ) ) ;
#22503 = EDGE_CURVE ( 'NONE', #45493, #17650, #6232, .T. ) ;
#22502 = EDGE_LOOP ( 'NONE', ( #12266, #41573, #40835, #22881, #1144 ) ) ;
#22504 = CARTESIAN_POINT ( 'NONE',  ( -17.56236230286711475, -7.756850561809762290, 60.08060705895821485 ) ) ;
#22505 = CARTESIAN_POINT ( 'NONE',  ( -21.26159385759799036, -7.228003583438117552, 51.38655588711986155 ) ) ;
#22506 = ORIENTED_EDGE ( 'NONE', *, *, #25100, .T. ) ;
#22507 = CARTESIAN_POINT ( 'NONE',  ( -11.34298429649192386, -19.11328791028677898, 68.37722950534919164 ) ) ;
#22508 = EDGE_CURVE ( 'NONE', #9150, #14458, #10077, .T. ) ;
#22509 = CARTESIAN_POINT ( 'NONE',  ( -22.57893663749957369, -9.999394138389961384, 73.49633153340955971 ) ) ;
#22510 = DIRECTION ( 'NONE',  ( 3.071710424422018668E-17, -6.404604876783312462E-16, -1.000000000000000000 ) ) ;
#22511 = EDGE_LOOP ( 'NONE', ( #2652, #334, #8054, #29621, #20459 ) ) ;
#22512 = DIRECTION ( 'NONE',  ( -0.2696806815386156297, 0.9629498065864429135, 3.780696488502153947E-18 ) ) ;
#22513 = AXIS2_PLACEMENT_3D ( 'NONE', #11333, #33461, #497 ) ;
#22514 = VECTOR ( 'NONE', #21022, 1000.000000000000000 ) ;
#22515 = CARTESIAN_POINT ( 'NONE',  ( -10.70034868013728691, -12.85632356314325264, 67.84905489101299736 ) ) ;
#22516 = EDGE_CURVE ( 'NONE', #14163, #32753, #34997, .T. ) ;
#22517 = ORIENTED_EDGE ( 'NONE', *, *, #18776, .T. ) ;
#22518 = CARTESIAN_POINT ( 'NONE',  ( -13.02466918351365877, -9.790356719747981273, 49.88236859574131898 ) ) ;
#22519 = CARTESIAN_POINT ( 'NONE',  ( -18.84997077804804988, -7.496759192315632703, 70.51034705133518798 ) ) ;
#22520 = PLANE ( 'NONE',  #28480 ) ;
#22521 = CARTESIAN_POINT ( 'NONE',  ( -24.85359113602694237, -14.25571898851532460, 69.76779851910008290 ) ) ;
#22522 = CARTESIAN_POINT ( 'NONE',  ( -19.61601503992405071, -21.50980213996393786, 65.76486213821362981 ) ) ;
#22523 = ORIENTED_EDGE ( 'NONE', *, *, #39407, .F. ) ;
#22524 = EDGE_LOOP ( 'NONE', ( #23250, #30754, #15727, #36687 ) ) ;
#22525 = CARTESIAN_POINT ( 'NONE',  ( -14.90534385650551918, -8.801233750844183135, 48.81488406609782515 ) ) ;
#22526 = CARTESIAN_POINT ( 'NONE',  ( -23.00442008925062254, -19.11762375203660724, 59.18410642057862248 ) ) ;
#22527 = CARTESIAN_POINT ( 'NONE',  ( -19.30272045617997634, -8.014115550771091279, 59.96092997145631642 ) ) ;
#22528 =( BOUNDED_CURVE ( )  B_SPLINE_CURVE ( 3, ( #101, #29637, #11406, #22493 ),
 .UNSPECIFIED., .F., .F. ) 
 B_SPLINE_CURVE_WITH_KNOTS ( ( 4, 4 ),
 ( 0.5000000000000000000, 0.9074455897393649551 ),
 .UNSPECIFIED. ) 
 CURVE ( )  GEOMETRIC_REPRESENTATION_ITEM ( )  RATIONAL_B_SPLINE_CURVE ( ( 1.000000000000030198, 0.4567392136813385184, 0.3561768502900115041, 0.6983129098260819623 ) ) 
 REPRESENTATION_ITEM ( '' )  );
#22529 = CARTESIAN_POINT ( 'NONE',  ( -15.24284385650551776, -8.811426318492348031, 52.18089403414752070 ) ) ;
#22530 = ORIENTED_EDGE ( 'NONE', *, *, #24474, .F. ) ;
#22531 = CARTESIAN_POINT ( 'NONE',  ( -16.71219879347879100, -22.22520166962337740, 68.81065243885818461 ) ) ;
#22532 = CARTESIAN_POINT ( 'NONE',  ( -15.55171133418867235, -7.598245370416885969, 70.79485226425863686 ) ) ;
#22533 = FACE_OUTER_BOUND ( 'NONE', #34411, .T. ) ;
#22534 = ADVANCED_FACE ( 'NONE', ( #43078 ), #32000, .T. ) ;
#22535 = EDGE_LOOP ( 'NONE', ( #222, #31664, #44503, #6678 ) ) ;
#22536 = CARTESIAN_POINT ( 'NONE',  ( -14.83274962301728195, -7.824406256316001951, 56.99999999999994316 ) ) ;
#22537 =( BOUNDED_CURVE ( )  B_SPLINE_CURVE ( 3, ( #40196, #6469, #28629, #13583 ),
 .UNSPECIFIED., .F., .F. ) 
 B_SPLINE_CURVE_WITH_KNOTS ( ( 4, 4 ),
 ( 0.4074455897393632342, 0.5000000000000000000 ),
 .UNSPECIFIED. ) 
 CURVE ( )  GEOMETRIC_REPRESENTATION_ITEM ( )  RATIONAL_B_SPLINE_CURVE ( ( 0.6983129098260907330, 0.7760317562606838804, 0.8765941196519834167, 0.9999999999999804601 ) ) 
 REPRESENTATION_ITEM ( '' )  );
#22538 = VECTOR ( 'NONE', #24668, 1000.000000000000000 ) ;
#22539 = AXIS2_PLACEMENT_3D ( 'NONE', #736, #37908, #4194 ) ;
#22540 = ORIENTED_EDGE ( 'NONE', *, *, #41920, .T. ) ;
#22541 = CARTESIAN_POINT ( 'NONE',  ( -12.59071586039360113, -9.139687517221355861, 74.48069540779324882 ) ) ;
#22542 = CARTESIAN_POINT ( 'NONE',  ( -18.30726797983150789, -21.75326897020822514, 68.81514702557041119 ) ) ;
#22543 = CARTESIAN_POINT ( 'NONE',  ( -24.42397805733578409, -17.36001670251561890, 69.57373184374615960 ) ) ;
#22544 = CARTESIAN_POINT ( 'NONE',  ( -17.18034385541238507, -9.360768649643061323, 51.01397948905569990 ) ) ;
#22545 = EDGE_CURVE ( 'NONE', #25448, #38352, #9206, .T. ) ;
#22546 = ORIENTED_EDGE ( 'NONE', *, *, #42961, .F. ) ;
#22547 = CARTESIAN_POINT ( 'NONE',  ( -10.37871274698333046, -17.23124524545501046, 61.41389037703014964 ) ) ;
#22548 = CARTESIAN_POINT ( 'NONE',  ( -15.34960817952164192, -21.96456228242026754, 72.24586663247542617 ) ) ;
#22549 = VECTOR ( 'NONE', #39099, 1000.000000000000000 ) ;
#22550 = CARTESIAN_POINT ( 'NONE',  ( -12.20124559944014564, -19.54486383628789170, 57.93242146526704062 ) ) ;
#22551 = CARTESIAN_POINT ( 'NONE',  ( -10.08493034298069269, -16.08955231886988813, 68.17779037433831490 ) ) ;
#22552 = ORIENTED_EDGE ( 'NONE', *, *, #28294, .F. ) ;
#22553 = CARTESIAN_POINT ( 'NONE',  ( -15.04196850781542771, -10.13074752191075234, 50.77966884056655772 ) ) ;
#22554 = DIRECTION ( 'NONE',  ( -0.9243256318339804212, 0.3816046728418208134, -8.614662759602032238E-09 ) ) ;
#22555 = CARTESIAN_POINT ( 'NONE',  ( -18.52460027084869765, -7.842592186127370191, 70.25579138408188840 ) ) ;
#22556 = DIRECTION ( 'NONE',  ( -0.6562885720885137664, 0.7545099801500437797, 1.193821363054684963E-08 ) ) ;
#22557 = VERTEX_POINT ( 'NONE', #2198 ) ;
#22558 = CARTESIAN_POINT ( 'NONE',  ( -13.11988144144721780, -20.89017172700268787, 58.16933213661681634 ) ) ;
#22559 = LINE ( 'NONE', #2088, #15288 ) ;
#22560 = CARTESIAN_POINT ( 'NONE',  ( -36.42409385541304800, -6.859212275519750435, 50.50378509014258555 ) ) ;
#22561 = EDGE_CURVE ( 'NONE', #45017, #24736, #36640, .T. ) ;
#22562 = CYLINDRICAL_SURFACE ( 'NONE', #15646, 1.999999999999999556 ) ;
#22563 = VERTEX_POINT ( 'NONE', #9115 ) ;
#22564 = DIRECTION ( 'NONE',  ( 1.000000000000000000, 0.000000000000000000, 0.000000000000000000 ) ) ;
#22565 = EDGE_CURVE ( 'NONE', #32730, #31348, #1511, .T. ) ;
#22566 = ORIENTED_EDGE ( 'NONE', *, *, #33248, .T. ) ;
#22567 = CARTESIAN_POINT ( 'NONE',  ( -20.21038821853196055, -19.56678358210140800, 53.69233794759168887 ) ) ;
#22568 = CARTESIAN_POINT ( 'NONE',  ( -14.93677222777187197, -21.83177888374075692, 65.21322516587865437 ) ) ;
#22569 = VERTEX_POINT ( 'NONE', #32483 ) ;
#22570 = DIRECTION ( 'NONE',  ( -0.8743548079231423520, -0.4852872034802501178, 5.778319183281970132E-08 ) ) ;
#22571 = EDGE_CURVE ( 'NONE', #13964, #2446, #47402, .T. ) ;
#22572 = CARTESIAN_POINT ( 'NONE',  ( -13.53742098904418079, -20.63104252237469538, 58.23753158413811803 ) ) ;
#22573 = ORIENTED_EDGE ( 'NONE', *, *, #35108, .F. ) ;
#22574 = VERTEX_POINT ( 'NONE', #10561 ) ;
#22575 = ORIENTED_EDGE ( 'NONE', *, *, #42706, .T. ) ;
#22576 = CARTESIAN_POINT ( 'NONE',  ( -45.92409385541305511, -15.81020654474410847, 70.50000000000000000 ) ) ;
#22577 = CARTESIAN_POINT ( 'NONE',  ( -20.31413516131974362, -8.378470924821744603, 67.06632013881642251 ) ) ;
#22578 = DIRECTION ( 'NONE',  ( -3.071710424422018668E-17, 6.404604876783312462E-16, 1.000000000000000000 ) ) ;
#22580 = ADVANCED_FACE ( 'NONE', ( #44076 ), #33669, .T. ) ;
#22579 = FACE_OUTER_BOUND ( 'NONE', #15130, .T. ) ;
#22581 = CARTESIAN_POINT ( 'NONE',  ( -21.89264518680100835, -20.26253109894388160, 58.77915004610761684 ) ) ;
#22582 = CARTESIAN_POINT ( 'NONE',  ( -14.36038767613011302, -18.37140530287405582, 49.52966884056656482 ) ) ;
#22583 = CARTESIAN_POINT ( 'NONE',  ( -12.55596561939055000, -20.44876490328156393, 71.99927837297406086 ) ) ;
#22584 = AXIS2_PLACEMENT_3D ( 'NONE', #13290, #35226, #28084 ) ;
#22585 = AXIS2_PLACEMENT_3D ( 'NONE', #3082, #29198, #44237 ) ;
#22586 = ORIENTED_EDGE ( 'NONE', *, *, #25817, .T. ) ;
#22587 = ORIENTED_EDGE ( 'NONE', *, *, #47945, .T. ) ;
#22588 = CARTESIAN_POINT ( 'NONE',  ( -12.18170095131842068, -10.17053037870675780, 64.02914326641410980 ) ) ;
#22589 = CARTESIAN_POINT ( 'NONE',  ( -11.82099675438171005, -9.899106633794131582, 64.21409753874590365 ) ) ;
#22590 = DIRECTION ( 'NONE',  ( -6.885933442982639089E-06, 1.077603661691792080E-05, -0.9999999999182304089 ) ) ;
#22591 = CIRCLE ( 'NONE', #33560, 2.000000000000000888 ) ;
#22592 = CARTESIAN_POINT ( 'NONE',  ( 10.57590614458695377, 0.6667653706753807752, 50.27657325150214973 ) ) ;
#22593 = ORIENTED_EDGE ( 'NONE', *, *, #18456, .F. ) ;
#22594 = CARTESIAN_POINT ( 'NONE',  ( -15.43659385650551741, -6.915538690918075382, 49.31353937987644542 ) ) ;
#22595 = ORIENTED_EDGE ( 'NONE', *, *, #6646, .T. ) ;
#22596 = PLANE ( 'NONE',  #15421 ) ;
#22597 = DIRECTION ( 'NONE',  ( -0.5540494244615012942, 0.8324837747691419265, -8.494877338007846103E-17 ) ) ;
#22598 = CARTESIAN_POINT ( 'NONE',  ( -10.42302287260171312, -13.97751933429587012, 57.73352905910142852 ) ) ;
#22599 = B_SPLINE_CURVE_WITH_KNOTS ( 'NONE', 3,
 ( #18005, #48065, #30099, #15281, #36960, #30347, #37444, #33259, #15038, #18496 ),
 .UNSPECIFIED., .F., .F.,
 ( 4, 2, 2, 2, 4 ),
 ( 0.000000000000000000, 0.2500000000000000000, 0.5000000000000000000, 0.7500000000000000000, 1.000000000000000000 ),
 .UNSPECIFIED. ) ;
#22600 = EDGE_CURVE ( 'NONE', #23164, #8867, #37366, .T. ) ;
#22601 = ORIENTED_EDGE ( 'NONE', *, *, #8216, .F. ) ;
#22602 = CARTESIAN_POINT ( 'NONE',  ( 23.62590614458706639, 1.890747609047893185, 50.53028072113869484 ) ) ;
#22603 = CARTESIAN_POINT ( 'NONE',  ( -10.39215589072981416, -14.30487699944780289, 64.68803863382906627 ) ) ;
#22604 = CARTESIAN_POINT ( 'NONE',  ( -21.53338499259908545, -20.54219595513480101, 72.73266144511720199 ) ) ;
#22605 = EDGE_LOOP ( 'NONE', ( #3197, #42770, #35105, #39748 ) ) ;
#22606 = CARTESIAN_POINT ( 'NONE',  ( -24.22092373047179237, -12.93688097883364208, 66.30246741375938768 ) ) ;
#22607 = B_SPLINE_CURVE_WITH_KNOTS ( 'NONE', 3,
 ( #13284, #35221, #28338, #9383, #1496, #43364, #24403, #5450, #9636, #24651 ),
 .UNSPECIFIED., .F., .F.,
 ( 4, 2, 2, 2, 4 ),
 ( 0.1272669073658181105, 0.2522669073463079670, 0.3772669073267977957, 0.5022669073072876245, 0.6272669072877774532 ),
 .UNSPECIFIED. ) ;
#22608 = FACE_OUTER_BOUND ( 'NONE', #16681, .T. ) ;
#22609 = DIRECTION ( 'NONE',  ( -0.05957303659011965041, -0.9982239494779875377, 2.515684304538401650E-08 ) ) ;
#22610 = ORIENTED_EDGE ( 'NONE', *, *, #41940, .T. ) ;
#22611 = CARTESIAN_POINT ( 'NONE',  ( -13.86189509728330904, -11.74550036546146004, 49.52966884056655772 ) ) ;
#22612 = VECTOR ( 'NONE', #30535, 999.9999999999998863 ) ;
#22613 = AXIS2_PLACEMENT_3D ( 'NONE', #11287, #41078, #26299 ) ;
#22614 = ORIENTED_EDGE ( 'NONE', *, *, #37210, .F. ) ;
#22615 = CARTESIAN_POINT ( 'NONE',  ( -10.31624708743292018, -17.04119049769829886, 57.88098858207660413 ) ) ;
#22616 = CARTESIAN_POINT ( 'NONE',  ( -19.17247849636888901, -7.567181371456696226, 63.61584626116109575 ) ) ;
#22617 = B_SPLINE_CURVE_WITH_KNOTS ( 'NONE', 3,
 ( #5655, #19696, #16706, #4928, #23644, #24610, #20170, #27801, #8864, #20666 ),
 .UNSPECIFIED., .F., .F.,
 ( 4, 2, 2, 2, 4 ),
 ( 0.1272669073658166949, 0.2522669073463078560, 0.3772669073267990725, 0.5022669073072902890, 0.6272669072877814500 ),
 .UNSPECIFIED. ) ;
#22618 = VERTEX_POINT ( 'NONE', #44541 ) ;
#22619 = CARTESIAN_POINT ( 'NONE',  ( -17.42409385541299471, -14.80920654474435771, 49.52966884056655772 ) ) ;
#22620 = CARTESIAN_POINT ( 'NONE',  ( -24.53826898343381302, -12.59737971884151975, 69.81597065678789704 ) ) ;
#22621 = CARTESIAN_POINT ( 'NONE',  ( -20.54979551517892489, -8.489990701729437816, 63.31121512946744190 ) ) ;
#22622 = EDGE_CURVE ( 'NONE', #44379, #14, #5453, .T. ) ;
#22623 = ORIENTED_EDGE ( 'NONE', *, *, #43989, .T. ) ;
#22624 = CARTESIAN_POINT ( 'NONE',  ( -17.89813664734472098, -21.84329158499116375, 61.87535928523301720 ) ) ;
#22625 = SHAPE_REPRESENTATION ( 'Pin Studded Brass Music Cylinder', ( #29031 ), #47881 ) ;
#22626 = CARTESIAN_POINT ( 'NONE',  ( -10.67159949484657488, -12.77026894434614590, 67.83012539855924672 ) ) ;
#22627 = DIRECTION ( 'NONE',  ( -7.404863043337546774E-06, 6.320720317253164815E-06, -0.9999999999526082428 ) ) ;
#22628 = ORIENTED_EDGE ( 'NONE', *, *, #27547, .T. ) ;
#22629 = CARTESIAN_POINT ( 'NONE',  ( -19.13761704877036962, -8.022058368695287101, 63.73089277027707311 ) ) ;
#22630 = AXIS2_PLACEMENT_3D ( 'NONE', #37999, #16558, #45667 ) ;
#22631 = ADVANCED_FACE ( 'NONE', ( #29510 ), #40834, .T. ) ;
#22632 = CARTESIAN_POINT ( 'NONE',  ( -21.78215779604922275, -8.766813257424896477, 70.32470860997653972 ) ) ;
#22633 = DIRECTION ( 'NONE',  ( -3.071710424422018668E-17, 6.404604876783312462E-16, 1.000000000000000000 ) ) ;
#22634 = VERTEX_POINT ( 'NONE', #6864 ) ;
#22635 = ORIENTED_EDGE ( 'NONE', *, *, #538, .F. ) ;
#22636 = CARTESIAN_POINT ( 'NONE',  ( -22.86572475812252847, -14.01004878893095196, 54.07175714974878389 ) ) ;
#22637 = CARTESIAN_POINT ( 'NONE',  ( -10.72456167543150229, -11.55053214535348616, 71.18886621469862064 ) ) ;
#22638 = CARTESIAN_POINT ( 'NONE',  ( -23.16117746674104438, -18.90708040007733359, 62.63934749780565880 ) ) ;
#22639 = EDGE_CURVE ( 'NONE', #16518, #31075, #28554, .T. ) ;
#22640 = CARTESIAN_POINT ( 'NONE',  ( -13.66784385759799392, -9.357632978295830739, 49.97845033065684106 ) ) ;
#22641 = CARTESIAN_POINT ( 'NONE',  ( -20.31649760022732565, -7.943510736669368910, 70.43595667626200907 ) ) ;
#22642 = CARTESIAN_POINT ( 'NONE',  ( -11.85162103594838001, -10.49015045520576983, 71.25420998615621215 ) ) ;
#22643 = DIRECTION ( 'NONE',  ( 0.000000000000000000, -0.9999954153791273948, -0.003028072113819838245 ) ) ;
#22644 = CARTESIAN_POINT ( 'NONE',  ( -17.19980212172655953, -7.762775302065858085, 70.79035839668003405 ) ) ;
#22645 = VERTEX_POINT ( 'NONE', #40352 ) ;
#22646 = DIRECTION ( 'NONE',  ( -0.1240347345892086200, 1.145860353393066553E-16, -0.9922778767136676281 ) ) ;
#22647 = VECTOR ( 'NONE', #19776, 1000.000000000000000 ) ;
#22648 = CARTESIAN_POINT ( 'NONE',  ( -17.00410561000564513, -7.771727611841389383, 74.26018273220857679 ) ) ;
#22649 = CARTESIAN_POINT ( 'NONE',  ( -12.77013062424865630, -8.927826924028671840, 53.49999999999994316 ) ) ;
#22650 = EDGE_CURVE ( 'NONE', #2641, #41338, #42702, .T. ) ;
#22651 = AXIS2_PLACEMENT_3D ( 'NONE', #6075, #21105, #3352 ) ;
#22652 = EDGE_LOOP ( 'NONE', ( #14524, #31533, #43482, #3504, #30243 ) ) ;
#22653 = EDGE_CURVE ( 'NONE', #6432, #32748, #10327, .T. ) ;
#22654 = ORIENTED_EDGE ( 'NONE', *, *, #33042, .T. ) ;
#22655 = EDGE_CURVE ( 'NONE', #21712, #4554, #7472, .T. ) ;
#22656 = DIRECTION ( 'NONE',  ( -3.071710424422018668E-17, 6.404604876783312462E-16, 1.000000000000000000 ) ) ;
#22657 = LINE ( 'NONE', #10, #46522 ) ;
#22658 = CARTESIAN_POINT ( 'NONE',  ( -11.67765893934995169, -10.06753235597849461, 67.63750359946666890 ) ) ;
#22659 = CARTESIAN_POINT ( 'NONE',  ( -13.81847227395522992, -21.32875440241131670, 72.06574357974443501 ) ) ;
#22660 = CIRCLE ( 'NONE', #1417, 3.999999999999996447 ) ;
#22661 = ORIENTED_EDGE ( 'NONE', *, *, #7182, .T. ) ;
#22662 = AXIS2_PLACEMENT_3D ( 'NONE', #48150, #47194, #21803 ) ;
#22663 = CARTESIAN_POINT ( 'NONE',  ( -13.76849323099554567, -20.83774554052356009, 65.27156739751333703 ) ) ;
#22664 = CARTESIAN_POINT ( 'NONE',  ( -14.12328906776938631, -8.570644558479624919, 67.41542347112275024 ) ) ;
#22665 = VERTEX_POINT ( 'NONE', #36629 ) ;
#22666 = CARTESIAN_POINT ( 'NONE',  ( -20.57278697373333998, -8.057206101692887756, 66.89608655064280640 ) ) ;
#22667 = CARTESIAN_POINT ( 'NONE',  ( -46.47622156840087371, -14.20920654474410760, 70.13000000000000966 ) ) ;
#22668 =( BOUNDED_SURFACE ( )  B_SPLINE_SURFACE ( 3, 1, ( 
 ( #11412, #41447 ),
 ( #344, #15331 ),
 ( #30390, #25466 ),
 ( #40476, #36757 ),
 ( #18058, #48113 ),
 ( #14344, #44437 ),
 ( #6995, #10686 ) ),
 .UNSPECIFIED., .T., .F., .F. ) 
 B_SPLINE_SURFACE_WITH_KNOTS ( ( 4, 3, 4 ),
 ( 2, 2 ),
 ( 0.000000000000000000, 0.5000000000000000000, 1.000000000000000000 ),
 ( 0.000000000000000000, 1.000000000000000000 ),
 .UNSPECIFIED. ) 
 GEOMETRIC_REPRESENTATION_ITEM ( )  RATIONAL_B_SPLINE_SURFACE ( (
 ( 1.000000000000000000, 1.000000000000000000),
 ( 0.3333333333333335369, 0.3333333333333330373),
 ( 0.3333333333333335369, 0.3333333333333330373),
 ( 1.000000000000000000, 1.000000000000000000),
 ( 0.3333333333333333703, 0.3333333333333333703),
 ( 0.3333333333333333703, 0.3333333333333333703),
 ( 1.000000000000000000, 1.000000000000000000) ) ) 
 REPRESENTATION_ITEM ( '' )  SURFACE ( )  );
#22669 = CARTESIAN_POINT ( 'NONE',  ( -14.75738004989435481, -8.279008875931440414, 56.85000000000044196 ) ) ;
#22670 = ORIENTED_EDGE ( 'NONE', *, *, #25170, .F. ) ;
#22671 = CARTESIAN_POINT ( 'NONE',  ( -17.47591198265878631, -7.808960448257721509, 67.30422983416791283 ) ) ;
#22672 = ORIENTED_EDGE ( 'NONE', *, *, #14731, .F. ) ;
#22673 = CARTESIAN_POINT ( 'NONE',  ( -22.83095763869631512, -19.93459457198476770, 72.82895875648904394 ) ) ;
#22674 = CARTESIAN_POINT ( 'NONE',  ( -11.28158159523816728, -11.33292898549803240, 57.36470039992773451 ) ) ;
#22675 = ORIENTED_EDGE ( 'NONE', *, *, #38036, .T. ) ;
#22676 = FACE_OUTER_BOUND ( 'NONE', #474, .T. ) ;
#22677 = CARTESIAN_POINT ( 'NONE',  ( -20.10030204730919223, -21.76202525863913451, 72.51983304728076973 ) ) ;
#22678 = CARTESIAN_POINT ( 'NONE',  ( -19.46159385650551599, -9.295667164867525756, 49.30633214617472504 ) ) ;
#22679 = CIRCLE ( 'NONE', #32104, 3.951441697420869481 ) ;
#22680 = CARTESIAN_POINT ( 'NONE',  ( -10.56492523587830235, -13.18000265412059058, 71.35828586226037373 ) ) ;
#22681 = AXIS2_PLACEMENT_3D ( 'NONE', #46327, #32023, #5202 ) ;
#22682 = B_SPLINE_CURVE_WITH_KNOTS ( 'NONE', 1,
 ( #8701, #5237 ),
 .UNSPECIFIED., .F., .F.,
 ( 2, 2 ),
 ( 0.000000000000000000, 1.000000000000000000 ),
 .UNSPECIFIED. ) ;
#22683 = FACE_OUTER_BOUND ( 'NONE', #17395, .T. ) ;
#22684 = DIRECTION ( 'NONE',  ( -0.000000000000000000, -1.000000000000000000, -0.000000000000000000 ) ) ;
#22685 = CARTESIAN_POINT ( 'NONE',  ( -21.72145186077268519, -9.220171914992313589, 66.66709799741713027 ) ) ;
#22686 = ORIENTED_EDGE ( 'NONE', *, *, #4988, .T. ) ;
#22688 =( BOUNDED_CURVE ( )  B_SPLINE_CURVE ( 3, ( #8394, #45599, #26877, #19723 ),
 .UNSPECIFIED., .F., .F. ) 
 B_SPLINE_CURVE_WITH_KNOTS ( ( 4, 4 ),
 ( 0.5000000000000000000, 0.9074455897393621795 ),
 .UNSPECIFIED. ) 
 CURVE ( )  GEOMETRIC_REPRESENTATION_ITEM ( )  RATIONAL_B_SPLINE_CURVE ( ( 0.9999999999999794609, 0.4567392136813308579, 0.3561768502900442002, 0.6983129098260970613 ) ) 
 REPRESENTATION_ITEM ( '' )  );
#22687 = CARTESIAN_POINT ( 'NONE',  ( -10.43358824505211224, -14.44357141193983374, 64.61477203541403469 ) ) ;
#22689 = VECTOR ( 'NONE', #25473, 1000.000000000000114 ) ;
#22690 = AXIS2_PLACEMENT_3D ( 'NONE', #8103, #30514, #7370 ) ;
#22691 = LINE ( 'NONE', #25406, #42375 ) ;
#22692 = CYLINDRICAL_SURFACE ( 'NONE', #25112, 4.686499999999997002 ) ;
#22693 = CARTESIAN_POINT ( 'NONE',  ( -22.38971998310932676, -20.36320860488637763, 62.41156058973809451 ) ) ;
#22694 = EDGE_CURVE ( 'NONE', #43000, #43727, #45996, .T. ) ;
#22695 = CARTESIAN_POINT ( 'NONE',  ( -12.01648201532752935, -10.28590752825076926, 67.64896869922044687 ) ) ;
#22696 = B_SPLINE_CURVE_WITH_KNOTS ( 'NONE', 1,
 ( #45856, #8669 ),
 .UNSPECIFIED., .F., .F.,
 ( 2, 2 ),
 ( 0.000000000000000000, 1.000000000000000000 ),
 .UNSPECIFIED. ) ;
#22697 = CARTESIAN_POINT ( 'NONE',  ( -16.00544582274271477, -7.903112417841744453, 63.95538887075813506 ) ) ;
#22698 = ORIENTED_EDGE ( 'NONE', *, *, #18715, .F. ) ;
#22699 = ORIENTED_EDGE ( 'NONE', *, *, #46810, .F. ) ;
#22700 = B_SPLINE_CURVE_WITH_KNOTS ( 'NONE', 3,
 ( #15833, #30882, #45895, #12155, #27173, #42195, #38485, #4770, #31109, #34798 ),
 .UNSPECIFIED., .F., .F.,
 ( 4, 2, 2, 2, 4 ),
 ( 0.6272669072877545826, 0.7522669073072720813, 0.8772669073267895801, 1.002266907346307079, 1.127266907365824578 ),
 .UNSPECIFIED. ) ;
#22701 = ADVANCED_FACE ( 'NONE', ( #29276 ), #10479, .T. ) ;
#22702 = CARTESIAN_POINT ( 'NONE',  ( -11.60247201135026884, -18.79965542285971836, 61.43277710409636683 ) ) ;
#22703 = CARTESIAN_POINT ( 'NONE',  ( -14.91737466579130711, -8.273365706877857662, 56.86467890717403861 ) ) ;
#22704 = ORIENTED_EDGE ( 'NONE', *, *, #25101, .T. ) ;
#22705 = CARTESIAN_POINT ( 'NONE',  ( -20.99124470470196968, -21.34988281449478364, 62.25438046261486136 ) ) ;
#22706 = DIRECTION ( 'NONE',  ( -3.071710424422018668E-17, 6.404604876783312462E-16, 1.000000000000000000 ) ) ;
#22707 = AXIS2_PLACEMENT_3D ( 'NONE', #27025, #18643, #22355 ) ;
#22708 = CARTESIAN_POINT ( 'NONE',  ( -11.86732220369407997, -9.846751984446582284, 64.28560238571537866 ) ) ;
#22709 = CARTESIAN_POINT ( 'NONE',  ( -10.45629970556533905, -15.48118908973361485, 57.56792791464064152 ) ) ;
#22710 = CARTESIAN_POINT ( 'NONE',  ( -12.10599200002982556, -20.02663609087960239, 61.58174067880212021 ) ) ;
#22711 = DIRECTION ( 'NONE',  ( 0.9687793358424819923, -0.2479245821708678243, 0.000000000000000000 ) ) ;
#22712 =( BOUNDED_CURVE ( )  B_SPLINE_CURVE ( 3, ( #26168, #34696, #40932, #38631 ),
 .UNSPECIFIED., .F., .F. ) 
 B_SPLINE_CURVE_WITH_KNOTS ( ( 4, 4 ),
 ( 0.5000000000000000000, 0.9074455897393589598 ),
 .UNSPECIFIED. ) 
 CURVE ( )  GEOMETRIC_REPRESENTATION_ITEM ( )  RATIONAL_B_SPLINE_CURVE ( ( 0.9999999999999746869, 0.4567392136813389625, 0.3561768502900504729, 0.6983129098260817402 ) ) 
 REPRESENTATION_ITEM ( '' )  );
#22713 = LINE ( 'NONE', #37206, #25961 ) ;
#22714 = CARTESIAN_POINT ( 'NONE',  ( -10.02281612969872349, -15.66031113496680049, 61.14514897868617282 ) ) ;
#22715 = CARTESIAN_POINT ( 'NONE',  ( -24.12409162043482524, -11.55122986829102238, 63.07501371131629497 ) ) ;
#22716 = LINE ( 'NONE', #23696, #8554 ) ;
#22717 = CARTESIAN_POINT ( 'NONE',  ( -17.74207408223254845, -7.814823900609349394, 63.73984019819800295 ) ) ;
#22718 = DIRECTION ( 'NONE',  ( 0.000000000000000000, 0.000000000000000000, 1.000000000000000000 ) ) ;
#22719 = CARTESIAN_POINT ( 'NONE',  ( -23.78676244964941233, -10.93361294341921131, 73.54688584860882372 ) ) ;
#22721 = VERTEX_POINT ( 'NONE', #8573 ) ;
#22720 = ADVANCED_FACE ( 'NONE', ( #26552 ), #30263, .T. ) ;
#22722 = ORIENTED_EDGE ( 'NONE', *, *, #48107, .T. ) ;
#22723 =( LENGTH_UNIT ( ) NAMED_UNIT ( * ) SI_UNIT ( .MILLI., .METRE. ) );
#22724 = ORIENTED_EDGE ( 'NONE', *, *, #8186, .F. ) ;
#22725 = B_SPLINE_CURVE_WITH_KNOTS ( 'NONE', 3,
 ( #36934, #3218, #26611, #22422, #3457, #14504, #29563, #44594, #29326, #7668 ),
 .UNSPECIFIED., .F., .F.,
 ( 4, 2, 2, 2, 4 ),
 ( 0.6272669072877775642, 0.7522669073072877355, 0.8772669073267977957, 1.002266907346307967, 1.127266907365818138 ),
 .UNSPECIFIED. ) ;
#22726 = EDGE_CURVE ( 'NONE', #47056, #8151, #14621, .T. ) ;
#22727 = ADVANCED_FACE ( 'NONE', ( #12498 ), #38841, .F. ) ;
#22728 = EDGE_CURVE ( 'NONE', #20803, #22914, #27036, .T. ) ;
#22729 = CARTESIAN_POINT ( 'NONE',  ( -15.63659385759799036, -8.995762431863214559, 51.38120296130585274 ) ) ;
#22730 = AXIS2_PLACEMENT_3D ( 'NONE', #26875, #33990, #517 ) ;
#22731 = CARTESIAN_POINT ( 'NONE',  ( -17.52853272358826686, -7.759682304905023642, 63.83584969886392457 ) ) ;
#22732 = VECTOR ( 'NONE', #44173, 1000.000000000000000 ) ;
#22733 = VECTOR ( 'NONE', #39151, 999.9999999999998863 ) ;
#22734 = CIRCLE ( 'NONE', #43973, 2.000000000000000888 ) ;
#22735 = CARTESIAN_POINT ( 'NONE',  ( -11.28351140919878759, -11.44840856261519768, 64.14882000273821916 ) ) ;
#22736 = CARTESIAN_POINT ( 'NONE',  ( -16.08586241947643458, -22.13815726599775857, 58.40868711133772706 ) ) ;
#22737 = ORIENTED_EDGE ( 'NONE', *, *, #30824, .T. ) ;
#22738 = CARTESIAN_POINT ( 'NONE',  ( -13.53844544295976249, -20.69534049476535031, 65.40117765236396963 ) ) ;
#22739 = CARTESIAN_POINT ( 'NONE',  ( -17.59054788464097996, -7.361056023586105113, 63.65033409075859794 ) ) ;
#22740 = B_SPLINE_CURVE_WITH_KNOTS ( 'NONE', 3,
 ( #47007, #18100, #48157, #13254, #43333, #9604, #24618, #39621, #13503, #32246 ),
 .UNSPECIFIED., .F., .F.,
 ( 4, 2, 2, 2, 4 ),
 ( 0.6272669072877842256, 0.7522669073072956181, 0.8772669073268071216, 1.002266907346318625, 1.127266907365829907 ),
 .UNSPECIFIED. ) ;
#22741 = ORIENTED_EDGE ( 'NONE', *, *, #39858, .F. ) ;
#22742 = DIRECTION ( 'NONE',  ( 0.4780674886490096642, -0.8783231047267436864, -5.292596398047473452E-08 ) ) ;
#22743 = CARTESIAN_POINT ( 'NONE',  ( -12.25434508901797770, -20.17367074759813406, 65.05170324716399932 ) ) ;
#22744 = ORIENTED_EDGE ( 'NONE', *, *, #36988, .F. ) ;
#22745 = DIRECTION ( 'NONE',  ( -3.071710424422018668E-17, 6.404604876783312462E-16, 1.000000000000000000 ) ) ;
#22746 = CARTESIAN_POINT ( 'NONE',  ( -11.04141237841800560, -11.93494539390495568, 74.85840195306853673 ) ) ;
#22747 = CARTESIAN_POINT ( 'NONE',  ( -17.19740490131689015, -7.362649021479085398, 70.69047035906775989 ) ) ;
#22748 = ORIENTED_EDGE ( 'NONE', *, *, #26947, .T. ) ;
#22749 = CARTESIAN_POINT ( 'NONE',  ( -12.79725838692604434, -20.12850099319811292, 71.80653676770127447 ) ) ;
#22750 = EDGE_CURVE ( 'NONE', #27898, #23048, #16776, .T. ) ;
#22751 = DIRECTION ( 'NONE',  ( -3.071710424422018668E-17, 6.404604876783312462E-16, 1.000000000000000000 ) ) ;
#22752 = CARTESIAN_POINT ( 'NONE',  ( -24.30112618867181240, -13.25578303422174997, 59.64795780745660636 ) ) ;
#22753 = DIRECTION ( 'NONE',  ( 0.2479245821708711550, 0.9687793358424812151, 0.000000000000000000 ) ) ;
#22754 = VERTEX_POINT ( 'NONE', #4385 ) ;
#22755 = CARTESIAN_POINT ( 'NONE',  ( -24.68310392741195258, -16.48564297948346891, 59.37978378043003147 ) ) ;
#22756 = FACE_OUTER_BOUND ( 'NONE', #2884, .T. ) ;
#22757 = CARTESIAN_POINT ( 'NONE',  ( -10.43098718212803000, -15.70539730037032911, 61.32316937334011442 ) ) ;
#22758 = CARTESIAN_POINT ( 'NONE',  ( -10.38360249164154325, -14.43747963625415309, 67.87272197508832505 ) ) ;
#22759 = CARTESIAN_POINT ( 'NONE',  ( -16.80428239998583351, -12.38725820513820253, 54.27966884056655061 ) ) ;
#22760 = CARTESIAN_POINT ( 'NONE',  ( -21.06702863216100496, -20.84540773593990792, 65.86981821684420879 ) ) ;
#22761 = CARTESIAN_POINT ( 'NONE',  ( -18.92409385650551812, -6.426201560718813433, 50.50509628382439331 ) ) ;
#22762 = ORIENTED_EDGE ( 'NONE', *, *, #44562, .F. ) ;
#22763 = B_SPLINE_CURVE_WITH_KNOTS ( 'NONE', 3,
 ( #14809, #34035, #324, #12362, #30615, #1272, #23459, #4744, #15551, #7970 ),
 .UNSPECIFIED., .F., .F.,
 ( 4, 2, 2, 2, 4 ),
 ( 0.6272669072877556928, 0.7522669073072749679, 0.8772669073267943540, 1.002266907346313740, 1.127266907365833015 ),
 .UNSPECIFIED. ) ;
#22764 = EDGE_CURVE ( 'NONE', #14369, #35176, #2268, .T. ) ;
#22765 = VECTOR ( 'NONE', #19118, 1000.000000000000000 ) ;
#22766 = LINE ( 'NONE', #10689, #33736 ) ;
#22767 = DIRECTION ( 'NONE',  ( -8.262539633966638414E-06, 9.998826072665628149E-07, 0.9999999999653652605 ) ) ;
#22768 = ORIENTED_EDGE ( 'NONE', *, *, #21498, .F. ) ;
#22769 = DIRECTION ( 'NONE',  ( -5.731567514496413899E-31, -1.020425574103664789E-16, -1.000000000000000000 ) ) ;
#22770 = FACE_OUTER_BOUND ( 'NONE', #26730, .T. ) ;
#22771 = CARTESIAN_POINT ( 'NONE',  ( -19.28939461086542906, -8.062307027802660286, 60.26092997386343342 ) ) ;
#22772 = ORIENTED_EDGE ( 'NONE', *, *, #12824, .F. ) ;
#22773 = CIRCLE ( 'NONE', #15676, 1.749999999999997558 ) ;
#22774 = VECTOR ( 'NONE', #28923, 1000.000000000000000 ) ;
#22775 = CARTESIAN_POINT ( 'NONE',  ( -10.47910621644337326, -16.03883162486972935, 64.39282756246913664 ) ) ;
#22776 = DIRECTION ( 'NONE',  ( 0.06357898915123498529, -0.9979768094191904249, 0.000000000000000000 ) ) ;
#22777 = VERTEX_POINT ( 'NONE', #26806 ) ;
#22778 = CARTESIAN_POINT ( 'NONE',  ( -14.42409385650551457, -6.426201560718813433, 50.50509628382439331 ) ) ;
#22779 = AXIS2_PLACEMENT_3D ( 'NONE', #40009, #46912, #44213 ) ;
#22780 = CARTESIAN_POINT ( 'NONE',  ( -10.99668346656864060, -11.04197136062318307, 60.72239829427679325 ) ) ;
#22781 = CARTESIAN_POINT ( 'NONE',  ( -24.80433737800517591, -15.82637729575692553, 69.73296257493650785 ) ) ;
#22782 = CARTESIAN_POINT ( 'NONE',  ( -22.41759978862804914, -13.18828134753566239, 52.02966884056656482 ) ) ;
#22783 = DIRECTION ( 'NONE',  ( 1.927470528863184130E-16, 1.434740771370715221E-29, -1.000000000000000000 ) ) ;
#22784 = EDGE_LOOP ( 'NONE', ( #39289, #24666, #41640, #23776, #35886 ) ) ;
#22785 = VERTEX_POINT ( 'NONE', #35139 ) ;
#22786 = CARTESIAN_POINT ( 'NONE',  ( -14.06159385650551741, -9.295667164867525756, 49.30633214617472504 ) ) ;
#22787 = ADVANCED_FACE ( 'NONE', ( #41828 ), #30333, .T. ) ;
#22788 = EDGE_CURVE ( 'NONE', #2135, #18357, #42202, .T. ) ;
#22789 = CARTESIAN_POINT ( 'NONE',  ( -23.48344415125163565, -18.41350569598871090, 73.04896097104848707 ) ) ;
#22790 = CARTESIAN_POINT ( 'NONE',  ( -28.42409385541305511, -6.859206544744110623, 52.99999999999997158 ) ) ;
#22791 = CARTESIAN_POINT ( 'NONE',  ( -15.80534385650551421, -8.801233750844183135, 48.81488406609782515 ) ) ;
#22792 = EDGE_CURVE ( 'NONE', #25029, #17957, #12744, .T. ) ;
#22793 = EDGE_CURVE ( 'NONE', #6378, #4829, #20358, .T. ) ;
#22794 = CARTESIAN_POINT ( 'NONE',  ( -16.06904075904983031, -7.890656793283918446, 63.97011029956862416 ) ) ;
#22795 = CARTESIAN_POINT ( 'NONE',  ( -10.23610939720467528, -12.85046776639672039, 67.85337053980535416 ) ) ;
#22796 = ADVANCED_FACE ( 'NONE', ( #46492 ), #27996, .T. ) ;
#22797 = DIRECTION ( 'NONE',  ( -1.000000000000000000, 3.159776991290051445E-16, -3.534154189880001717E-15 ) ) ;
#22798 = CARTESIAN_POINT ( 'NONE',  ( -11.46043946983621709, -11.04924301243271678, 57.35903212150709152 ) ) ;
#22799 = ORIENTED_EDGE ( 'NONE', *, *, #19280, .T. ) ;
#22800 = DIRECTION ( 'NONE',  ( -0.9997277805376393323, 0.02333162706040292633, 9.101776391673754705E-09 ) ) ;
#22801 = AXIS2_PLACEMENT_3D ( 'NONE', #3936, #18942, #41107 ) ;
#22802 = VERTEX_POINT ( 'NONE', #12969 ) ;
#22803 = CARTESIAN_POINT ( 'NONE',  ( -14.44809130310161471, -8.473323905341505480, 67.25975083863336579 ) ) ;
#22804 = CARTESIAN_POINT ( 'NONE',  ( -13.62243047842596866, -8.871999776185514719, 56.96967785305174203 ) ) ;
#22805 = DIRECTION ( 'NONE',  ( 1.927470528863119542E-16, 0.000000000000000000, -1.000000000000000000 ) ) ;
#22806 = DIRECTION ( 'NONE',  ( 5.551115123125782702E-17, 1.232595164407830946E-32, 1.000000000000000000 ) ) ;
#22807 = ADVANCED_FACE ( 'NONE', ( #2384 ), #1661, .F. ) ;
#22808 = ORIENTED_EDGE ( 'NONE', *, *, #28736, .T. ) ;
#22809 = CARTESIAN_POINT ( 'NONE',  ( -17.98584054083101691, -22.23808389992613499, 62.06031238270200845 ) ) ;
#22810 = AXIS2_PLACEMENT_3D ( 'NONE', #11777, #22872, #25810 ) ;
#22811 = CARTESIAN_POINT ( 'NONE',  ( -22.79909142865265537, -19.96788931561671276, 72.84411743013269813 ) ) ;
#22812 = CARTESIAN_POINT ( 'NONE',  ( -13.06813783877040791, -9.265530354883376063, 67.66470656304637998 ) ) ;
#22813 = FACE_OUTER_BOUND ( 'NONE', #11435, .T. ) ;
#22814 = EDGE_LOOP ( 'NONE', ( #9707, #39915, #9730, #8036 ) ) ;
#22815 = CARTESIAN_POINT ( 'NONE',  ( -23.12302852889638061, -18.95946475466559633, 62.65406880579606508 ) ) ;
#22816 = CARTESIAN_POINT ( 'NONE',  ( -18.57335281209669375, -21.76520412651811043, 72.57038810541313012 ) ) ;
#22817 = DIRECTION ( 'NONE',  ( 3.071710424422018668E-17, -6.404604876783312462E-16, -1.000000000000000000 ) ) ;
#22818 = FACE_BOUND ( 'NONE', #31512, .T. ) ;
#22819 = ITEM_DEFINED_TRANSFORMATION ( 'NONE', 'NONE', #20408,  #29031 ) ;
#22820 = ORIENTED_EDGE ( 'NONE', *, *, #41809, .F. ) ;
#22821 = DIRECTION ( 'NONE',  ( -3.071710424422018668E-17, 6.404604876783312462E-16, 1.000000000000000000 ) ) ;
#22822 = AXIS2_PLACEMENT_3D ( 'NONE', #23850, #17815, #47878 ) ;
#22823 = CARTESIAN_POINT ( 'NONE',  ( -10.55151208239364635, -17.68521041179895548, 68.28217381303441869 ) ) ;
#22824 = DIRECTION ( 'NONE',  ( 0.9687793358424819923, -0.2479245821708680464, 0.000000000000000000 ) ) ;
#22825 = EDGE_LOOP ( 'NONE', ( #9547, #44011, #22834, #37858, #34799 ) ) ;
#22826 = CARTESIAN_POINT ( 'NONE',  ( -10.44202790750644461, -14.30845231023897846, 64.38803863533676974 ) ) ;
#22827 = ORIENTED_EDGE ( 'NONE', *, *, #31030, .F. ) ;
#22828 = CARTESIAN_POINT ( 'NONE',  ( -12.28110106126006507, -10.05819346760517341, 64.13987352327488622 ) ) ;
#22829 = CARTESIAN_POINT ( 'NONE',  ( -17.40545348791034286, -7.756229321676927135, 70.90524440011041918 ) ) ;
#22830 = LINE ( 'NONE', #3607, #9399 ) ;
#22831 = ORIENTED_EDGE ( 'NONE', *, *, #27670, .F. ) ;
#22832 = CARTESIAN_POINT ( 'NONE',  ( -10.98345768875619832, -17.55129762975471408, 68.38256636668904775 ) ) ;
#22833 = ORIENTED_EDGE ( 'NONE', *, *, #20870, .T. ) ;
#22834 = ORIENTED_EDGE ( 'NONE', *, *, #21080, .F. ) ;
#22835 = ORIENTED_EDGE ( 'NONE', *, *, #11805, .F. ) ;
#22836 = CARTESIAN_POINT ( 'NONE',  ( -15.46105799208929454, -21.99670631207736449, 72.15920124769014876 ) ) ;
#22837 = VECTOR ( 'NONE', #3401, 1000.000000000000000 ) ;
#22838 = VECTOR ( 'NONE', #23165, 1000.000000000000000 ) ;
#22839 = CARTESIAN_POINT ( 'NONE',  ( -24.82750195234013191, -13.97654432178796569, 73.30766915316792165 ) ) ;
#22840 = CARTESIAN_POINT ( 'NONE',  ( -10.03092739215081686, -13.89030502949973567, 57.64099168746837165 ) ) ;
#22841 = EDGE_CURVE ( 'NONE', #7586, #10306, #19757, .T. ) ;
#22842 =( BOUNDED_CURVE ( )  B_SPLINE_CURVE ( 3, ( #46565, #31280, #42629, #38909 ),
 .UNSPECIFIED., .F., .F. ) 
 B_SPLINE_CURVE_WITH_KNOTS ( ( 4, 4 ),
 ( 0.000000000000000000, 0.4074455897393638448 ),
 .UNSPECIFIED. ) 
 CURVE ( )  GEOMETRIC_REPRESENTATION_ITEM ( )  RATIONAL_B_SPLINE_CURVE ( ( 1.000000000000000000, 0.4567392136813312464, 0.3561768502900300448, 0.6983129098260963952 ) ) 
 REPRESENTATION_ITEM ( '' )  );
#22843 = DIRECTION ( 'NONE',  ( 0.000000000000000000, 0.000000000000000000, -1.000000000000000000 ) ) ;
#22844 = CARTESIAN_POINT ( 'NONE',  ( -45.92409385541306222, -14.90920654474410867, 71.75000000000001421 ) ) ;
#22845 = CARTESIAN_POINT ( 'NONE',  ( -12.50201028167747275, -20.40183342018594814, 71.92936770876625019 ) ) ;
#22846 = AXIS2_PLACEMENT_3D ( 'NONE', #3128, #2879, #47704 ) ;
#22847 = ORIENTED_EDGE ( 'NONE', *, *, #17702, .F. ) ;
#22848 = ORIENTED_EDGE ( 'NONE', *, *, #12988, .F. ) ;
#22849 = CARTESIAN_POINT ( 'NONE',  ( -24.82492784865917201, -15.66438054851105832, 73.25949685721523963 ) ) ;
#22850 = ADVANCED_FACE ( 'NONE', ( #9302 ), #47301, .T. ) ;
#22851 = DIRECTION ( 'NONE',  ( -5.255974128148611414E-06, 1.684062796621483993E-06, 0.9999999999847694054 ) ) ;
#22852 = AXIS2_PLACEMENT_3D ( 'NONE', #21265, #36721, #3010 ) ;
#22853 = CARTESIAN_POINT ( 'NONE',  ( -19.60046790782316251, -21.46228069541063732, 65.46486213989528835 ) ) ;
#22854 = EDGE_LOOP ( 'NONE', ( #3572, #894 ) ) ;
#22855 = CARTESIAN_POINT ( 'NONE',  ( -16.61784385650551954, -9.790100578890868377, 49.79778022625163203 ) ) ;
#22856 =( BOUNDED_CURVE ( )  B_SPLINE_CURVE ( 3, ( #13427, #36076, #24300, #9525 ),
 .UNSPECIFIED., .F., .F. ) 
 B_SPLINE_CURVE_WITH_KNOTS ( ( 4, 4 ),
 ( 0.9074455897393604031, 1.000000000000000000 ),
 .UNSPECIFIED. ) 
 CURVE ( )  GEOMETRIC_REPRESENTATION_ITEM ( )  RATIONAL_B_SPLINE_CURVE ( ( 0.6983129098260820733, 0.7760317562606887654, 0.8765941196519947409, 1.000000000000000000 ) ) 
 REPRESENTATION_ITEM ( '' )  );
#22858 = EDGE_LOOP ( 'NONE', ( #9232, #21766, #12970, #8471, #41805, #12092 ) ) ;
#22857 = EDGE_CURVE ( 'NONE', #43487, #43698, #39810, .T. ) ;
#22859 = DIRECTION ( 'NONE',  ( 0.9974380310868018462, 0.07153582418399356824, -3.008056593457534435E-08 ) ) ;
#22860 = CARTESIAN_POINT ( 'NONE',  ( -15.42710743425593733, -21.51837058719337037, 68.64880986307761646 ) ) ;
#22861 = ADVANCED_FACE ( 'NONE', ( #2137 ), #36102, .T. ) ;
#22862 = PLANE ( 'NONE',  #45688 ) ;
#22863 = EDGE_CURVE ( 'NONE', #1260, #48343, #43824, .T. ) ;
#22864 = VERTEX_POINT ( 'NONE', #14578 ) ;
#22865 = CARTESIAN_POINT ( 'NONE',  ( -20.32351072818673288, -7.946504961695468161, 70.44374510728370353 ) ) ;
#22866 = DIRECTION ( 'NONE',  ( -0.8447509909909768355, 0.5351595679979596065, 0.000000000000000000 ) ) ;
#22867 = DIRECTION ( 'NONE',  ( -0.7506333037770538397, 0.6607190350373941534, 0.000000000000000000 ) ) ;
#22868 = VECTOR ( 'NONE', #21940, 1000.000000000000000 ) ;
#22869 = VERTEX_POINT ( 'NONE', #41443 ) ;
#22870 = DIRECTION ( 'NONE',  ( 0.9687793358424821033, -0.2479245821708677133, 0.000000000000000000 ) ) ;
#22871 = EDGE_CURVE ( 'NONE', #32161, #34423, #41207, .T. ) ;
#22872 = DIRECTION ( 'NONE',  ( -3.071710424422018668E-17, 6.404604876783312462E-16, 1.000000000000000000 ) ) ;
#22873 = CARTESIAN_POINT ( 'NONE',  ( 23.52590614458706852, -0.009252390952106800612, 50.53028072113869484 ) ) ;
#22874 = ORIENTED_EDGE ( 'NONE', *, *, #1031, .T. ) ;
#22875 = CARTESIAN_POINT ( 'NONE',  ( -10.52210740440793124, -15.97650391503338874, 64.69874700433834391 ) ) ;
#22876 = AXIS2_PLACEMENT_3D ( 'NONE', #5648, #13231, #6109 ) ;
#22877 = ORIENTED_EDGE ( 'NONE', *, *, #2986, .F. ) ;
#22878 = DIRECTION ( 'NONE',  ( 1.000000000000000000, -4.164305804376849172E-17, 1.614929280266638808E-16 ) ) ;
#22879 = PRODUCT_DEFINITION_SHAPE ( 'NONE', 'NONE',  #42442 ) ;
#22880 = DIRECTION ( 'NONE',  ( 2.866981220435666553E-17, -1.000000000000000000, -1.190614954331866791E-16 ) ) ;
#22881 = ORIENTED_EDGE ( 'NONE', *, *, #4853, .F. ) ;
#22882 = CARTESIAN_POINT ( 'NONE',  ( -45.94606420501752098, -14.19714313411900264, 69.94185769334995939 ) ) ;
#22883 = PLANE ( 'NONE',  #25528 ) ;
#22884 = CARTESIAN_POINT ( 'NONE',  ( -18.61375994297531378, -22.16373410720964543, 72.46227804786110482 ) ) ;
#22885 = ORIENTED_EDGE ( 'NONE', *, *, #429, .T. ) ;
#22886 = CARTESIAN_POINT ( 'NONE',  ( -21.38163477318978423, -20.58317637574389991, 72.80981012061528190 ) ) ;
#22887 = PLANE ( 'NONE',  #37726 ) ;
#22888 = CARTESIAN_POINT ( 'NONE',  ( -11.43178109911094431, -11.19077805147660065, 57.28191156135590489 ) ) ;
#22889 = ORIENTED_EDGE ( 'NONE', *, *, #41035, .T. ) ;
#22890 = CARTESIAN_POINT ( 'NONE',  ( -19.09949158415725634, -8.012660229328147921, 63.43089235425713923 ) ) ;
#22891 = DIRECTION ( 'NONE',  ( 0.9687793358424821033, -0.2479245821708680464, 0.000000000000000000 ) ) ;
#22893 = ORIENTED_EDGE ( 'NONE', *, *, #38809, .T. ) ;
#22892 = AXIS2_PLACEMENT_3D ( 'NONE', #15077, #19274, #809 ) ;
#22894 = ORIENTED_EDGE ( 'NONE', *, *, #33030, .T. ) ;
#22895 = CARTESIAN_POINT ( 'NONE',  ( -22.75923595801102550, -10.27751167601812909, 66.54182257657851096 ) ) ;
#22896 = DIRECTION ( 'NONE',  ( -1.000000000000000000, -1.669677910507523057E-21, -6.493791346278465266E-22 ) ) ;
#22897 = B_SPLINE_CURVE_WITH_KNOTS ( 'NONE', 1,
 ( #37348, #3635 ),
 .UNSPECIFIED., .F., .F.,
 ( 2, 2 ),
 ( 0.000000000000000000, 1.000000000000000000 ),
 .UNSPECIFIED. ) ;
#22898 = PLANE ( 'NONE',  #37461 ) ;
#22899 = FACE_OUTER_BOUND ( 'NONE', #14294, .T. ) ;
#22900 = CARTESIAN_POINT ( 'NONE',  ( -21.96159385650551599, -9.295667164867525756, 49.30633214617472504 ) ) ;
#22901 = CARTESIAN_POINT ( 'NONE',  ( -10.42302287260171312, -13.97751933429587012, 57.73352905910142852 ) ) ;
#22902 = ADVANCED_FACE ( 'NONE', ( #4275 ), #30621, .T. ) ;
#22903 = CARTESIAN_POINT ( 'NONE',  ( -12.13611197186221524, -9.561363708614054602, 57.28946728381664855 ) ) ;
#22904 = CARTESIAN_POINT ( 'NONE',  ( -16.99405130501816075, -7.371615963843898278, 74.06044024557584748 ) ) ;
#22905 = DIRECTION ( 'NONE',  ( 0.6607190350373968180, 0.7506333037770515082, 0.000000000000000000 ) ) ;
#22906 = ORIENTED_EDGE ( 'NONE', *, *, #27691, .T. ) ;
#22908 = LINE ( 'NONE', #11558, #22612 ) ;
#22907 = VECTOR ( 'NONE', #12234, 1000.000000000000000 ) ;
#22909 = VECTOR ( 'NONE', #34120, 1000.000000000000000 ) ;
#22910 = CARTESIAN_POINT ( 'NONE',  ( -10.02813348864759035, -13.91211103331672483, 57.60858365818264559 ) ) ;
#22911 = CARTESIAN_POINT ( 'NONE',  ( -23.88415222675040184, -17.63235122089636775, 62.47360984996718258 ) ) ;
#22912 = AXIS2_PLACEMENT_3D ( 'NONE', #12420, #16591, #23768 ) ;
#22913 = EDGE_LOOP ( 'NONE', ( #36399, #34993, #2382, #32509, #7782 ) ) ;
#22914 = VERTEX_POINT ( 'NONE', #19046 ) ;
#22915 = CARTESIAN_POINT ( 'NONE',  ( -19.89647106316203562, -21.35805615853005435, 69.18000941309762197 ) ) ;
#22916 = ADVANCED_FACE ( 'NONE', ( #17629 ), #3560, .T. ) ;
#22917 = CARTESIAN_POINT ( 'NONE',  ( -22.83095840648717711, -19.93459376977450859, 72.82895984417613988 ) ) ;
#22918 = PLANE ( 'NONE',  #506 ) ;
#22919 = EDGE_CURVE ( 'NONE', #7972, #35214, #7989, .T. ) ;
#22920 = ORIENTED_EDGE ( 'NONE', *, *, #10803, .T. ) ;
#22921 = CARTESIAN_POINT ( 'NONE',  ( -23.54764978442466727, -11.41761097281034409, 66.64887858452939895 ) ) ;
#22922 = ADVANCED_FACE ( 'NONE', ( #33804 ), #8615, .T. ) ;
#22923 = CARTESIAN_POINT ( 'NONE',  ( -22.97645422746545663, -19.15384556476019995, 58.88970445631586159 ) ) ;
#22924 = VECTOR ( 'NONE', #6070, 1000.000000000000114 ) ;
#22925 = ORIENTED_EDGE ( 'NONE', *, *, #44676, .F. ) ;
#22926 = CARTESIAN_POINT ( 'NONE',  ( -10.37818569806566948, -17.22973468411262132, 61.27247807055057649 ) ) ;
#22927 = CARTESIAN_POINT ( 'NONE',  ( -17.66159697976433307, -21.85550285805611637, 58.42025434932890704 ) ) ;
#22928 = EDGE_CURVE ( 'NONE', #47072, #34499, #22402, .T. ) ;
#22929 = CARTESIAN_POINT ( 'NONE',  ( -14.97188219925329378, -8.199429090594037461, 56.84999999999995168 ) ) ;
#22930 = ORIENTED_EDGE ( 'NONE', *, *, #32405, .T. ) ;
#22932 = EDGE_CURVE ( 'NONE', #19285, #7976, #3205, .T. ) ;
#22931 = DIRECTION ( 'NONE',  ( -3.413470714839332458E-33, 1.190614954331866791E-16, -1.000000000000000000 ) ) ;
#22933 = ORIENTED_EDGE ( 'NONE', *, *, #12349, .T. ) ;
#22934 = B_SPLINE_CURVE_WITH_KNOTS ( 'NONE', 3,
 ( #21846, #25311, #40322, #36129, #28524, #17657, #47479, #25538, #14419, #28755 ),
 .UNSPECIFIED., .F., .F.,
 ( 4, 2, 2, 2, 4 ),
 ( 0.000000000000000000, 0.2500000000000000000, 0.5000000000000000000, 0.7500000000000000000, 1.000000000000000000 ),
 .UNSPECIFIED. ) ;
#22935 = FACE_OUTER_BOUND ( 'NONE', #4441, .T. ) ;
#22936 = CARTESIAN_POINT ( 'NONE',  ( -11.35070632453979478, -11.22329048540824559, 57.09414325051740491 ) ) ;
#22937 = VERTEX_POINT ( 'NONE', #14017 ) ;
#22938 = CARTESIAN_POINT ( 'NONE',  ( -16.52316554273587101, -21.80170452179945073, 65.24036514508233608 ) ) ;
#22939 = DIRECTION ( 'NONE',  ( -4.115385489419834812E-17, -0.9999954153791273948, -0.003028072113822188795 ) ) ;
#22940 = CARTESIAN_POINT ( 'NONE',  ( -21.82409385650551670, -6.426201560718813433, 50.50509628382439331 ) ) ;
#22941 = AXIS2_PLACEMENT_3D ( 'NONE', #44937, #22769, #3304 ) ;
#22942 = CARTESIAN_POINT ( 'NONE',  ( -11.35825037048775066, -11.21643016533577075, 60.67885780704619947 ) ) ;
#22943 = DIRECTION ( 'NONE',  ( 3.071710424422018668E-17, -6.404604876783312462E-16, -1.000000000000000000 ) ) ;
#22944 = CARTESIAN_POINT ( 'NONE',  ( -10.55151208239364635, -17.68521041179895548, 68.28217381303441869 ) ) ;
#22945 = CARTESIAN_POINT ( 'NONE',  ( -13.37591485149932602, -8.555017749724795451, 57.16956523174690119 ) ) ;
#22946 = VERTEX_POINT ( 'NONE', #37156 ) ;
#22947 = LINE ( 'NONE', #45832, #1917 ) ;
#22948 = CARTESIAN_POINT ( 'NONE',  ( -24.72409385541305582, -14.80920654474426357, 72.98823529411762934 ) ) ;
#22949 = CARTESIAN_POINT ( 'NONE',  ( -13.41327670018355001, -20.54622194888242603, 58.34650078082590596 ) ) ;
#22950 = CARTESIAN_POINT ( 'NONE',  ( -18.71756812234623979, -7.929749856837892352, 70.67068030594712980 ) ) ;
#22951 = CARTESIAN_POINT ( 'NONE',  ( -24.21188451782586881, -13.09817894282342898, 63.13264126965447076 ) ) ;
#22952 = ORIENTED_EDGE ( 'NONE', *, *, #27239, .T. ) ;
#22953 = ORIENTED_EDGE ( 'NONE', *, *, #6734, .F. ) ;
#22954 = PLANE ( 'NONE',  #26705 ) ;
#22955 = CARTESIAN_POINT ( 'NONE',  ( -10.34189029804177906, -12.49727573565278504, 60.99842349757105353 ) ) ;
#22956 = VERTEX_POINT ( 'NONE', #29549 ) ;
#22957 = DIRECTION ( 'NONE',  ( 1.000000000000000000, 0.000000000000000000, -5.466375705775733989E-17 ) ) ;
#22958 = AXIS2_PLACEMENT_3D ( 'NONE', #36143, #10547, #9825 ) ;
#22959 = DIRECTION ( 'NONE',  ( -7.130145686836404013E-06, 1.088473443322539125E-05, 0.9999999999153418306 ) ) ;
#22960 = CARTESIAN_POINT ( 'NONE',  ( -23.00454255336054743, -10.50046069577333441, 59.88731295783226471 ) ) ;
#22961 = CARTESIAN_POINT ( 'NONE',  ( -13.38462805196022565, -20.58720062598995426, 58.34650077712429095 ) ) ;
#22962 = ADVANCED_FACE ( 'NONE', ( #6662 ), #21917, .T. ) ;
#22963 = CARTESIAN_POINT ( 'NONE',  ( -23.55811799921815819, -19.03726020201580837, 65.92415190940894831 ) ) ;
#22964 = CARTESIAN_POINT ( 'NONE',  ( -22.37985683132060188, -19.82347751554591753, 69.47417989525709459 ) ) ;
#22965 = CIRCLE ( 'NONE', #1715, 1.999999999999999556 ) ;
#22966 = DIRECTION ( 'NONE',  ( 0.9687793358424821033, -0.2479245821708677133, 0.000000000000000000 ) ) ;
#22967 = LINE ( 'NONE', #11142, #38888 ) ;
#22968 = DIRECTION ( 'NONE',  ( -0.1240347345892086062, 1.145860353393066553E-16, -0.9922778767136676281 ) ) ;
#22969 = CARTESIAN_POINT ( 'NONE',  ( -21.59804182614902146, -20.98026282434625500, 72.70941811628220819 ) ) ;
#22970 = FACE_OUTER_BOUND ( 'NONE', #46291, .T. ) ;
#22971 = ADVANCED_FACE ( 'NONE', ( #2950 ), #17962, .T. ) ;
#22972 = ORIENTED_EDGE ( 'NONE', *, *, #48322, .T. ) ;
#22973 = ORIENTED_EDGE ( 'NONE', *, *, #24938, .T. ) ;
#22974 = CARTESIAN_POINT ( 'NONE',  ( -14.14284385541304800, -7.587656875400194068, 49.25157356644813689 ) ) ;
#22975 = CIRCLE ( 'NONE', #28448, 2.000000000000001776 ) ;
#22976 = ORIENTED_EDGE ( 'NONE', *, *, #10858, .F. ) ;
#22977 = CARTESIAN_POINT ( 'NONE',  ( -14.72778360411233045, -21.32322305517535099, 58.31617885012778402 ) ) ;
#22978 = VECTOR ( 'NONE', #15114, 1000.000000000000000 ) ;
#22979 = CARTESIAN_POINT ( 'NONE',  ( -10.03884236986523604, -13.82852981289494210, 57.70470977341523167 ) ) ;
#22980 =( BOUNDED_CURVE ( )  B_SPLINE_CURVE ( 3, ( #29250, #44286, #25546, #6838 ),
 .UNSPECIFIED., .F., .F. ) 
 B_SPLINE_CURVE_WITH_KNOTS ( ( 4, 4 ),
 ( 0.5000000000000000000, 0.9074455897393668424 ),
 .UNSPECIFIED. ) 
 CURVE ( )  GEOMETRIC_REPRESENTATION_ITEM ( )  RATIONAL_B_SPLINE_CURVE ( ( 1.000000000000035083, 0.4567392136813309134, 0.3561768502900051203, 0.6983129098260960621 ) ) 
 REPRESENTATION_ITEM ( '' )  );
#22981 = ADVANCED_FACE ( 'NONE', ( #12895 ), #7158, .F. ) ;
#22982 = CARTESIAN_POINT ( 'NONE',  ( -13.61159385759799001, -8.990409506049202193, 49.61344411288074951 ) ) ;
#22983 = CARTESIAN_POINT ( 'NONE',  ( -17.05968203966123298, -22.25103879409192231, 72.27887915399999486 ) ) ;
#22984 = VERTEX_POINT ( 'NONE', #18212 ) ;
#22985 = EDGE_CURVE ( 'NONE', #20660, #40480, #27151, .T. ) ;
#22986 = CARTESIAN_POINT ( 'NONE',  ( -13.99679447977218061, -20.97040113148658591, 71.94079819673058296 ) ) ;
#22987 = CARTESIAN_POINT ( 'NONE',  ( -9.990608257894338706, -8.638304610707185915, 54.49999999999995026 ) ) ;
#22988 = ORIENTED_EDGE ( 'NONE', *, *, #5735, .F. ) ;
#22989 = CARTESIAN_POINT ( 'NONE',  ( -22.33041777183100507, -20.41561037748852669, 62.34943743628787161 ) ) ;
#22990 = AXIS2_PLACEMENT_3D ( 'NONE', #46250, #4894, #40010 ) ;
#22991 =( BOUNDED_SURFACE ( )  B_SPLINE_SURFACE ( 3, 1, ( 
 ( #36358, #22086 ),
 ( #36585, #2637 ),
 ( #37083, #43775 ),
 ( #47943, #47220 ),
 ( #17643, #2869 ),
 ( #21118, #29229 ),
 ( #44268, #10522 ) ),
 .UNSPECIFIED., .T., .F., .F. ) 
 B_SPLINE_SURFACE_WITH_KNOTS ( ( 4, 3, 4 ),
 ( 2, 2 ),
 ( 0.000000000000000000, 0.5000000000000000000, 1.000000000000000000 ),
 ( 0.000000000000000000, 1.000000000000000000 ),
 .UNSPECIFIED. ) 
 GEOMETRIC_REPRESENTATION_ITEM ( )  RATIONAL_B_SPLINE_SURFACE ( (
 ( 1.000000000000000000, 1.000000000000000000),
 ( 0.3333333333333335369, 0.3333333333333330373),
 ( 0.3333333333333335369, 0.3333333333333330373),
 ( 1.000000000000000000, 1.000000000000000000),
 ( 0.3333333333333333703, 0.3333333333333333703),
 ( 0.3333333333333333703, 0.3333333333333333703),
 ( 1.000000000000000000, 1.000000000000000000) ) ) 
 REPRESENTATION_ITEM ( '' )  SURFACE ( )  );
#22992 = CARTESIAN_POINT ( 'NONE',  ( -23.98474799315784978, -17.25007060033011896, 69.41339792561625188 ) ) ;
#22993 = EDGE_LOOP ( 'NONE', ( #36132, #5426, #31775, #42200 ) ) ;
#22994 = CYLINDRICAL_SURFACE ( 'NONE', #22892, 4.686499999999997002 ) ;
#22995 = CARTESIAN_POINT ( 'NONE',  ( -15.12990733413706046, -8.194132228790286021, 56.96073009183007940 ) ) ;
#22996 = ORIENTED_EDGE ( 'NONE', *, *, #20532, .F. ) ;
#22997 = CARTESIAN_POINT ( 'NONE',  ( -10.93436299408032752, -11.15019271687858726, 64.31028572978402735 ) ) ;
#22998 = DIRECTION ( 'NONE',  ( 0.000000000000000000, -1.000000000000000000, 9.912705577010318647E-16 ) ) ;
#22999 = ADVANCED_FACE ( 'NONE', ( #33218 ), #35549, .T. ) ;
#23000 = CARTESIAN_POINT ( 'NONE',  ( -11.57022994764690260, -10.20106918018851339, 71.06869474401152331 ) ) ;
#23001 = ORIENTED_EDGE ( 'NONE', *, *, #31904, .F. ) ;
#23002 = CARTESIAN_POINT ( 'NONE',  ( -24.31477923169101629, -16.30090137217950641, 59.40860294853779777 ) ) ;
#23003 = DIRECTION ( 'NONE',  ( -3.071710424422018668E-17, 6.404604876783312462E-16, 1.000000000000000000 ) ) ;
#23004 = CARTESIAN_POINT ( 'NONE',  ( -20.25191534917340874, -8.350868906188830820, 70.26572394742477456 ) ) ;
#23005 = ADVANCED_FACE ( 'NONE', ( #43197 ), #40650, .T. ) ;
#23006 =( BOUNDED_CURVE ( )  B_SPLINE_CURVE ( 3, ( #23040, #10968, #15363, #29434 ),
 .UNSPECIFIED., .F., .F. ) 
 B_SPLINE_CURVE_WITH_KNOTS ( ( 4, 4 ),
 ( 0.5000000000000000000, 0.9074455897393631787 ),
 .UNSPECIFIED. ) 
 CURVE ( )  GEOMETRIC_REPRESENTATION_ITEM ( )  RATIONAL_B_SPLINE_CURVE ( ( 0.9999999999999653610, 0.4567392136813298587, 0.3561768502900535815, 0.6983129098260990597 ) ) 
 REPRESENTATION_ITEM ( '' )  );
#23007 = CARTESIAN_POINT ( 'NONE',  ( -13.06813783877040791, -9.265530354883376063, 67.66470656304637998 ) ) ;
#23008 = DIRECTION ( 'NONE',  ( -0.3478314405900310713, -0.9375570856950864451, 0.000000000000000000 ) ) ;
#23009 = CARTESIAN_POINT ( 'NONE',  ( -10.49862840407593367, -15.82799419795606966, 64.80771590052736997 ) ) ;
#23010 = EDGE_CURVE ( 'NONE', #42266, #3256, #18644, .T. ) ;
#23011 = ADVANCED_FACE ( 'NONE', ( #30306 ), #41125, .T. ) ;
#23012 = CARTESIAN_POINT ( 'NONE',  ( -20.89284385650552522, -7.406986770994972602, 48.81910596585309747 ) ) ;
#23013 = ORIENTED_EDGE ( 'NONE', *, *, #31377, .T. ) ;
#23014 = FACE_OUTER_BOUND ( 'NONE', #2299, .T. ) ;
#23015 = CARTESIAN_POINT ( 'NONE',  ( -11.03951130610352749, -10.96966301366620478, 60.84032324715965245 ) ) ;
#23016 = VERTEX_POINT ( 'NONE', #19442 ) ;
#23017 = CARTESIAN_POINT ( 'NONE',  ( -18.37611662992575390, -7.874247802443992583, 73.94950313365406203 ) ) ;
#23018 = CARTESIAN_POINT ( 'NONE',  ( -21.48659385759799179, -7.222650657624104298, 49.61879703869476543 ) ) ;
#23019 = CARTESIAN_POINT ( 'NONE',  ( -10.42546172544805039, -12.25520447285018122, 57.44362008841285672 ) ) ;
#23020 = VERTEX_POINT ( 'NONE', #12062 ) ;
#23021 = CARTESIAN_POINT ( 'NONE',  ( -17.98089531606498781, -21.84518143609853524, 68.95947724711012938 ) ) ;
#23022 = CARTESIAN_POINT ( 'NONE',  ( -16.94458744105653381, -7.374567917109038362, 74.14513580114275726 ) ) ;
#23023 = CARTESIAN_POINT ( 'NONE',  ( -10.67174875255963329, -12.96329817365894321, 68.03832382196286233 ) ) ;
#23024 = ORIENTED_EDGE ( 'NONE', *, *, #22622, .T. ) ;
#23025 = CARTESIAN_POINT ( 'NONE',  ( -14.25534385650552238, -7.417179338643134834, 52.18511593390279302 ) ) ;
#23026 = DIRECTION ( 'NONE',  ( 0.9687793358424821033, -0.2479245821708679909, 0.000000000000000000 ) ) ;
#23027 = CARTESIAN_POINT ( 'NONE',  ( -24.54825887019308794, -12.63003870855543553, 69.92243000373970574 ) ) ;
#23028 = CARTESIAN_POINT ( 'NONE',  ( -50.42409385541304800, -25.10920654474410441, 47.99999999999998579 ) ) ;
#23029 = CARTESIAN_POINT ( 'NONE',  ( -13.59466166437493762, -8.949414174231923980, 57.26967704109966917 ) ) ;
#23030 = ORIENTED_EDGE ( 'NONE', *, *, #25630, .F. ) ;
#23031 = ORIENTED_EDGE ( 'NONE', *, *, #11852, .T. ) ;
#23032 = CARTESIAN_POINT ( 'NONE',  ( -14.84909385650551705, -8.104110260919579645, 48.81699501597546487 ) ) ;
#23033 = EDGE_CURVE ( 'NONE', #41432, #1105, #45432, .T. ) ;
#23034 = CARTESIAN_POINT ( 'NONE',  ( -14.01837044221388417, -8.636059239884620098, 74.48482605064899076 ) ) ;
#23035 = CYLINDRICAL_SURFACE ( 'NONE', #19781, 5.249999999999998224 ) ;
#23036 = DIRECTION ( 'NONE',  ( 0.3109111061729913916, 0.9504389954427825415, 3.354176643444177759E-08 ) ) ;
#23037 = CARTESIAN_POINT ( 'NONE',  ( -14.17409385650551457, -9.792211528768504536, 50.49490371617623197 ) ) ;
#23038 = DIRECTION ( 'NONE',  ( -3.071710424422018668E-17, 6.404604876783312462E-16, 1.000000000000000000 ) ) ;
#23039 = CARTESIAN_POINT ( 'NONE',  ( -10.21764062494887781, -12.91954801228597915, 67.92327636273336111 ) ) ;
#23040 = CARTESIAN_POINT ( 'NONE',  ( -18.44528782684011858, -21.78515541812411982, 72.29983070759432451 ) ) ;
#23041 = EDGE_LOOP ( 'NONE', ( #31553, #20463, #32646, #18244, #39839 ) ) ;
#23042 = DIRECTION ( 'NONE',  ( 1.000000000000000000, 2.866981220435666553E-17, 0.000000000000000000 ) ) ;
#23043 = ORIENTED_EDGE ( 'NONE', *, *, #8442, .F. ) ;
#23044 = CARTESIAN_POINT ( 'NONE',  ( -22.04114742393716142, -9.481025248639415537, 59.73643293354757589 ) ) ;
#23045 = CARTESIAN_POINT ( 'NONE',  ( -20.22893085845381123, -8.395648538660806182, 66.85392180442863719 ) ) ;
#23046 = CARTESIAN_POINT ( 'NONE',  ( -12.51522269766590512, -9.204924993125867871, 74.45776466667307147 ) ) ;
#23047 = DIRECTION ( 'NONE',  ( 3.549360974554993999E-17, -6.371834667797928663E-18, -1.000000000000000000 ) ) ;
#23048 = VERTEX_POINT ( 'NONE', #38144 ) ;
#23049 = CARTESIAN_POINT ( 'NONE',  ( -10.87811525140410929, -17.44835992831754368, 61.31310265544169624 ) ) ;
#23050 = CARTESIAN_POINT ( 'NONE',  ( -24.69336539026762267, -16.44026253781551361, 59.22308793767378177 ) ) ;
#23051 = CARTESIAN_POINT ( 'NONE',  ( -15.69736699998981422, -8.025519224215527103, 70.60989840319118116 ) ) ;
#23052 = CARTESIAN_POINT ( 'NONE',  ( -24.31456807776294227, -16.04512561575171503, 66.34708430620283082 ) ) ;
#23053 = ORIENTED_EDGE ( 'NONE', *, *, #35383, .T. ) ;
#23054 = CARTESIAN_POINT ( 'NONE',  ( -22.69786088827318338, -10.13032044058513748, 70.01738298352940149 ) ) ;
#23055 = CARTESIAN_POINT ( 'NONE',  ( -17.77921064978749044, -22.25082400685520057, 58.59048811498988840 ) ) ;
#23056 = CARTESIAN_POINT ( 'NONE',  ( -10.92750425249182022, -11.16255029878774252, 64.26386639478288032 ) ) ;
#23057 = FACE_BOUND ( 'NONE', #9031, .T. ) ;
#23058 = ORIENTED_EDGE ( 'NONE', *, *, #20324, .F. ) ;
#23059 = EDGE_CURVE ( 'NONE', #9176, #29117, #7023, .T. ) ;
#23060 = EDGE_CURVE ( 'NONE', #46952, #38508, #22410, .T. ) ;
#23061 = CARTESIAN_POINT ( 'NONE',  ( -22.63183829035100914, -15.47396055967928952, 52.02966884056656482 ) ) ;
#23062 = CARTESIAN_POINT ( 'NONE',  ( -10.82687744661835971, -17.29512782721398523, 64.62739381397786076 ) ) ;
#23063 = CIRCLE ( 'NONE', #15966, 1.249999999999999556 ) ;
#23064 = CARTESIAN_POINT ( 'NONE',  ( -15.12736045941317897, -21.89643407171298151, 68.69097498501147925 ) ) ;
#23065 = CARTESIAN_POINT ( 'NONE',  ( -24.83515304063678286, -14.04764234229505959, 73.23776096988058271 ) ) ;
#23066 = EDGE_LOOP ( 'NONE', ( #39889, #39309, #19385, #20816, #21806 ) ) ;
#23067 = CARTESIAN_POINT ( 'NONE',  ( -10.45275820844018355, -14.15883753957306546, 64.57730928593822739 ) ) ;
#23068 = EDGE_LOOP ( 'NONE', ( #29370, #2046, #4864, #22906, #48537 ) ) ;
#23069 = CARTESIAN_POINT ( 'NONE',  ( -14.05371385056185574, -21.00138210837564401, 72.07607703579976999 ) ) ;
#23070 = CARTESIAN_POINT ( 'NONE',  ( -12.10131192688100299, -10.18592936015514816, 64.31442259820508411 ) ) ;
#23071 = VERTEX_POINT ( 'NONE', #42103 ) ;
#23072 = EDGE_CURVE ( 'NONE', #47558, #37481, #23385, .T. ) ;
#23073 = EDGE_CURVE ( 'NONE', #11801, #48136, #32038, .T. ) ;
#23074 = CARTESIAN_POINT ( 'NONE',  ( -21.73662441638723308, -9.231682010981758779, 66.67622112302015580 ) ) ;
#23075 = VERTEX_POINT ( 'NONE', #18453 ) ;
#23076 = ORIENTED_EDGE ( 'NONE', *, *, #5072, .T. ) ;
#23077 = ORIENTED_EDGE ( 'NONE', *, *, #24775, .T. ) ;
#23078 = CARTESIAN_POINT ( 'NONE',  ( -15.15660932275500095, -21.48492473237050859, 65.39124617759186719 ) ) ;
#23079 = PLANE ( 'NONE',  #23389 ) ;
#23080 = CARTESIAN_POINT ( 'NONE',  ( -15.62101046192594289, -7.580605815997546237, 70.72494447658496597 ) ) ;
#23081 = CARTESIAN_POINT ( 'NONE',  ( -12.01648161716052954, -10.28590799842451098, 67.79896869921918778 ) ) ;
#23082 = CARTESIAN_POINT ( 'NONE',  ( -19.30271816048872324, -8.014114901043837946, 60.26092997144682784 ) ) ;
#23083 = CARTESIAN_POINT ( 'NONE',  ( -10.64854695470030599, -12.86019059820356958, 64.55364013863997741 ) ) ;
#23084 = CARTESIAN_POINT ( 'NONE',  ( -10.51729421260818498, -16.22293138110306998, 71.44750383217574097 ) ) ;
#23085 = ORIENTED_EDGE ( 'NONE', *, *, #12809, .F. ) ;
#23086 = EDGE_LOOP ( 'NONE', ( #11790, #8841, #45093, #19270, #7001 ) ) ;
#23087 = CARTESIAN_POINT ( 'NONE',  ( -24.40844971322602319, -15.79084262311724629, 73.41792560911460441 ) ) ;
#23088 = ADVANCED_FACE ( 'NONE', ( #264 ), #22918, .F. ) ;
#23089 = CARTESIAN_POINT ( 'NONE',  ( -11.87774890630698899, -9.834968260482170876, 64.19060820317955063 ) ) ;
#23090 = CARTESIAN_POINT ( 'NONE',  ( -19.61601425152793254, -21.50980239257335569, 65.61486213821591207 ) ) ;
#23091 = CARTESIAN_POINT ( 'NONE',  ( -13.54822921233619226, -20.69819393533649077, 61.51646323540209949 ) ) ;
#23092 = ORIENTED_EDGE ( 'NONE', *, *, #33153, .F. ) ;
#23093 = CARTESIAN_POINT ( 'NONE',  ( -15.21159385650551776, -6.922745924619793101, 51.69366785382590024 ) ) ;
#23094 = EDGE_LOOP ( 'NONE', ( #2774, #2938, #48565, #42017, #45698 ) ) ;
#23095 = B_SPLINE_CURVE_WITH_KNOTS ( 'NONE', 3,
 ( #9652, #8920, #38943, #31314, #34999, #1264, #9400, #20719, #19998, #16272 ),
 .UNSPECIFIED., .F., .F.,
 ( 4, 2, 2, 2, 4 ),
 ( 0.6272669072877873342, 0.7522669073072947299, 0.8772669073268022366, 1.002266907346309743, 1.127266907365817028 ),
 .UNSPECIFIED. ) ;
#23096 = LINE ( 'NONE', #23330, #507 ) ;
#23097 = CARTESIAN_POINT ( 'NONE',  ( -17.42409385541305511, -14.80920654474410725, 47.99999999999998579 ) ) ;
#23098 = AXIS2_PLACEMENT_3D ( 'NONE', #45717, #35079, #31400 ) ;
#23099 = CARTESIAN_POINT ( 'NONE',  ( -15.15518245968824651, -21.43299258235331450, 68.76519962665837227 ) ) ;
#23100 = ORIENTED_EDGE ( 'NONE', *, *, #1893, .F. ) ;
#23101 = DIRECTION ( 'NONE',  ( -1.000000000000000000, 0.000000000000000000, 0.000000000000000000 ) ) ;
#23102 = CARTESIAN_POINT ( 'NONE',  ( -22.08174701096107384, -8.994662730349551438, 63.29130125984253397 ) ) ;
#23103 = CARTESIAN_POINT ( 'NONE',  ( -22.78678841951795420, -19.98074385893927740, 72.75126376599935440 ) ) ;
#23104 =( REPRESENTATION_RELATIONSHIP ('NONE','NONE', #2768, #22625 ) REPRESENTATION_RELATIONSHIP_WITH_TRANSFORMATION ( #24521 )SHAPE_REPRESENTATION_RELATIONSHIP( ) );
#23105 = ORIENTED_EDGE ( 'NONE', *, *, #20686, .T. ) ;
#23106 =( BOUNDED_CURVE ( )  B_SPLINE_CURVE ( 3, ( #43047, #20409, #1925, #1688 ),
 .UNSPECIFIED., .F., .F. ) 
 B_SPLINE_CURVE_WITH_KNOTS ( ( 4, 4 ),
 ( 1.570796326794896558, 1.675516081914546707 ),
 .UNSPECIFIED. ) 
 CURVE ( )  GEOMETRIC_REPRESENTATION_ITEM ( )  RATIONAL_B_SPLINE_CURVE ( ( 1.000000000000000000, 0.9990863565030494442, 0.9990863565030494442, 1.000000000000000000 ) ) 
 REPRESENTATION_ITEM ( '' )  );
#23107 = DIRECTION ( 'NONE',  ( -2.866981220435666553E-17, 1.000000000000000000, 1.190614954331866791E-16 ) ) ;
#23108 = CARTESIAN_POINT ( 'NONE',  ( -20.14464072020449237, -7.873698051035776579, 73.82072983659610088 ) ) ;
#23109 = ORIENTED_EDGE ( 'NONE', *, *, #39342, .T. ) ;
#23110 = CARTESIAN_POINT ( 'NONE',  ( -10.51021933215485227, -15.90427549348945035, 64.52273984823442277 ) ) ;
#23111 = ORIENTED_EDGE ( 'NONE', *, *, #38859, .F. ) ;
#23112 = DIRECTION ( 'NONE',  ( -3.071710424422018668E-17, 6.404604876783312462E-16, 1.000000000000000000 ) ) ;
#23113 = DIRECTION ( 'NONE',  ( 3.413470714839332458E-33, -1.190614954331866791E-16, 1.000000000000000000 ) ) ;
#23114 = EDGE_LOOP ( 'NONE', ( #28483, #23690, #41956, #11531 ) ) ;
#23115 = EDGE_CURVE ( 'NONE', #828, #21857, #33765, .T. ) ;
#23116 = DIRECTION ( 'NONE',  ( -0.3964226963016468375, -0.9180681052388937058, 0.000000000000000000 ) ) ;
#23117 = CARTESIAN_POINT ( 'NONE',  ( -17.92193097897699872, -21.84160713959417421, 62.17535923543130139 ) ) ;
#23118 = CARTESIAN_POINT ( 'NONE',  ( -14.26926634389775828, -8.060150775150390245, 67.36000830278645424 ) ) ;
#23119 = ORIENTED_EDGE ( 'NONE', *, *, #17808, .F. ) ;
#23120 = DIRECTION ( 'NONE',  ( 1.000000000000000000, 2.866981220435666553E-17, 0.000000000000000000 ) ) ;
#23121 = CARTESIAN_POINT ( 'NONE',  ( -22.23346828763840222, -19.89562310515971078, 65.70421727878456863 ) ) ;
#23122 =( BOUNDED_CURVE ( )  B_SPLINE_CURVE ( 3, ( #10916, #44417, #7482, #40951 ),
 .UNSPECIFIED., .F., .F. ) 
 B_SPLINE_CURVE_WITH_KNOTS ( ( 4, 4 ),
 ( 0.5000000000000000000, 0.9074455897393700621 ),
 .UNSPECIFIED. ) 
 CURVE ( )  GEOMETRIC_REPRESENTATION_ITEM ( )  RATIONAL_B_SPLINE_CURVE ( ( 1.000000000000003997, 0.4567392136813233083, 0.3561768502900242162, 0.6983129098261110501 ) ) 
 REPRESENTATION_ITEM ( '' )  );
#23123 = CARTESIAN_POINT ( 'NONE',  ( -10.38078069312423679, -14.50222183502507356, 68.00800126083242958 ) ) ;
#23124 = ORIENTED_EDGE ( 'NONE', *, *, #3198, .F. ) ;
#23125 = CARTESIAN_POINT ( 'NONE',  ( -12.20316607747752613, -9.493609027659992705, 57.27590782196710251 ) ) ;
#23126 = ADVANCED_FACE ( 'NONE', ( #26846 ), #30059, .F. ) ;
#23127 = CARTESIAN_POINT ( 'NONE',  ( -13.19711905255361195, -20.45611100226741641, 58.34650356412061001 ) ) ;
#23128 = VECTOR ( 'NONE', #2514, 1000.000000000000227 ) ;
#23129 = ORIENTED_EDGE ( 'NONE', *, *, #43485, .T. ) ;
#23130 = EDGE_LOOP ( 'NONE', ( #32903, #20582, #36540, #33465, #22433 ) ) ;
#23131 = B_SPLINE_CURVE_WITH_KNOTS ( 'NONE', 3,
 ( #2312, #9720, #47387, #28429, #32369, #36736, #21282, #36280, #32592, #6738 ),
 .UNSPECIFIED., .F., .F.,
 ( 4, 2, 2, 2, 4 ),
 ( 0.6272669072877743446, 0.7522669073072896229, 0.8772669073268047901, 1.002266907346319957, 1.127266907365835236 ),
 .UNSPECIFIED. ) ;
#23132 = EDGE_CURVE ( 'NONE', #19831, #26003, #42608, .T. ) ;
#23133 = DIRECTION ( 'NONE',  ( 0.8244078399817417191, 0.5659962132175737626, 7.627400655798535667E-08 ) ) ;
#23134 = CARTESIAN_POINT ( 'NONE',  ( -10.18401476999287425, -13.05278034840643286, 71.32333300961973066 ) ) ;
#23135 = CARTESIAN_POINT ( 'NONE',  ( -10.72552559342236833, -12.61109755851567549, 60.94853568372188590 ) ) ;
#23136 = CARTESIAN_POINT ( 'NONE',  ( -13.27409385759798965, -6.859212275519751323, 50.50378509014259265 ) ) ;
#23137 = EDGE_CURVE ( 'NONE', #31902, #5757, #2639, .T. ) ;
#23138 = CARTESIAN_POINT ( 'NONE',  ( -10.61330328728660533, -12.98831903967553814, 67.73832347272892207 ) ) ;
#23139 = CARTESIAN_POINT ( 'NONE',  ( -12.40421236734144728, -20.31415489762336435, 68.38011531907731921 ) ) ;
#23140 = CARTESIAN_POINT ( 'NONE',  ( -14.39909385759799143, -8.105421454601382081, 49.25000573077640098 ) ) ;
#23141 =( BOUNDED_CURVE ( )  B_SPLINE_CURVE ( 3, ( #4698, #30084, #18987, #4951 ),
 .UNSPECIFIED., .F., .F. ) 
 B_SPLINE_CURVE_WITH_KNOTS ( ( 4, 4 ),
 ( 0.000000000000000000, 0.4074455897393651771 ),
 .UNSPECIFIED. ) 
 CURVE ( )  GEOMETRIC_REPRESENTATION_ITEM ( )  RATIONAL_B_SPLINE_CURVE ( ( 1.000000000000000000, 0.4567392136813308023, 0.3561768502900298783, 0.6983129098260971723 ) ) 
 REPRESENTATION_ITEM ( '' )  );
#23142 = CARTESIAN_POINT ( 'NONE',  ( -10.76351158211370240, -11.46999907741044034, 67.73209273364366823 ) ) ;
#23143 = ORIENTED_EDGE ( 'NONE', *, *, #19658, .F. ) ;
#23144 = ADVANCED_FACE ( 'NONE', ( #46766 ), #20427, .T. ) ;
#23145 =( NAMED_UNIT ( * ) SI_UNIT ( $, .STERADIAN. ) SOLID_ANGLE_UNIT ( ) );
#23146 = CARTESIAN_POINT ( 'NONE',  ( -45.92409385541293432, 985.6101381041504510, 70.50000000000000000 ) ) ;
#23147 = CARTESIAN_POINT ( 'NONE',  ( -12.49057014363319773, -19.84541670790808965, 64.86674882886633497 ) ) ;
#23148 = ORIENTED_EDGE ( 'NONE', *, *, #47238, .F. ) ;
#23149 = ORIENTED_EDGE ( 'NONE', *, *, #7241, .F. ) ;
#23150 = CARTESIAN_POINT ( 'NONE',  ( -19.90352600502131963, -21.35538510417552516, 69.16997613342608986 ) ) ;
#23151 = DIRECTION ( 'NONE',  ( -2.866981220435666553E-17, 1.000000000000000000, 1.190614954331866791E-16 ) ) ;
#23152 = CARTESIAN_POINT ( 'NONE',  ( -15.40768640085200047, -21.98131303373579115, 72.20608812448921299 ) ) ;
#23153 = CARTESIAN_POINT ( 'NONE',  ( -11.49688049385020960, -18.62690763749001732, 64.76179218520603342 ) ) ;
#23154 = ORIENTED_EDGE ( 'NONE', *, *, #35579, .F. ) ;
#23155 = PLANE ( 'NONE',  #3701 ) ;
#23156 = AXIS2_PLACEMENT_3D ( 'NONE', #33762, #7944, #30103 ) ;
#23157 = CARTESIAN_POINT ( 'NONE',  ( -14.61306878872958137, -8.340592061241681066, 67.67463703838096478 ) ) ;
#23158 = VECTOR ( 'NONE', #20031, 1000.000000000000227 ) ;
#23159 = ORIENTED_EDGE ( 'NONE', *, *, #12542, .T. ) ;
#23160 = CARTESIAN_POINT ( 'NONE',  ( -24.45304548397136202, -14.21871265238332604, 66.18292724403113425 ) ) ;
#23161 = CARTESIAN_POINT ( 'NONE',  ( -23.62594491300536959, -11.45603751788689451, 66.70742424642772050 ) ) ;
#23162 = EDGE_CURVE ( 'NONE', #28374, #46725, #28797, .T. ) ;
#23163 = EDGE_LOOP ( 'NONE', ( #33243, #4749 ) ) ;
#23164 = VERTEX_POINT ( 'NONE', #8622 ) ;
#23165 = DIRECTION ( 'NONE',  ( -3.413470714839332458E-33, 1.190614954331866791E-16, -1.000000000000000000 ) ) ;
#23166 = DIRECTION ( 'NONE',  ( 2.331190576225089612E-06, -8.511884079520847478E-06, 0.9999999999610567070 ) ) ;
#23167 = ORIENTED_EDGE ( 'NONE', *, *, #33440, .F. ) ;
#23168 = CARTESIAN_POINT ( 'NONE',  ( -43.17409385541305511, -14.80920654474410547, 56.99999999999998579 ) ) ;
#23169 = EDGE_CURVE ( 'NONE', #21742, #4040, #47574, .T. ) ;
#23170 = DIRECTION ( 'NONE',  ( -2.866981220435666553E-17, 1.000000000000000000, 1.190614954331866791E-16 ) ) ;
#23171 = CARTESIAN_POINT ( 'NONE',  ( -16.08659385650551599, -9.302874398569244363, 51.68646062012417985 ) ) ;
#23172 = CARTESIAN_POINT ( 'NONE',  ( -24.47217469780903798, -14.64471797168181233, 63.01296487297644688 ) ) ;
#23173 = CARTESIAN_POINT ( 'NONE',  ( -24.20884359724224311, -11.73171579724705005, 59.59740298356196320 ) ) ;
#23174 = CARTESIAN_POINT ( 'NONE',  ( -21.95939004544374740, -9.477125498926222136, 59.72171213236985921 ) ) ;
#23175 = ORIENTED_EDGE ( 'NONE', *, *, #20174, .F. ) ;
#23176 = FACE_OUTER_BOUND ( 'NONE', #19892, .T. ) ;
#23177 = DIRECTION ( 'NONE',  ( 2.866981220435666553E-17, -1.000000000000000000, -1.190614954331866791E-16 ) ) ;
#23178 = CARTESIAN_POINT ( 'NONE',  ( 18.07590614458695200, 2.144077342217588722, 49.43104278224995340 ) ) ;
#23179 = B_SPLINE_CURVE_WITH_KNOTS ( 'NONE', 3,
 ( #24834, #4730, #39843, #28763, #20894, #12110, #9588, #8417, #32224, #45858 ),
 .UNSPECIFIED., .F., .F.,
 ( 4, 2, 2, 2, 4 ),
 ( 0.000000000000000000, 0.2500000000000000000, 0.5000000000000000000, 0.7500000000000000000, 1.000000000000000000 ),
 .UNSPECIFIED. ) ;
#23180 = CARTESIAN_POINT ( 'NONE',  ( -18.58429415988738143, -7.905961439831743931, 70.59741261408042590 ) ) ;
#23181 = CARTESIAN_POINT ( 'NONE',  ( -30.42409385541305156, -25.10920654474410441, 47.99999999999997868 ) ) ;
#23182 = VERTEX_POINT ( 'NONE', #9595 ) ;
#23183 = ORIENTED_EDGE ( 'NONE', *, *, #26850, .T. ) ;
#23184 = EDGE_CURVE ( 'NONE', #37645, #32748, #16996, .T. ) ;
#23185 = CARTESIAN_POINT ( 'NONE',  ( -21.46132405888245032, -9.088780516485673644, 73.71201958758717865 ) ) ;
#23186 = CARTESIAN_POINT ( 'NONE',  ( -10.35661267713556022, -12.45241038966069347, 60.91358145539074798 ) ) ;
#23187 = ORIENTED_EDGE ( 'NONE', *, *, #45646, .T. ) ;
#23188 = CARTESIAN_POINT ( 'NONE',  ( -18.01931865558045942, -7.780653922786444632, 60.38060830724960937 ) ) ;
#23189 = PLANE ( 'NONE',  #24004 ) ;
#23190 = CARTESIAN_POINT ( 'NONE',  ( -21.43034385759799321, -6.857644439848013640, 49.98602051094139398 ) ) ;
#23191 = EDGE_CURVE ( 'NONE', #38842, #15214, #22617, .T. ) ;
#23192 = CARTESIAN_POINT ( 'NONE',  ( -17.35131669183886061, -7.807977842693357040, 70.60108831583485767 ) ) ;
#23193 = CARTESIAN_POINT ( 'NONE',  ( -24.39823041255490921, -14.19330756662983362, 73.19441791716994317 ) ) ;
#23194 = CARTESIAN_POINT ( 'NONE',  ( -19.58430998839561354, -21.93927299186879765, 62.17220519270452428 ) ) ;
#23195 = DIRECTION ( 'NONE',  ( 0.000000000000000000, 1.000000000000000000, 0.000000000000000000 ) ) ;
#23196 = VECTOR ( 'NONE', #17140, 1000.000000000000114 ) ;
#23197 = EDGE_LOOP ( 'NONE', ( #176, #13556, #36541, #4502 ) ) ;
#23198 = EDGE_CURVE ( 'NONE', #508, #28688, #13010, .T. ) ;
#23199 = CARTESIAN_POINT ( 'NONE',  ( -24.38143469521110518, -15.58083332675401067, 73.00303748421107741 ) ) ;
#23200 = AXIS2_PLACEMENT_3D ( 'NONE', #14057, #18250, #48064 ) ;
#23201 = DIRECTION ( 'NONE',  ( -3.071710424422018668E-17, 6.404604876783312462E-16, 1.000000000000000000 ) ) ;
#23202 = ADVANCED_BREP_SHAPE_REPRESENTATION ( '', ( #48318, #29031 ), #47881 ) ;
#23203 = CARTESIAN_POINT ( 'NONE',  ( -24.10584550580110630, -12.56049697540380095, 73.54225570139644219 ) ) ;
#23204 = CARTESIAN_POINT ( 'NONE',  ( -17.72591277258568709, -7.814435863198863075, 63.62227229162045461 ) ) ;
#23205 = DIRECTION ( 'NONE',  ( -3.413470714839332458E-33, 1.190614954331866791E-16, -1.000000000000000000 ) ) ;
#23206 = ADVANCED_FACE ( 'NONE', ( #13244 ), #6728, .T. ) ;
#23207 = CARTESIAN_POINT ( 'NONE',  ( -23.42915847708036381, -11.11517115755410146, 73.64721174900437006 ) ) ;
#23208 = ORIENTED_EDGE ( 'NONE', *, *, #9347, .F. ) ;
#23209 = EDGE_LOOP ( 'NONE', ( #19190, #17530, #31411, #14842 ) ) ;
#23210 = CARTESIAN_POINT ( 'NONE',  ( -20.10030308072983374, -21.76202485516048668, 72.51983413602351902 ) ) ;
#23211 = ORIENTED_EDGE ( 'NONE', *, *, #37603, .T. ) ;
#23212 = DIRECTION ( 'NONE',  ( 5.625773296287788022E-06, 7.100530152274343103E-06, 0.9999999999589664901 ) ) ;
#23213 = CARTESIAN_POINT ( 'NONE',  ( -16.53298114947924802, -21.75231650153539675, 61.98241377463749302 ) ) ;
#23214 =( BOUNDED_SURFACE ( )  B_SPLINE_SURFACE ( 3, 1, ( 
 ( #17088, #6025 ),
 ( #9247, #32137 ),
 ( #24987, #5800 ),
 ( #40005, #28197 ),
 ( #43473, #20809 ),
 ( #28451, #13397 ),
 ( #9735, #6274 ) ),
 .UNSPECIFIED., .T., .F., .F. ) 
 B_SPLINE_SURFACE_WITH_KNOTS ( ( 4, 3, 4 ),
 ( 2, 2 ),
 ( 0.000000000000000000, 0.5000000000000000000, 1.000000000000000000 ),
 ( 0.000000000000000000, 1.000000000000000000 ),
 .UNSPECIFIED. ) 
 GEOMETRIC_REPRESENTATION_ITEM ( )  RATIONAL_B_SPLINE_SURFACE ( (
 ( 1.000000000000000000, 1.000000000000000000),
 ( 0.3333333333333335369, 0.3333333333333330373),
 ( 0.3333333333333335369, 0.3333333333333330373),
 ( 1.000000000000000000, 1.000000000000000000),
 ( 0.3333333333333333703, 0.3333333333333333703),
 ( 0.3333333333333333703, 0.3333333333333333703),
 ( 1.000000000000000000, 1.000000000000000000) ) ) 
 REPRESENTATION_ITEM ( '' )  SURFACE ( )  );
#23215 = B_SPLINE_CURVE_WITH_KNOTS ( 'NONE', 3,
 ( #26628, #22693, #37690, #3980, #18992, #33995, #15271, #7929, #19233, #9128 ),
 .UNSPECIFIED., .F., .F.,
 ( 4, 2, 2, 2, 4 ),
 ( 0.6272669072877684604, 0.7522669073072830725, 0.8772669073267977957, 1.002266907346312408, 1.127266907365827020 ),
 .UNSPECIFIED. ) ;
#23216 = CARTESIAN_POINT ( 'NONE',  ( -13.34362782723684049, -8.575845938274239799, 57.10821201658431789 ) ) ;
#23217 = LINE ( 'NONE', #82, #34033 ) ;
#23218 = EDGE_LOOP ( 'NONE', ( #26089, #17599, #32054, #26849, #46257, #31267, #21598, #35727, #39695, #14913, #30859, #48629, #39983, #21638, #41818, #34568 ) ) ;
#23219 = CARTESIAN_POINT ( 'NONE',  ( -14.23443154292173674, -21.09974595518388440, 71.81118900415394535 ) ) ;
#23220 = CARTESIAN_POINT ( 'NONE',  ( -17.55954837273607438, -7.360311716977308905, 63.72773943437917410 ) ) ;
#23221 = ORIENTED_EDGE ( 'NONE', *, *, #19714, .F. ) ;
#23222 = CARTESIAN_POINT ( 'NONE',  ( -10.83683317046381234, -12.44108562964681219, 57.62857332099802932 ) ) ;
#23223 = EDGE_CURVE ( 'NONE', #34094, #32811, #46040, .T. ) ;
#23224 = DIRECTION ( 'NONE',  ( -8.560949394918188676E-06, 2.380493831898821895E-06, -0.9999999999605216905 ) ) ;
#23225 = AXIS2_PLACEMENT_3D ( 'NONE', #19483, #46330, #28754 ) ;
#23226 = ORIENTED_EDGE ( 'NONE', *, *, #493, .F. ) ;
#23227 = DIRECTION ( 'NONE',  ( 3.549360974554993999E-17, -6.371834667797928663E-18, -1.000000000000000000 ) ) ;
#23228 = CARTESIAN_POINT ( 'NONE',  ( -16.71379370341422543, -22.22534705626145879, 68.95206582789661809 ) ) ;
#23229 = CARTESIAN_POINT ( 'NONE',  ( -24.72409385541305582, -14.90920654474417972, 64.94117647058821774 ) ) ;
#23230 = EDGE_LOOP ( 'NONE', ( #23770, #26948 ) ) ;
#23231 = FACE_OUTER_BOUND ( 'NONE', #12247, .T. ) ;
#23232 = VECTOR ( 'NONE', #12091, 1000.000000000000000 ) ;
#23233 = LINE ( 'NONE', #18538, #12392 ) ;
#23234 = FACE_OUTER_BOUND ( 'NONE', #6985, .T. ) ;
#23235 = B_SPLINE_CURVE_WITH_KNOTS ( 'NONE', 3,
 ( #46978, #27302, #35163, #12519, #42328, #27544, #46515, #12768, #38868, #9576 ),
 .UNSPECIFIED., .F., .F.,
 ( 4, 2, 2, 2, 4 ),
 ( 0.000000000000000000, 0.2500000000000000000, 0.5000000000000000000, 0.7500000000000000000, 1.000000000000000000 ),
 .UNSPECIFIED. ) ;
#23236 = DIRECTION ( 'NONE',  ( 1.000000000000000000, 2.866981220435666553E-17, 0.000000000000000000 ) ) ;
#23237 = EDGE_CURVE ( 'NONE', #48136, #2367, #46697, .T. ) ;
#23238 = CARTESIAN_POINT ( 'NONE',  ( -16.36862302632751209, -10.24310716135927812, 52.02966884056656482 ) ) ;
#23239 = CARTESIAN_POINT ( 'NONE',  ( -11.07752443122393693, -17.88727437471119330, 71.77538231106770183 ) ) ;
#23240 = FACE_OUTER_BOUND ( 'NONE', #11095, .T. ) ;
#23241 = DIRECTION ( 'NONE',  ( -3.071710424422018668E-17, 6.404604876783312462E-16, 1.000000000000000000 ) ) ;
#23242 = CARTESIAN_POINT ( 'NONE',  ( -21.23034385650551670, -9.794322478646142471, 51.19202720610083190 ) ) ;
#23243 = ORIENTED_EDGE ( 'NONE', *, *, #41061, .T. ) ;
#23244 = EDGE_CURVE ( 'NONE', #18974, #46408, #44552, .T. ) ;
#23245 = PLANE ( 'NONE',  #25122 ) ;
#23246 = CARTESIAN_POINT ( 'NONE',  ( -10.99975357571800849, -11.03678792477782622, 60.87159911480458874 ) ) ;
#23247 = ORIENTED_EDGE ( 'NONE', *, *, #1038, .F. ) ;
#23248 = CARTESIAN_POINT ( 'NONE',  ( -15.66191361000415583, -7.982949215278682509, 70.90989811847559565 ) ) ;
#23249 = CARTESIAN_POINT ( 'NONE',  ( -50.42609385541305755, -14.80920654474422271, 68.96470588235293064 ) ) ;
#23250 = ORIENTED_EDGE ( 'NONE', *, *, #30365, .T. ) ;
#23251 = CARTESIAN_POINT ( 'NONE',  ( -14.76542504939979139, -8.279692840553558142, 60.61996284471974406 ) ) ;
#23252 = CARTESIAN_POINT ( 'NONE',  ( -16.94618458872839994, -7.374472604449730184, 74.00372349603880195 ) ) ;
#23253 = EDGE_CURVE ( 'NONE', #20557, #23343, #18910, .T. ) ;
#23254 = CARTESIAN_POINT ( 'NONE',  ( -18.96774969734608618, -7.981470143064878897, 63.65762499020824805 ) ) ;
#23255 = EDGE_LOOP ( 'NONE', ( #14525, #14144, #7690, #7258 ) ) ;
#23256 = CARTESIAN_POINT ( 'NONE',  ( -17.15134141312287852, -7.364115244199362920, 70.67531166753866501 ) ) ;
#23257 = EDGE_CURVE ( 'NONE', #46413, #44873, #32189, .T. ) ;
#23258 = DIRECTION ( 'NONE',  ( 1.000000000000000000, 0.000000000000000000, 0.000000000000000000 ) ) ;
#23259 = CARTESIAN_POINT ( 'NONE',  ( -10.41531639268335496, -14.04517892474411589, 60.93293405735092705 ) ) ;
#23260 =( BOUNDED_SURFACE ( )  B_SPLINE_SURFACE ( 3, 1, ( 
 ( #26600, #37405 ),
 ( #22664, #269 ),
 ( #4200, #19205 ),
 ( #37915, #34211 ),
 ( #18706, #33972 ),
 ( #23157, #41128 ),
 ( #3702, #33714 ) ),
 .UNSPECIFIED., .T., .F., .F. ) 
 B_SPLINE_SURFACE_WITH_KNOTS ( ( 4, 3, 4 ),
 ( 2, 2 ),
 ( 0.000000000000000000, 0.5000000000000000000, 1.000000000000000000 ),
 ( 0.000000000000000000, 1.000000000000000000 ),
 .UNSPECIFIED. ) 
 GEOMETRIC_REPRESENTATION_ITEM ( )  RATIONAL_B_SPLINE_SURFACE ( (
 ( 1.000000000000000000, 1.000000000000000000),
 ( 0.3333333333333335369, 0.3333333333333330373),
 ( 0.3333333333333335369, 0.3333333333333330373),
 ( 1.000000000000000000, 1.000000000000000000),
 ( 0.3333333333333333703, 0.3333333333333333703),
 ( 0.3333333333333333703, 0.3333333333333333703),
 ( 1.000000000000000000, 1.000000000000000000) ) ) 
 REPRESENTATION_ITEM ( '' )  SURFACE ( )  );
#23261 = DIRECTION ( 'NONE',  ( -0.7506333037770542838, 0.6607190350373937093, 0.000000000000000000 ) ) ;
#23262 = CARTESIAN_POINT ( 'NONE',  ( -23.16981202414103080, -18.80754655606318693, 62.54509979339044179 ) ) ;
#23263 = ORIENTED_EDGE ( 'NONE', *, *, #2601, .T. ) ;
#23264 = ORIENTED_EDGE ( 'NONE', *, *, #2952, .F. ) ;
#23265 = AXIS2_PLACEMENT_3D ( 'NONE', #30841, #23699, #4244 ) ;
#23266 = CARTESIAN_POINT ( 'NONE',  ( -22.18659385541304374, -7.222650657624104298, 49.61879703869476543 ) ) ;
#23267 = LINE ( 'NONE', #30904, #12283 ) ;
#23268 = CARTESIAN_POINT ( 'NONE',  ( -20.25220558506708102, -7.916061535415647832, 70.36445088532752834 ) ) ;
#23269 = DIRECTION ( 'NONE',  ( 1.000000000000000000, 0.000000000000000000, 0.000000000000000000 ) ) ;
#23270 = EDGE_CURVE ( 'NONE', #1137, #35822, #8487, .T. ) ;
#23271 =( BOUNDED_CURVE ( )  B_SPLINE_CURVE ( 3, ( #28925, #10229, #34554, #41223 ),
 .UNSPECIFIED., .F., .F. ) 
 B_SPLINE_CURVE_WITH_KNOTS ( ( 4, 4 ),
 ( 0.4074455897393626236, 0.5000000000000000000 ),
 .UNSPECIFIED. ) 
 CURVE ( )  GEOMETRIC_REPRESENTATION_ITEM ( )  RATIONAL_B_SPLINE_CURVE ( ( 0.6983129098260891787, 0.7760317562606902086, 0.8765941196519926315, 0.9999999999999927836 ) ) 
 REPRESENTATION_ITEM ( '' )  );
#23272 = EDGE_CURVE ( 'NONE', #46893, #9283, #24368, .T. ) ;
#23273 = B_SPLINE_CURVE_WITH_KNOTS ( 'NONE', 1,
 ( #2876, #47474 ),
 .UNSPECIFIED., .F., .F.,
 ( 2, 2 ),
 ( 0.000000000000000000, 1.000000000000000000 ),
 .UNSPECIFIED. ) ;
#23274 = PLANE ( 'NONE',  #41819 ) ;
#23275 = EDGE_CURVE ( 'NONE', #23280, #41320, #26064, .T. ) ;
#23276 = CARTESIAN_POINT ( 'NONE',  ( -20.88147674714181079, -8.209942860146695054, 60.02620543942160225 ) ) ;
#23277 = DIRECTION ( 'NONE',  ( 0.000000000000000000, 0.000000000000000000, 1.000000000000000000 ) ) ;
#23278 = EDGE_LOOP ( 'NONE', ( #36638, #4896 ) ) ;
#23279 = CARTESIAN_POINT ( 'NONE',  ( -14.01118748589248320, -10.49619482288619920, 53.49999999999995026 ) ) ;
#23280 = VERTEX_POINT ( 'NONE', #19148 ) ;
#23281 = DIRECTION ( 'NONE',  ( -0.1675476790616363121, 0.9858639740050647582, -1.222863418168487711E-17 ) ) ;
#23282 = CARTESIAN_POINT ( 'NONE',  ( -20.98899269145036328, -20.89566229441305723, 69.14630445674248449 ) ) ;
#23283 = LINE ( 'NONE', #18585, #6356 ) ;
#23284 = CARTESIAN_POINT ( 'NONE',  ( -11.69468685320639345, -19.67737422254949919, 54.02312124697527906 ) ) ;
#23285 = ORIENTED_EDGE ( 'NONE', *, *, #4735, .F. ) ;
#23286 = CARTESIAN_POINT ( 'NONE',  ( -20.22231478687352890, -8.334269993598422133, 74.02096540213653952 ) ) ;
#23287 = CARTESIAN_POINT ( 'NONE',  ( -10.35661267713556022, -12.45241038966069347, 60.91358145539074798 ) ) ;
#23288 = CARTESIAN_POINT ( 'NONE',  ( -24.46690853180149361, -14.41907004423223171, 62.92116527710209084 ) ) ;
#23289 = ORIENTED_EDGE ( 'NONE', *, *, #954, .F. ) ;
#23290 = CARTESIAN_POINT ( 'NONE',  ( -18.17795515447646792, -21.82680332084924046, 72.42944048533317414 ) ) ;
#23291 = CARTESIAN_POINT ( 'NONE',  ( -17.71538801587749035, -22.25356272040728101, 58.51279210549326848 ) ) ;
#23292 = DIRECTION ( 'NONE',  ( -3.071710424422018668E-17, 6.404604876783312462E-16, 1.000000000000000000 ) ) ;
#23293 = AXIS2_PLACEMENT_3D ( 'NONE', #24108, #19928, #9095 ) ;
#23294 = CARTESIAN_POINT ( 'NONE',  ( -21.15981645306944259, -20.78812328065465920, 69.05450213015602401 ) ) ;
#23295 = PRODUCT_CONTEXT ( 'NONE', #10515, 'mechanical' ) ;
#23296 = DIRECTION ( 'NONE',  ( -0.5420872618288283817, -0.8403222004463036798, 7.592316861452270591E-08 ) ) ;
#23297 = CARTESIAN_POINT ( 'NONE',  ( -14.03034385541274531, -6.857644439846917628, 49.98602051094207610 ) ) ;
#23298 = CARTESIAN_POINT ( 'NONE',  ( -15.19549097431359463, -21.91815212410659086, 68.76088336006283441 ) ) ;
#23299 = LINE ( 'NONE', #16617, #32183 ) ;
#23300 = VERTEX_POINT ( 'NONE', #18163 ) ;
#23301 = DIRECTION ( 'NONE',  ( -2.866981220435666553E-17, 1.000000000000000000, 1.190614954331866791E-16 ) ) ;
#23302 = EDGE_LOOP ( 'NONE', ( #13648, #4372, #9058, #24389, #23956 ) ) ;
#23303 = DIRECTION ( 'NONE',  ( 0.9687793358424821033, -0.2479245821708680464, 0.000000000000000000 ) ) ;
#23304 = ORIENTED_EDGE ( 'NONE', *, *, #37976, .F. ) ;
#23305 = FACE_BOUND ( 'NONE', #10925, .T. ) ;
#23306 = EDGE_CURVE ( 'NONE', #21625, #44542, #7327, .T. ) ;
#23307 = ORIENTED_EDGE ( 'NONE', *, *, #23060, .T. ) ;
#23308 = ORIENTED_EDGE ( 'NONE', *, *, #31431, .T. ) ;
#23309 = ORIENTED_EDGE ( 'NONE', *, *, #11497, .T. ) ;
#23310 = CARTESIAN_POINT ( 'NONE',  ( -17.58740562021222686, -21.86528886929834670, 62.01968736857112674 ) ) ;
#23311 = DIRECTION ( 'NONE',  ( 0.000000000000000000, 0.000000000000000000, 1.000000000000000000 ) ) ;
#23312 = CYLINDRICAL_SURFACE ( 'NONE', #16900, 1.999999999999999556 ) ;
#23313 = DIRECTION ( 'NONE',  ( -3.071710424422018668E-17, 6.404604876783312462E-16, 1.000000000000000000 ) ) ;
#23314 = CARTESIAN_POINT ( 'NONE',  ( -12.58533685989522333, -19.86927988795931554, 68.56487230657450027 ) ) ;
#23315 = CARTESIAN_POINT ( 'NONE',  ( -13.44904343725875684, -12.32681728777199481, 49.52966884056655772 ) ) ;
#23316 = ORIENTED_EDGE ( 'NONE', *, *, #40247, .F. ) ;
#23317 = VERTEX_POINT ( 'NONE', #3642 ) ;
#23318 = CARTESIAN_POINT ( 'NONE',  ( -21.71159385650551599, -6.922745924619793101, 51.69366785382590024 ) ) ;
#23319 = FACE_OUTER_BOUND ( 'NONE', #36657, .T. ) ;
#23320 = CARTESIAN_POINT ( 'NONE',  ( -11.35825037048775066, -11.21643016533576898, 60.67885780704619947 ) ) ;
#23321 = CARTESIAN_POINT ( 'NONE',  ( -21.56183257638102901, -9.162504018457454436, 70.14749226153745099 ) ) ;
#23322 = ORIENTED_EDGE ( 'NONE', *, *, #27212, .F. ) ;
#23323 = CARTESIAN_POINT ( 'NONE',  ( -16.16784385650552025, -6.428312510596451368, 51.20221977374900035 ) ) ;
#23324 = EDGE_CURVE ( 'NONE', #32458, #14076, #8377, .T. ) ;
#23325 = AXIS2_PLACEMENT_3D ( 'NONE', #30511, #42305, #16171 ) ;
#23326 = CIRCLE ( 'NONE', #4437, 5.249999999999998224 ) ;
#23327 = ORIENTED_EDGE ( 'NONE', *, *, #12075, .T. ) ;
#23328 = EDGE_CURVE ( 'NONE', #48564, #38209, #14683, .T. ) ;
#23329 = EDGE_CURVE ( 'NONE', #1270, #8865, #6744, .T. ) ;
#23330 = CARTESIAN_POINT ( 'NONE',  ( -14.24626305875727184, -11.36469298288595731, 49.52966884056655772 ) ) ;
#23331 = DIRECTION ( 'NONE',  ( 1.000000000000000000, -4.164305804376849788E-17, 1.614929280266638808E-16 ) ) ;
#23332 = CARTESIAN_POINT ( 'NONE',  ( -12.23220189640646538, -19.57856266540686718, 58.07682373937821296 ) ) ;
#23333 = VERTEX_POINT ( 'NONE', #18405 ) ;
#23334 = CYLINDRICAL_SURFACE ( 'NONE', #10110, 2.000000000000001332 ) ;
#23335 = CARTESIAN_POINT ( 'NONE',  ( -11.76008542200333018, -19.01204350050032232, 68.10200740694565980 ) ) ;
#23336 = CARTESIAN_POINT ( 'NONE',  ( -24.18875248430348179, -11.68798133371211279, 59.58212113430876400 ) ) ;
#23337 = VERTEX_POINT ( 'NONE', #33659 ) ;
#23338 = CARTESIAN_POINT ( 'NONE',  ( -22.60969001043771698, -13.98939405582217432, 49.52966884056655772 ) ) ;
#23339 = DIRECTION ( 'NONE',  ( -0.1666496227699850730, 0.9805797387979519053, 0.1033986416233890343 ) ) ;
#23340 = CARTESIAN_POINT ( 'NONE',  ( -20.49170831689750472, -8.461258797198503601, 63.59649424907593129 ) ) ;
#23341 = ORIENTED_EDGE ( 'NONE', *, *, #23820, .T. ) ;
#23342 = DIRECTION ( 'NONE',  ( -0.000000000000000000, -1.000000000000000000, -0.000000000000000000 ) ) ;
#23343 = VERTEX_POINT ( 'NONE', #48703 ) ;
#23344 = B_SPLINE_CURVE_WITH_KNOTS ( 'NONE', 1,
 ( #45258, #45019 ),
 .UNSPECIFIED., .F., .F.,
 ( 2, 2 ),
 ( 0.000000000000000000, 1.000000000000000000 ),
 .UNSPECIFIED. ) ;
#23345 = CARTESIAN_POINT ( 'NONE',  ( -19.15853812393435618, -7.563744986369119516, 63.59122566566123425 ) ) ;
#23346 = DIRECTION ( 'NONE',  ( -5.551115123125782702E-17, -1.232595164407830946E-32, -1.000000000000000000 ) ) ;
#23347 = ORIENTED_EDGE ( 'NONE', *, *, #27337, .T. ) ;
#23348 = CYLINDRICAL_SURFACE ( 'NONE', #23468, 4.686499999999997002 ) ;
#23350 = ADVANCED_FACE ( 'NONE', ( #14943 ), #17061, .T. ) ;
#23349 = CARTESIAN_POINT ( 'NONE',  ( -11.08976439687648075, -11.70580308251566315, 74.85839985167115174 ) ) ;
#23351 = DIRECTION ( 'NONE',  ( -1.274157596560980788E-05, -2.329884826735012561E-06, 0.9999999999161118813 ) ) ;
#23352 = EDGE_LOOP ( 'NONE', ( #24236, #10329, #23159, #3581, #8906 ) ) ;
#23353 = CYLINDRICAL_SURFACE ( 'NONE', #27596, 0.1500000000000050182 ) ;
#23354 = UNCERTAINTY_MEASURE_WITH_UNIT (LENGTH_MEASURE( 1.000000000000000082E-05 ), #21908, 'distance_accuracy_value', 'NONE');
#23355 = LINE ( 'NONE', #38116, #47969 ) ;
#23356 = CARTESIAN_POINT ( 'NONE',  ( -11.95103603871087650, -9.754441519819101458, 60.71951479555669096 ) ) ;
#23357 = ORIENTED_EDGE ( 'NONE', *, *, #45220, .T. ) ;
#23358 = CARTESIAN_POINT ( 'NONE',  ( -12.45873566688478107, -9.804017486950373339, 57.10407583662104258 ) ) ;
#23359 = VECTOR ( 'NONE', #47226, 1000.000000000000000 ) ;
#23360 = AXIS2_PLACEMENT_3D ( 'NONE', #40458, #39739, #10670 ) ;
#23361 = DIRECTION ( 'NONE',  ( 0.3126464228004117163, 0.3197690014840504635, 0.8944271909999156334 ) ) ;
#23362 = VERTEX_POINT ( 'NONE', #12487 ) ;
#23363 = EDGE_LOOP ( 'NONE', ( #10812, #28028, #37827, #42898 ) ) ;
#23364 = CARTESIAN_POINT ( 'NONE',  ( -10.47787889545108087, -15.67627839034492787, 61.03789014633728272 ) ) ;
#23365 = LINE ( 'NONE', #30281, #19493 ) ;
#23366 = EDGE_CURVE ( 'NONE', #43494, #7495, #20264, .T. ) ;
#23367 = CARTESIAN_POINT ( 'NONE',  ( -10.40277084706750621, -15.44444119821074679, 57.86792809062919218 ) ) ;
#23368 = CARTESIAN_POINT ( 'NONE',  ( -21.00534385650551883, -8.801233750844183135, 48.81488406609782515 ) ) ;
#23369 = CARTESIAN_POINT ( 'NONE',  ( -12.50974054546264469, -19.79409688107175924, 61.58781908136975147 ) ) ;
#23370 = CARTESIAN_POINT ( 'NONE',  ( -12.89671927708317689, -20.22380232670898081, 68.49224713894388117 ) ) ;
#23371 = CARTESIAN_POINT ( 'NONE',  ( -23.23017095593700532, -18.72167141714702510, 69.52201958683488670 ) ) ;
#23372 = LINE ( 'NONE', #8355, #4868 ) ;
#23373 = ORIENTED_EDGE ( 'NONE', *, *, #8005, .F. ) ;
#23374 = VERTEX_POINT ( 'NONE', #19885 ) ;
#23375 = CARTESIAN_POINT ( 'NONE',  ( -24.72409385541305582, -14.90920654474424190, 70.07647058823528141 ) ) ;
#23376 = CARTESIAN_POINT ( 'NONE',  ( -14.17292126938155761, -21.07377676424729884, 68.61192020317307083 ) ) ;
#23377 = CARTESIAN_POINT ( 'NONE',  ( -17.23248763171904230, -7.758097994416163878, 74.26018367925263419 ) ) ;
#23378 = CARTESIAN_POINT ( 'NONE',  ( -18.66311988809301425, -7.868636481342422329, 70.65595886192740238 ) ) ;
#23379 = ORIENTED_EDGE ( 'NONE', *, *, #4783, .F. ) ;
#23380 = ORIENTED_EDGE ( 'NONE', *, *, #27011, .F. ) ;
#23381 = EDGE_CURVE ( 'NONE', #36678, #29084, #27223, .T. ) ;
#23382 = CARTESIAN_POINT ( 'NONE',  ( -19.85889901765038346, -21.37233916515964438, 69.21353063550283480 ) ) ;
#23383 = LINE ( 'NONE', #41860, #19765 ) ;
#23384 = CARTESIAN_POINT ( 'NONE',  ( -14.99706828511980916, -21.85287925006270626, 65.29092110561946072 ) ) ;
#23385 = LINE ( 'NONE', #37400, #35884 ) ;
#23386 =( BOUNDED_SURFACE ( )  B_SPLINE_SURFACE ( 3, 1, ( 
 ( #11543, #26569 ),
 ( #41588, #19175 ),
 ( #473, #15455 ),
 ( #30523, #35400 ),
 ( #34916, #15952 ),
 ( #24090, #35154 ),
 ( #19911, #4643 ) ),
 .UNSPECIFIED., .T., .F., .F. ) 
 B_SPLINE_SURFACE_WITH_KNOTS ( ( 4, 3, 4 ),
 ( 2, 2 ),
 ( 0.000000000000000000, 0.5000000000000000000, 1.000000000000000000 ),
 ( 0.000000000000000000, 1.000000000000000000 ),
 .UNSPECIFIED. ) 
 GEOMETRIC_REPRESENTATION_ITEM ( )  RATIONAL_B_SPLINE_SURFACE ( (
 ( 1.000000000000000000, 1.000000000000000000),
 ( 0.3333333333333335369, 0.3333333333333330373),
 ( 0.3333333333333335369, 0.3333333333333330373),
 ( 1.000000000000000000, 1.000000000000000000),
 ( 0.3333333333333333703, 0.3333333333333333703),
 ( 0.3333333333333333703, 0.3333333333333333703),
 ( 1.000000000000000000, 1.000000000000000000) ) ) 
 REPRESENTATION_ITEM ( '' )  SURFACE ( )  );
#23387 = ORIENTED_EDGE ( 'NONE', *, *, #41868, .T. ) ;
#23388 = CARTESIAN_POINT ( 'NONE',  ( -24.84793648988037518, -14.18443574041886457, 69.83770584630335065 ) ) ;
#23389 = AXIS2_PLACEMENT_3D ( 'NONE', #15167, #14415, #48425 ) ;
#23390 = CIRCLE ( 'NONE', #31257, 0.4000000000000011879 ) ;
#23391 = EDGE_CURVE ( 'NONE', #38482, #26173, #14374, .T. ) ;
#23392 = ADVANCED_FACE ( 'NONE', ( #12245 ), #34393, .T. ) ;
#23393 = CARTESIAN_POINT ( 'NONE',  ( -19.55442184481404766, -21.52995072282663358, 65.47958309245051112 ) ) ;
#23394 = VERTEX_POINT ( 'NONE', #1394 ) ;
#23395 = EDGE_CURVE ( 'NONE', #20101, #5342, #38327, .T. ) ;
#23396 = VECTOR ( 'NONE', #29279, 1000.000000000000000 ) ;
#23397 = CARTESIAN_POINT ( 'NONE',  ( -12.86134249074305913, -20.11797452945269882, 72.10653668688858886 ) ) ;
#23398 = EDGE_CURVE ( 'NONE', #5898, #10296, #9050, .T. ) ;
#23399 = CARTESIAN_POINT ( 'NONE',  ( -13.97837889017616320, -8.203094814523453238, 74.38609903144701718 ) ) ;
#23400 =( BOUNDED_CURVE ( )  B_SPLINE_CURVE ( 3, ( #31287, #15771, #31054, #46071 ),
 .UNSPECIFIED., .F., .F. ) 
 B_SPLINE_CURVE_WITH_KNOTS ( ( 4, 4 ),
 ( 0.5000000000000000000, 0.9074455897393672865 ),
 .UNSPECIFIED. ) 
 CURVE ( )  GEOMETRIC_REPRESENTATION_ITEM ( )  RATIONAL_B_SPLINE_CURVE ( ( 0.9999999999999759082, 0.4567392136813248626, 0.3561768502900444222, 0.6983129098261084966 ) ) 
 REPRESENTATION_ITEM ( '' )  );
#23401 = ORIENTED_EDGE ( 'NONE', *, *, #8722, .T. ) ;
#23402 =( BOUNDED_CURVE ( )  B_SPLINE_CURVE ( 3, ( #4431, #37918, #23160, #33225 ),
 .UNSPECIFIED., .F., .F. ) 
 B_SPLINE_CURVE_WITH_KNOTS ( ( 4, 4 ),
 ( 0.000000000000000000, 0.4074455897393657322 ),
 .UNSPECIFIED. ) 
 CURVE ( )  GEOMETRIC_REPRESENTATION_ITEM ( )  RATIONAL_B_SPLINE_CURVE ( ( 1.000000000000000000, 0.4567392136813294146, 0.3561768502900293787, 0.6983129098260999479 ) ) 
 REPRESENTATION_ITEM ( '' )  );
#23403 = CARTESIAN_POINT ( 'NONE',  ( -45.92409385541306932, -16.43194983366065287, 69.94390897503836868 ) ) ;
#23404 = ORIENTED_EDGE ( 'NONE', *, *, #559, .T. ) ;
#23405 = CARTESIAN_POINT ( 'NONE',  ( -21.43863153483710349, -12.36809147865652747, 52.02966884056656482 ) ) ;
#23406 = PLANE ( 'NONE',  #2973 ) ;
#23407 = ORIENTED_EDGE ( 'NONE', *, *, #42946, .F. ) ;
#23408 = CARTESIAN_POINT ( 'NONE',  ( -13.88419686192642111, -8.703135698866935499, 57.11400917758039952 ) ) ;
#23409 = CARTESIAN_POINT ( 'NONE',  ( -10.29140437080923220, -12.65793278909525377, 64.46174418839692066 ) ) ;
#23410 = EDGE_CURVE ( 'NONE', #26632, #28414, #29062, .T. ) ;
#23411 = CARTESIAN_POINT ( 'NONE',  ( -19.01159385650551670, -6.922745924619793101, 51.69366785382590024 ) ) ;
#23412 = CARTESIAN_POINT ( 'NONE',  ( -21.37011387998928669, -21.12839667555923029, 69.24788507571554419 ) ) ;
#23413 = CARTESIAN_POINT ( 'NONE',  ( -22.17153284776674482, -17.05070671513899683, 50.77966884056655772 ) ) ;
#23414 = DIRECTION ( 'NONE',  ( -1.000000000000000000, 4.164305804376849172E-17, -1.614929280266638808E-16 ) ) ;
#23415 = ORIENTED_EDGE ( 'NONE', *, *, #11385, .F. ) ;
#23416 = CARTESIAN_POINT ( 'NONE',  ( -15.28291064399146215, -21.52618758091310980, 68.57592918174772478 ) ) ;
#23417 =( BOUNDED_SURFACE ( )  B_SPLINE_SURFACE ( 3, 1, ( 
 ( #5753, #17034 ),
 ( #47103, #43906 ),
 ( #43663, #13343 ),
 ( #42925, #25180 ),
 ( #39951, #9918 ),
 ( #36244, #2526 ),
 ( #27900, #21489 ) ),
 .UNSPECIFIED., .T., .F., .F. ) 
 B_SPLINE_SURFACE_WITH_KNOTS ( ( 4, 3, 4 ),
 ( 2, 2 ),
 ( 0.000000000000000000, 0.5000000000000000000, 1.000000000000000000 ),
 ( 0.000000000000000000, 1.000000000000000000 ),
 .UNSPECIFIED. ) 
 GEOMETRIC_REPRESENTATION_ITEM ( )  RATIONAL_B_SPLINE_SURFACE ( (
 ( 1.000000000000000000, 1.000000000000000000),
 ( 0.3333333333333335369, 0.3333333333333330373),
 ( 0.3333333333333335369, 0.3333333333333330373),
 ( 1.000000000000000000, 1.000000000000000000),
 ( 0.3333333333333333703, 0.3333333333333333703),
 ( 0.3333333333333333703, 0.3333333333333333703),
 ( 1.000000000000000000, 1.000000000000000000) ) ) 
 REPRESENTATION_ITEM ( '' )  SURFACE ( )  );
#23418 = CARTESIAN_POINT ( 'NONE',  ( -13.65948078749761585, -20.77935321253323053, 58.20216925893738846 ) ) ;
#23419 = CARTESIAN_POINT ( 'NONE',  ( 18.62590614458706995, 1.890747609047893185, 50.53028072113869484 ) ) ;
#23420 = FACE_OUTER_BOUND ( 'NONE', #20970, .T. ) ;
#23421 = CARTESIAN_POINT ( 'NONE',  ( -20.74847686076342157, -20.96993771475205293, 62.13088051185322769 ) ) ;
#23422 = ORIENTED_EDGE ( 'NONE', *, *, #40052, .F. ) ;
#23423 = ORIENTED_EDGE ( 'NONE', *, *, #18084, .T. ) ;
#23424 = CARTESIAN_POINT ( 'NONE',  ( -18.59601872632196873, -7.856991649524070809, 73.85536540707786912 ) ) ;
#23425 = CARTESIAN_POINT ( 'NONE',  ( -14.72744631621160494, -8.295007313424175521, 60.60524229057013201 ) ) ;
#23426 = ORIENTED_EDGE ( 'NONE', *, *, #3826, .F. ) ;
#23428 = FACE_OUTER_BOUND ( 'NONE', #42751, .T. ) ;
#23427 = VECTOR ( 'NONE', #32420, 1000.000000000000000 ) ;
#23429 = CARTESIAN_POINT ( 'NONE',  ( -15.06075745000970834, -21.87520294740874149, 68.76248218113177302 ) ) ;
#23430 = CARTESIAN_POINT ( 'NONE',  ( -10.45630165105249532, -15.48121050910559937, 57.86792791455135188 ) ) ;
#23431 = LINE ( 'NONE', #4717, #26699 ) ;
#23432 = CARTESIAN_POINT ( 'NONE',  ( -11.30174378650323064, -18.30512181131203064, 57.81274399976084766 ) ) ;
#23433 = VECTOR ( 'NONE', #6703, 1000.000000000000114 ) ;
#23434 = CARTESIAN_POINT ( 'NONE',  ( -50.42609385541305755, -14.80920654474420139, 66.05294117647058272 ) ) ;
#23435 = ORIENTED_EDGE ( 'NONE', *, *, #45705, .F. ) ;
#23436 = DIRECTION ( 'NONE',  ( 1.224646799147353207E-16, 1.000000000000000000, -1.912410701131276611E-32 ) ) ;
#23437 = SURFACE_STYLE_FILL_AREA ( #19488 ) ;
#23438 = CARTESIAN_POINT ( 'NONE',  ( -11.06712629860931152, -18.69414434431124761, 61.39215439313597500 ) ) ;
#23439 = AXIS2_PLACEMENT_3D ( 'NONE', #1785, #27643, #27161 ) ;
#23440 = CARTESIAN_POINT ( 'NONE',  ( -11.67943375510494874, -18.89645239624664796, 68.50217487844219022 ) ) ;
#23441 = CARTESIAN_POINT ( 'NONE',  ( -21.43520510711937277, -9.072323815021505311, 70.14634923480093676 ) ) ;
#23442 = EDGE_CURVE ( 'NONE', #20668, #25586, #45734, .T. ) ;
#23443 = CARTESIAN_POINT ( 'NONE',  ( -14.78750802578769452, -21.29541614796527682, 61.82527411501091308 ) ) ;
#23444 = VECTOR ( 'NONE', #45544, 1000.000000000000000 ) ;
#23445 = ORIENTED_EDGE ( 'NONE', *, *, #39858, .T. ) ;
#23446 = ORIENTED_EDGE ( 'NONE', *, *, #31060, .T. ) ;
#23447 = B_SPLINE_CURVE_WITH_KNOTS ( 'NONE', 3,
 ( #41548, #915, #440, #23089, #18628, #30958, #34143, #27012, #45973, #22589 ),
 .UNSPECIFIED., .F., .F.,
 ( 4, 2, 2, 2, 4 ),
 ( 0.1272669073658179995, 0.2522669073439466336, 0.3772669073220752400, 0.5022669073002039575, 0.6272669072783325639 ),
 .UNSPECIFIED. ) ;
#23448 = CARTESIAN_POINT ( 'NONE',  ( -22.13034385650552238, -9.794322478646142471, 51.19202720610083901 ) ) ;
#23449 = ORIENTED_EDGE ( 'NONE', *, *, #24056, .F. ) ;
#23450 = EDGE_CURVE ( 'NONE', #19139, #7346, #45762, .T. ) ;
#23451 = CARTESIAN_POINT ( 'NONE',  ( -17.52853272358826686, -7.759682304905023642, 63.83584969886392457 ) ) ;
#23452 = DIRECTION ( 'NONE',  ( 0.9687793358424821033, -0.2479245821708677133, 0.000000000000000000 ) ) ;
#23453 = ORIENTED_EDGE ( 'NONE', *, *, #23306, .T. ) ;
#23454 = LINE ( 'NONE', #12359, #9372 ) ;
#23455 = CARTESIAN_POINT ( 'NONE',  ( -17.85555652284939043, -7.772123375420258107, 60.09532845646905486 ) ) ;
#23456 = DIRECTION ( 'NONE',  ( -0.9950649908465211135, -0.09922531930717196080, 4.894557008102618136E-08 ) ) ;
#23457 = ORIENTED_EDGE ( 'NONE', *, *, #25091, .F. ) ;
#23458 = ADVANCED_FACE ( 'NONE', ( #688 ), #13892, .T. ) ;
#23459 = CARTESIAN_POINT ( 'NONE',  ( -15.98001679475065373, -7.500493000024420098, 63.76987390602237582 ) ) ;
#23460 = VECTOR ( 'NONE', #33805, 1000.000000000000000 ) ;
#23461 = CARTESIAN_POINT ( 'NONE',  ( -10.47558912380517882, -13.96067967406488464, 57.44824990916067975 ) ) ;
#23462 = EDGE_CURVE ( 'NONE', #34358, #35817, #12056, .T. ) ;
#23463 = AXIS2_PLACEMENT_3D ( 'NONE', #46631, #36004, #13588 ) ;
#23464 = EDGE_LOOP ( 'NONE', ( #34165, #47784, #30224, #36306, #30220 ) ) ;
#23465 = DIRECTION ( 'NONE',  ( 0.000000000000000000, 0.000000000000000000, 1.000000000000000000 ) ) ;
#23466 = CARTESIAN_POINT ( 'NONE',  ( -10.37136279787074500, -14.92680326906059740, 71.32782707526337163 ) ) ;
#23467 = VECTOR ( 'NONE', #37429, 1000.000000000000000 ) ;
#23468 = AXIS2_PLACEMENT_3D ( 'NONE', #9304, #12746, #20384 ) ;
#23469 = ORIENTED_EDGE ( 'NONE', *, *, #34052, .F. ) ;
#23470 = CARTESIAN_POINT ( 'NONE',  ( -23.42532394183187705, -19.22384306421519184, 62.46911594462533657 ) ) ;
#23471 = CARTESIAN_POINT ( 'NONE',  ( -22.51880736180295983, -20.24487813920610790, 65.90410515226939481 ) ) ;
#23472 = CARTESIAN_POINT ( 'NONE',  ( -22.27608729174900049, -12.19078426442220930, 53.88362224778187226 ) ) ;
#23473 = ORIENTED_EDGE ( 'NONE', *, *, #13422, .T. ) ;
#23474 = DIRECTION ( 'NONE',  ( 0.9687793358424821033, -0.2479245821708680464, 0.000000000000000000 ) ) ;
#23475 = CARTESIAN_POINT ( 'NONE',  ( -24.08569470166255400, -11.47342236436628404, 63.12935185382383452 ) ) ;
#23476 = CIRCLE ( 'NONE', #28178, 1.250000000000001998 ) ;
#23477 = EDGE_CURVE ( 'NONE', #25709, #30260, #26586, .T. ) ;
#23478 = CARTESIAN_POINT ( 'NONE',  ( -15.47038646904106507, -21.58309222549749506, 72.34575460768671462 ) ) ;
#23479 = CARTESIAN_POINT ( 'NONE',  ( -21.18836735823073525, -20.77369112572868914, 65.46965119999302374 ) ) ;
#23480 = LINE ( 'NONE', #15823, #7791 ) ;
#23481 = CARTESIAN_POINT ( 'NONE',  ( -17.42409385541299471, -14.80920654474435771, 49.52966884056655772 ) ) ;
#23482 = LINE ( 'NONE', #16060, #29751 ) ;
#23483 = CARTESIAN_POINT ( 'NONE',  ( -17.42409385541300892, -14.80920654474439502, 75.49999999999994316 ) ) ;
#23484 = CARTESIAN_POINT ( 'NONE',  ( -12.85169559483840374, -15.89028456787280952, 49.52966884056655772 ) ) ;
#23485 = CARTESIAN_POINT ( 'NONE',  ( -15.94284385650551883, -8.811426318492348031, 52.18089403414752070 ) ) ;
#23486 = ORIENTED_EDGE ( 'NONE', *, *, #39300, .F. ) ;
#23487 = CARTESIAN_POINT ( 'NONE',  ( -27.42409385541305511, -25.10920654474410441, 45.99999999999998579 ) ) ;
#23488 = CARTESIAN_POINT ( 'NONE',  ( -24.25171713147202368, -16.35308467727669068, 59.12332432120680181 ) ) ;
#23489 = ORIENTED_EDGE ( 'NONE', *, *, #37483, .T. ) ;
#23490 = CYLINDRICAL_SURFACE ( 'NONE', #24525, 0.1499999999999993838 ) ;
#23491 = CARTESIAN_POINT ( 'NONE',  ( -16.17067486245293040, -22.15313371995832625, 58.40772777080032796 ) ) ;
#23492 = CARTESIAN_POINT ( 'NONE',  ( -45.38107656289594871, -12.76354662275040219, 70.87000000000000455 ) ) ;
#23493 = CARTESIAN_POINT ( 'NONE',  ( -14.74690617566109019, -21.27702427001963414, 58.46617884968173229 ) ) ;
#23494 = ORIENTED_EDGE ( 'NONE', *, *, #9945, .F. ) ;
#23495 = CARTESIAN_POINT ( 'NONE',  ( -10.37497031247464463, -14.69804315800203121, 71.62782692816419683 ) ) ;
#23496 = CARTESIAN_POINT ( 'NONE',  ( -20.72573862760241070, -8.580110178657996300, 60.14125250079693785 ) ) ;
#23497 = CARTESIAN_POINT ( 'NONE',  ( -10.09412421677371796, -16.14182453506428061, 68.09955039505892671 ) ) ;
#23498 = VERTEX_POINT ( 'NONE', #39798 ) ;
#23499 = CARTESIAN_POINT ( 'NONE',  ( -23.87505191747562705, -17.66227225522637667, 66.24357201825841912 ) ) ;
#23500 = AXIS2_PLACEMENT_3D ( 'NONE', #20018, #30388, #26929 ) ;
#23501 =( BOUNDED_CURVE ( )  B_SPLINE_CURVE ( 3, ( #25760, #29701, #33612, #41770 ),
 .UNSPECIFIED., .F., .F. ) 
 B_SPLINE_CURVE_WITH_KNOTS ( ( 4, 4 ),
 ( 0.000000000000000000, 0.4074455897393618464 ),
 .UNSPECIFIED. ) 
 CURVE ( )  GEOMETRIC_REPRESENTATION_ITEM ( )  RATIONAL_B_SPLINE_CURVE ( ( 1.000000000000000000, 0.4567392136813374082, 0.3561768502900323208, 0.6983129098260847378 ) ) 
 REPRESENTATION_ITEM ( '' )  );
#23502 = CARTESIAN_POINT ( 'NONE',  ( -36.42409385541304800, -8.109206544743658540, 50.50000000000030553 ) ) ;
#23503 = CARTESIAN_POINT ( 'NONE',  ( -10.00747133761319141, -14.10395761772617362, 60.96175355949325336 ) ) ;
#23504 = EDGE_CURVE ( 'NONE', #24008, #20983, #43100, .T. ) ;
#23505 = CARTESIAN_POINT ( 'NONE',  ( -10.21764033814386963, -12.91954908504599331, 67.92327745040803677 ) ) ;
#23506 = CARTESIAN_POINT ( 'NONE',  ( -17.59331746331979929, -7.761237803891376075, 63.55057029381062961 ) ) ;
#23507 = AXIS2_PLACEMENT_3D ( 'NONE', #34208, #499, #21920 ) ;
#23508 = ORIENTED_EDGE ( 'NONE', *, *, #11329, .T. ) ;
#23509 = VERTEX_POINT ( 'NONE', #20368 ) ;
#23510 = CARTESIAN_POINT ( 'NONE',  ( -21.23034385541303948, -6.857644439848013640, 49.98602051094139398 ) ) ;
#23511 = LINE ( 'NONE', #4793, #27983 ) ;
#23512 = CARTESIAN_POINT ( 'NONE',  ( -50.42609385541305755, -14.90920654474410512, 57.89999999999999147 ) ) ;
#23513 = AXIS2_PLACEMENT_3D ( 'NONE', #48645, #29948, #11231 ) ;
#23514 = SURFACE_STYLE_USAGE ( .BOTH. , #26467 ) ;
#23515 = B_SPLINE_CURVE_WITH_KNOTS ( 'NONE', 3,
 ( #40582, #17458, #21166, #39869, #29278, #5902, #17689, #32714, #39630, #20920 ),
 .UNSPECIFIED., .F., .F.,
 ( 4, 2, 2, 2, 4 ),
 ( 0.6272669072782607325, 0.7522669073001474471, 0.8772669073220342728, 1.002266907343920987, 1.127266907365807702 ),
 .UNSPECIFIED. ) ;
#23516 = CARTESIAN_POINT ( 'NONE',  ( -17.63792724537347212, -22.25688666393347859, 58.59208636575791473 ) ) ;
#23517 = CARTESIAN_POINT ( 'NONE',  ( -20.42320262601612413, -8.483743935243163392, 66.79720689127475453 ) ) ;
#23518 = EDGE_CURVE ( 'NONE', #41967, #7285, #33143, .T. ) ;
#23519 = CARTESIAN_POINT ( 'NONE',  ( -10.41586258189964376, -15.60891902706924306, 64.80771822714827124 ) ) ;
#23520 = CARTESIAN_POINT ( 'NONE',  ( -24.72409385541305582, -15.80920654474410725, 65.99999999999998579 ) ) ;
#23521 = EDGE_CURVE ( 'NONE', #5461, #1862, #35372, .T. ) ;
#23522 = VERTEX_POINT ( 'NONE', #5602 ) ;
#23523 = CARTESIAN_POINT ( 'NONE',  ( -21.68499379980493558, -9.192514338196573931, 66.96149992326067490 ) ) ;
#23524 = DIRECTION ( 'NONE',  ( -3.071710424422018668E-17, 6.404604876783312462E-16, 1.000000000000000000 ) ) ;
#23525 = EDGE_LOOP ( 'NONE', ( #36214, #5376, #42618, #13681, #26483 ) ) ;
#23526 = EDGE_CURVE ( 'NONE', #25093, #11434, #47440, .T. ) ;
#23527 = FACE_OUTER_BOUND ( 'NONE', #25457, .T. ) ;
#23528 = DIRECTION ( 'NONE',  ( -3.071710424422018668E-17, 6.404604876783312462E-16, 1.000000000000000000 ) ) ;
#23529 = ORIENTED_EDGE ( 'NONE', *, *, #48001, .F. ) ;
#23530 = CARTESIAN_POINT ( 'NONE',  ( -18.18630483459547165, -22.22016634624343467, 65.53806309781653283 ) ) ;
#23531 = CARTESIAN_POINT ( 'NONE',  ( -19.91159385759799250, -8.990409506049200417, 49.61344411288074951 ) ) ;
#23532 = CIRCLE ( 'NONE', #16443, 4.686499999999999666 ) ;
#23533 = EDGE_CURVE ( 'NONE', #46821, #2243, #43851, .T. ) ;
#23534 =( GEOMETRIC_REPRESENTATION_CONTEXT ( 3 ) GLOBAL_UNCERTAINTY_ASSIGNED_CONTEXT ( ( #42069 ) ) GLOBAL_UNIT_ASSIGNED_CONTEXT ( ( #14481, #40608, #3683 ) ) REPRESENTATION_CONTEXT ( 'NONE', 'WORKASPACE' ) );
#23535 = CARTESIAN_POINT ( 'NONE',  ( -10.32991051753928780, -12.53378322482101126, 60.93707066162556885 ) ) ;
#23536 = CARTESIAN_POINT ( 'NONE',  ( -24.32102835452959866, -16.00663571048927381, 66.36324977196242969 ) ) ;
#23537 = ORIENTED_EDGE ( 'NONE', *, *, #33662, .T. ) ;
#23538 = CARTESIAN_POINT ( 'NONE',  ( -22.06477193427564387, -8.981018767459000074, 63.23507824025425350 ) ) ;
#23539 = CARTESIAN_POINT ( 'NONE',  ( -20.89525781030762630, -21.40132374626120182, 58.78328657048043482 ) ) ;
#23540 = AXIS2_PLACEMENT_3D ( 'NONE', #29118, #24717, #40212 ) ;
#23542 = DIRECTION ( 'NONE',  ( -3.071710424422018668E-17, 6.404604876783312462E-16, 1.000000000000000000 ) ) ;
#23541 = AXIS2_PLACEMENT_3D ( 'NONE', #9253, #39286, #20815 ) ;
#23543 = FACE_BOUND ( 'NONE', #34200, .T. ) ;
#23544 = CARTESIAN_POINT ( 'NONE',  ( -11.36795091080559850, -18.31963851737709348, 58.10714594516144871 ) ) ;
#23545 = CARTESIAN_POINT ( 'NONE',  ( -14.14284385541286859, -7.587656875400065282, 49.25157356644783135 ) ) ;
#23546 = DIRECTION ( 'NONE',  ( -3.071710424422018668E-17, 6.404604876783312462E-16, 1.000000000000000000 ) ) ;
#23547 = ORIENTED_EDGE ( 'NONE', *, *, #25292, .F. ) ;
#23548 = CYLINDRICAL_SURFACE ( 'NONE', #42547, 0.1499999999999973577 ) ;
#23549 = ORIENTED_EDGE ( 'NONE', *, *, #16275, .T. ) ;
#23550 = CARTESIAN_POINT ( 'NONE',  ( -11.17634552511236734, -11.65223367170475655, 67.63367030445587602 ) ) ;
#23551 = CARTESIAN_POINT ( 'NONE',  ( -24.29232374648589854, -16.16102685949518403, 62.89328677060923667 ) ) ;
#23552 =( BOUNDED_CURVE ( )  B_SPLINE_CURVE ( 3, ( #46693, #2824, #44453, #25006 ),
 .UNSPECIFIED., .F., .F. ) 
 B_SPLINE_CURVE_WITH_KNOTS ( ( 4, 4 ),
 ( 0.9074455897393639559, 1.000000000000000000 ),
 .UNSPECIFIED. ) 
 CURVE ( )  GEOMETRIC_REPRESENTATION_ITEM ( )  RATIONAL_B_SPLINE_CURVE ( ( 0.6983129098260923984, 0.7760317562606976471, 0.8765941196520001810, 1.000000000000000000 ) ) 
 REPRESENTATION_ITEM ( '' )  );
#23553 = EDGE_CURVE ( 'NONE', #31463, #18208, #2029, .T. ) ;
#23554 = VERTEX_POINT ( 'NONE', #43010 ) ;
#23555 = DIRECTION ( 'NONE',  ( 0.8447509909909731718, -0.5351595679979654907, 0.000000000000000000 ) ) ;
#23556 = ADVANCED_FACE ( 'NONE', ( #2614 ), #13672, .T. ) ;
#23557 = FACE_BOUND ( 'NONE', #30889, .T. ) ;
#23558 = VERTEX_POINT ( 'NONE', #17618 ) ;
#23559 = EDGE_LOOP ( 'NONE', ( #35386, #11178, #24471, #3883 ) ) ;
#23560 = ORIENTED_EDGE ( 'NONE', *, *, #12476, .F. ) ;
#23561 = CARTESIAN_POINT ( 'NONE',  ( -10.44761804341386124, -15.84536169652562343, 60.92300268024614240 ) ) ;
#23562 = CARTESIAN_POINT ( 'NONE',  ( -16.25451963475149952, -21.76959929332391397, 65.36997467570328979 ) ) ;
#23563 = EDGE_CURVE ( 'NONE', #33660, #44249, #28473, .T. ) ;
#23564 = CARTESIAN_POINT ( 'NONE',  ( -17.40624601077856681, -7.359220752920395903, 67.22050788099178931 ) ) ;
#23565 = CARTESIAN_POINT ( 'NONE',  ( -13.79463883769849097, -8.760909077082668972, 57.26968041321134706 ) ) ;
#23566 = CARTESIAN_POINT ( 'NONE',  ( -12.54339362283315396, -20.43782951766612044, 72.00642459070172663 ) ) ;
#23567 =( BOUNDED_CURVE ( )  B_SPLINE_CURVE ( 3, ( #19529, #7991, #1288, #11411 ),
 .UNSPECIFIED., .F., .F. ) 
 B_SPLINE_CURVE_WITH_KNOTS ( ( 4, 4 ),
 ( 0.9074455897393722825, 1.000000000000000000 ),
 .UNSPECIFIED. ) 
 CURVE ( )  GEOMETRIC_REPRESENTATION_ITEM ( )  RATIONAL_B_SPLINE_CURVE ( ( 0.6983129098261009471, 0.7760317562607050856, 0.8765941196520047329, 1.000000000000000000 ) ) 
 REPRESENTATION_ITEM ( '' )  );
#23568 = VERTEX_POINT ( 'NONE', #39558 ) ;
#23569 = ORIENTED_EDGE ( 'NONE', *, *, #2101, .F. ) ;
#23570 = FACE_OUTER_BOUND ( 'NONE', #22993, .T. ) ;
#23571 = AXIS2_PLACEMENT_3D ( 'NONE', #32763, #13791, #3216 ) ;
#23572 = DIRECTION ( 'NONE',  ( 1.070267892916910012E-05, 6.715522048394477486E-06, -0.9999999999201771850 ) ) ;
#23573 = CARTESIAN_POINT ( 'NONE',  ( -19.74286224202880291, -21.41400126446427166, 65.65589394489410324 ) ) ;
#23574 = ORIENTED_EDGE ( 'NONE', *, *, #32860, .F. ) ;
#23575 = CARTESIAN_POINT ( 'NONE',  ( -20.64284385650552167, -8.811426318492348031, 52.18089403414751359 ) ) ;
#23576 = AXIS2_PLACEMENT_3D ( 'NONE', #32507, #28812, #43849 ) ;
#23577 = ORIENTED_EDGE ( 'NONE', *, *, #8305, .F. ) ;
#23578 = CARTESIAN_POINT ( 'NONE',  ( -14.97035482569482312, -21.41873484682592377, 61.92128389535452015 ) ) ;
#23579 = CARTESIAN_POINT ( 'NONE',  ( 10.57590614458695377, 3.140741878271517962, 50.53406581128081143 ) ) ;
#23580 = CARTESIAN_POINT ( 'NONE',  ( -17.39761409878557785, -7.809256622337199971, 67.02039592144427615 ) ) ;
#23581 = VECTOR ( 'NONE', #27350, 1000.000000000000114 ) ;
#23582 = ORIENTED_EDGE ( 'NONE', *, *, #17244, .F. ) ;
#23583 = CARTESIAN_POINT ( 'NONE',  ( -17.79084007069931417, -7.768752218527305686, 60.38060768310334225 ) ) ;
#23584 = EDGE_CURVE ( 'NONE', #44063, #46918, #5835, .T. ) ;
#23585 = CARTESIAN_POINT ( 'NONE',  ( -22.05807764791711278, -8.975638133202819446, 63.31340990608051555 ) ) ;
#23586 = CARTESIAN_POINT ( 'NONE',  ( -15.95285335075216970, -19.84884456522215146, 52.02966884056656482 ) ) ;
#23587 = EDGE_CURVE ( 'NONE', #23075, #5574, #36117, .T. ) ;
#23588 = ORIENTED_EDGE ( 'NONE', *, *, #5232, .T. ) ;
#23589 = B_SPLINE_CURVE_WITH_KNOTS ( 'NONE', 1,
 ( #19076, #11440 ),
 .UNSPECIFIED., .F., .F.,
 ( 2, 2 ),
 ( 0.000000000000000000, 1.000000000000000000 ),
 .UNSPECIFIED. ) ;
#23590 = LINE ( 'NONE', #12017, #19446 ) ;
#23591 = CARTESIAN_POINT ( 'NONE',  ( -24.82475127085388422, -15.66597259679895693, 73.11808347143848152 ) ) ;
#23592 = DIRECTION ( 'NONE',  ( -3.071710424422018668E-17, 6.404604876783312462E-16, 1.000000000000000000 ) ) ;
#23593 = EDGE_LOOP ( 'NONE', ( #6529, #11082, #28128, #26672 ) ) ;
#23594 = CARTESIAN_POINT ( 'NONE',  ( -15.98090817348981751, -7.500318407754576810, 63.86999797141741908 ) ) ;
#23595 = EDGE_LOOP ( 'NONE', ( #26478, #41858, #6077, #23825, #19141 ) ) ;
#23596 = DIRECTION ( 'NONE',  ( 0.3688590060343580612, -0.9294853595766560117, 0.000000000000000000 ) ) ;
#23597 = CARTESIAN_POINT ( 'NONE',  ( -24.72409385541305582, -14.80920654474412679, 59.91176470588234793 ) ) ;
#23598 = ORIENTED_EDGE ( 'NONE', *, *, #28165, .F. ) ;
#23599 = CARTESIAN_POINT ( 'NONE',  ( -16.45566506110110083, -21.79267588865899086, 62.04095995016087528 ) ) ;
#23600 = CARTESIAN_POINT ( 'NONE',  ( -24.14679772577363437, -12.68507108172156883, 70.05770892828130059 ) ) ;
#23601 = CARTESIAN_POINT ( 'NONE',  ( -15.39536932222403287, -19.92137602241599836, 53.49999999999995026 ) ) ;
#23602 = VECTOR ( 'NONE', #19948, 1000.000000000000000 ) ;
#23603 = ORIENTED_EDGE ( 'NONE', *, *, #6200, .T. ) ;
#23604 = CARTESIAN_POINT ( 'NONE',  ( -10.57723003925373106, -17.74759380694297306, 71.75373442408677249 ) ) ;
#23605 = CIRCLE ( 'NONE', #8782, 1.250000000000001110 ) ;
#23606 = CARTESIAN_POINT ( 'NONE',  ( -15.15158015243114953, -21.90415461596747448, 68.77604118143560186 ) ) ;
#23607 = DIRECTION ( 'NONE',  ( 1.000000000000000000, 2.866981220435666553E-17, 0.000000000000000000 ) ) ;
#23609 = EDGE_CURVE ( 'NONE', #48232, #47529, #40759, .T. ) ;
#23608 = CARTESIAN_POINT ( 'NONE',  ( -17.42409385541299471, -14.80920654474435771, 49.52966884056655772 ) ) ;
#23610 = ORIENTED_EDGE ( 'NONE', *, *, #45395, .F. ) ;
#23611 = B_SPLINE_CURVE_WITH_KNOTS ( 'NONE', 1,
 ( #44302, #6129 ),
 .UNSPECIFIED., .F., .F.,
 ( 2, 2 ),
 ( 0.000000000000000000, 1.000000000000000000 ),
 .UNSPECIFIED. ) ;
#23612 = CARTESIAN_POINT ( 'NONE',  ( -10.64577744754535082, -11.71757184301072563, 74.67344733366148546 ) ) ;
#23613 = VECTOR ( 'NONE', #13225, 1000.000000000000000 ) ;
#23614 = EDGE_CURVE ( 'NONE', #596, #19379, #45575, .T. ) ;
#23615 = LINE ( 'NONE', #16437, #19628 ) ;
#23616 = ADVANCED_FACE ( 'NONE', ( #48637 ), #14877, .T. ) ;
#23617 = ADVANCED_FACE ( 'NONE', ( #37291 ), #26480, .T. ) ;
#23618 = EDGE_CURVE ( 'NONE', #31116, #8437, #5631, .T. ) ;
#23619 = EDGE_LOOP ( 'NONE', ( #26047, #8974, #645, #22116 ) ) ;
#23620 = EDGE_LOOP ( 'NONE', ( #5901, #1551, #3891, #16980 ) ) ;
#23621 = CARTESIAN_POINT ( 'NONE',  ( -22.85634303820408064, -10.39183521286026490, 66.73109339323789868 ) ) ;
#23622 = CARTESIAN_POINT ( 'NONE',  ( -11.16720021946830421, -11.56054808309503379, 67.91864607954204303 ) ) ;
#23623 = CARTESIAN_POINT ( 'NONE',  ( -10.42732927881409388, -14.54885027197008185, 71.51709673969678249 ) ) ;
#23624 = VECTOR ( 'NONE', #47502, 1000.000000000000000 ) ;
#23625 = CARTESIAN_POINT ( 'NONE',  ( -21.45534385650551812, -7.417179338643134834, 52.18511593390279302 ) ) ;
#23626 = DIRECTION ( 'NONE',  ( -0.9729319276368275649, -0.2310918955413239495, 6.827553174175006206E-08 ) ) ;
#23627 = DIRECTION ( 'NONE',  ( -3.071710424422018668E-17, 6.404604876783312462E-16, 1.000000000000000000 ) ) ;
#23628 = CARTESIAN_POINT ( 'NONE',  ( -23.22139472215082279, -18.73524832941601304, 69.48299170654385648 ) ) ;
#23629 = CARTESIAN_POINT ( 'NONE',  ( -11.03230881600246427, -10.98182333549695322, 60.79390388117851529 ) ) ;
#23630 = EDGE_LOOP ( 'NONE', ( #7077, #36264, #6801, #13498, #4429 ) ) ;
#23631 = ORIENTED_EDGE ( 'NONE', *, *, #19563, .F. ) ;
#23632 = CARTESIAN_POINT ( 'NONE',  ( -12.37147782024668707, -20.28402873453449828, 68.53668635025047706 ) ) ;
#23633 = CYLINDRICAL_SURFACE ( 'NONE', #18085, 1.249999999999998668 ) ;
#23634 = B_SPLINE_CURVE_WITH_KNOTS ( 'NONE', 3,
 ( #26376, #44866, #3982, #18994, #15273, #33997, #26882, #37940, #29839, #7196 ),
 .UNSPECIFIED., .F., .F.,
 ( 4, 2, 2, 2, 4 ),
 ( 0.1272669073658881933, 0.2522669073463699174, 0.3772669073268516970, 0.5022669073073334767, 0.6272669072878152008 ),
 .UNSPECIFIED. ) ;
#23635 = FACE_OUTER_BOUND ( 'NONE', #42358, .T. ) ;
#23636 = DIRECTION ( 'NONE',  ( -0.8603395911234870130, -0.5097212845717461471, 0.000000000000000000 ) ) ;
#23637 = ORIENTED_EDGE ( 'NONE', *, *, #17429, .T. ) ;
#23638 = ORIENTED_EDGE ( 'NONE', *, *, #21648, .F. ) ;
#23639 = EDGE_CURVE ( 'NONE', #7665, #39283, #47810, .T. ) ;
#23640 = FACE_OUTER_BOUND ( 'NONE', #19626, .T. ) ;
#23641 = CARTESIAN_POINT ( 'NONE',  ( -10.34343347544818847, -12.28147837111555774, 54.02312124697528617 ) ) ;
#23642 = AXIS2_PLACEMENT_3D ( 'NONE', #29571, #10856, #40895 ) ;
#23643 = CARTESIAN_POINT ( 'NONE',  ( -18.68070144837527735, -7.415226739706411330, 54.27966884056654351 ) ) ;
#23644 = CARTESIAN_POINT ( 'NONE',  ( -11.06345430940418417, -18.68820014949154640, 61.45523615231426362 ) ) ;
#23645 = ORIENTED_EDGE ( 'NONE', *, *, #7381, .T. ) ;
#23646 = VECTOR ( 'NONE', #46527, 1000.000000000000000 ) ;
#23647 = CARTESIAN_POINT ( 'NONE',  ( -24.85359104829803911, -14.25571788259268402, 69.76779960783916579 ) ) ;
#23648 = CARTESIAN_POINT ( 'NONE',  ( -17.42409385541300892, -14.80920654474439502, 77.49999999999994316 ) ) ;
#23649 = ORIENTED_EDGE ( 'NONE', *, *, #38846, .F. ) ;
#23650 = EDGE_CURVE ( 'NONE', #47561, #32087, #4924, .T. ) ;
#23651 = CARTESIAN_POINT ( 'NONE',  ( -14.98249323814573941, -9.880861343182303358, 53.49999999999995026 ) ) ;
#23652 = B_SPLINE_CURVE_WITH_KNOTS ( 'NONE', 3,
 ( #28746, #43776, #10034, #40073, #21605, #25057, #6340, #17878, #32902, #14177 ),
 .UNSPECIFIED., .F., .F.,
 ( 4, 2, 2, 2, 4 ),
 ( 0.6272669072877726792, 0.7522669073072767443, 0.8772669073267809203, 1.002266907346284874, 1.127266907365789050 ),
 .UNSPECIFIED. ) ;
#23653 = CARTESIAN_POINT ( 'NONE',  ( -23.65624057141237202, -11.51332318074561911, 66.72214514605295221 ) ) ;
#23654 = ORIENTED_EDGE ( 'NONE', *, *, #31718, .T. ) ;
#23655 = DIRECTION ( 'NONE',  ( 0.9375570856950864451, -0.3478314405900309603, 3.549360974553817487E-17 ) ) ;
#23656 = EDGE_LOOP ( 'NONE', ( #20195, #34890, #36865, #6823 ) ) ;
#23657 = DIRECTION ( 'NONE',  ( -0.8949343913984795229, -0.4461977533473618918, 4.967883834297468681E-17 ) ) ;
#23658 = CYLINDRICAL_SURFACE ( 'NONE', #25801, 0.1499999999999949984 ) ;
#23659 = EDGE_LOOP ( 'NONE', ( #4851, #33493, #47415, #21000, #28366 ) ) ;
#23660 = CARTESIAN_POINT ( 'NONE',  ( -24.20836943865575464, -17.88934756284849215, 62.66016244028183024 ) ) ;
#23661 = CARTESIAN_POINT ( 'NONE',  ( -18.39792479006713677, -22.19536379348757293, 68.85868763382491409 ) ) ;
#23662 = CARTESIAN_POINT ( 'NONE',  ( -18.61784385650552309, -9.790100578890868377, 49.79778022625163203 ) ) ;
#23663 = CARTESIAN_POINT ( 'NONE',  ( -15.12736151640637416, -21.89643440865206614, 68.69097607374993686 ) ) ;
#23664 = CARTESIAN_POINT ( 'NONE',  ( -13.92409385541305511, -10.10920654474410618, 78.99999999999998579 ) ) ;
#23665 = B_SPLINE_CURVE_WITH_KNOTS ( 'NONE', 3,
 ( #29834, #11117, #17991, #17747, #37183, #32546, #14515, #10146, #26138, #3469 ),
 .UNSPECIFIED., .F., .F.,
 ( 4, 2, 2, 2, 4 ),
 ( 0.1272669073658366790, 0.2522669073463276179, 0.3772669073268185014, 0.5022669073073093848, 0.6272669072878003238 ),
 .UNSPECIFIED. ) ;
#23666 = CARTESIAN_POINT ( 'NONE',  ( -14.79906637807316550, -21.78150152883456059, 61.67954536979805624 ) ) ;
#23667 = ORIENTED_EDGE ( 'NONE', *, *, #13742, .F. ) ;
#23668 = CARTESIAN_POINT ( 'NONE',  ( -33.42409385541304800, -9.359200813967566646, 50.49621490985803263 ) ) ;
#23669 = FACE_OUTER_BOUND ( 'NONE', #48586, .T. ) ;
#23670 = CARTESIAN_POINT ( 'NONE',  ( -15.54909385541290590, -8.112991634885938552, 51.74999426922445878 ) ) ;
#23671 = CARTESIAN_POINT ( 'NONE',  ( -20.55284450191522083, -8.048022495885772898, 66.88129830338009185 ) ) ;
#23672 = AXIS2_PLACEMENT_3D ( 'NONE', #10713, #3566, #18570 ) ;
#23673 = CARTESIAN_POINT ( 'NONE',  ( -13.17078218117215549, -9.186392337449538203, 67.39414915108072535 ) ) ;
#23674 = ADVANCED_FACE ( 'NONE', ( #47918 ), #48153, .F. ) ;
#23675 = EDGE_CURVE ( 'NONE', #5852, #486, #39004, .T. ) ;
#23676 = ORIENTED_EDGE ( 'NONE', *, *, #31436, .F. ) ;
#23677 = ORIENTED_EDGE ( 'NONE', *, *, #35548, .F. ) ;
#23678 = VECTOR ( 'NONE', #18365, 1000.000000000000114 ) ;
#23679 = CARTESIAN_POINT ( 'NONE',  ( -18.55957040452605611, -7.446158924837727788, 74.02559677774105751 ) ) ;
#23680 = CARTESIAN_POINT ( 'NONE',  ( -10.33431723597471930, -12.52035407725662886, 60.98348989824278732 ) ) ;
#23681 = ORIENTED_EDGE ( 'NONE', *, *, #5733, .F. ) ;
#23682 = CARTESIAN_POINT ( 'NONE',  ( -22.48430662296557614, -20.27711519517875516, 65.81926411519917508 ) ) ;
#23683 = CARTESIAN_POINT ( 'NONE',  ( -16.30515107485298998, -22.17475187132452064, 61.86293996623023617 ) ) ;
#23684 = CARTESIAN_POINT ( 'NONE',  ( -21.76784385759799179, -9.357632978295830739, 49.97845033065684106 ) ) ;
#23685 = LINE ( 'NONE', #22961, #19512 ) ;
#23686 = CARTESIAN_POINT ( 'NONE',  ( -21.60978650687268754, -20.97240088203421493, 72.66299873415312049 ) ) ;
#23687 = CARTESIAN_POINT ( 'NONE',  ( -11.32469144785209103, -18.34471071427194389, 57.80714594245691273 ) ) ;
#23688 = AXIS2_PLACEMENT_3D ( 'NONE', #25449, #35553, #36027 ) ;
#23689 = CARTESIAN_POINT ( 'NONE',  ( -23.59327504554355315, -11.39630409041826198, 69.90682860766239060 ) ) ;
#23690 = ORIENTED_EDGE ( 'NONE', *, *, #4845, .T. ) ;
#23691 = EDGE_CURVE ( 'NONE', #12198, #26955, #12342, .T. ) ;
#23692 = PRODUCT ( 'MAS-175', 'MAS-175', '', ( #23295 ) ) ;
#23693 = EDGE_CURVE ( 'NONE', #42299, #42753, #11772, .T. ) ;
#23694 = B_SPLINE_CURVE_WITH_KNOTS ( 'NONE', 3,
 ( #34288, #38964, #41941, #818, #12622, #15568, #573, #42677, #37988, #8942 ),
 .UNSPECIFIED., .F., .F.,
 ( 4, 2, 2, 2, 4 ),
 ( 0.1272669073658150296, 0.2522669073463081890, 0.3772669073268013484, 0.5022669073072945078, 0.6272669072877876673 ),
 .UNSPECIFIED. ) ;
#23695 = CARTESIAN_POINT ( 'NONE',  ( -20.42942694929465119, -8.423054519096806914, 59.99692253513481432 ) ) ;
#23696 = CARTESIAN_POINT ( 'NONE',  ( -17.83128375312269753, -10.14042954887026049, 49.52966884056655772 ) ) ;
#23697 = AXIS2_PLACEMENT_3D ( 'NONE', #11146, #19257, #7219 ) ;
#23698 = CARTESIAN_POINT ( 'NONE',  ( -22.88264614489240856, -10.34704276773305764, 63.35713876973677827 ) ) ;
#23699 = DIRECTION ( 'NONE',  ( -0.4846961512978548714, -0.8746825943832684525, -4.196010045124609427E-08 ) ) ;
#23700 = DIRECTION ( 'NONE',  ( 0.000000000000000000, 0.000000000000000000, 1.000000000000000000 ) ) ;
#23701 =( BOUNDED_SURFACE ( )  B_SPLINE_SURFACE ( 3, 1, ( 
 ( #40201, #5755 ),
 ( #47360, #43909 ),
 ( #24469, #47105 ),
 ( #1803, #39473 ),
 ( #13824, #16802 ),
 ( #29108, #10162 ),
 ( #24936, #21492 ) ),
 .UNSPECIFIED., .T., .F., .F. ) 
 B_SPLINE_SURFACE_WITH_KNOTS ( ( 4, 3, 4 ),
 ( 2, 2 ),
 ( 0.000000000000000000, 0.5000000000000000000, 1.000000000000000000 ),
 ( 0.000000000000000000, 1.000000000000000000 ),
 .UNSPECIFIED. ) 
 GEOMETRIC_REPRESENTATION_ITEM ( )  RATIONAL_B_SPLINE_SURFACE ( (
 ( 1.000000000000000000, 1.000000000000000000),
 ( 0.3333333333333335369, 0.3333333333333330373),
 ( 0.3333333333333335369, 0.3333333333333330373),
 ( 1.000000000000000000, 1.000000000000000000),
 ( 0.3333333333333333703, 0.3333333333333333703),
 ( 0.3333333333333333703, 0.3333333333333333703),
 ( 1.000000000000000000, 1.000000000000000000) ) ) 
 REPRESENTATION_ITEM ( '' )  SURFACE ( )  );
#23702 = ORIENTED_EDGE ( 'NONE', *, *, #17958, .F. ) ;
#23703 = ORIENTED_EDGE ( 'NONE', *, *, #43918, .T. ) ;
#23704 = CARTESIAN_POINT ( 'NONE',  ( -21.90534385650552096, -8.801233750844183135, 48.81488406609782515 ) ) ;
#23705 = ORIENTED_EDGE ( 'NONE', *, *, #12278, .F. ) ;
#23706 = EDGE_CURVE ( 'NONE', #575, #34661, #1409, .T. ) ;
#23707 = CARTESIAN_POINT ( 'NONE',  ( -23.42409385541304090, -9.359200813967568422, 50.49621490985803263 ) ) ;
#23708 = VECTOR ( 'NONE', #36811, 1000.000000000000000 ) ;
#23709 = CYLINDRICAL_SURFACE ( 'NONE', #35470, 0.1500000000000015488 ) ;
#23710 = ORIENTED_EDGE ( 'NONE', *, *, #2653, .T. ) ;
#23711 =( BOUNDED_CURVE ( )  B_SPLINE_CURVE ( 3, ( #34093, #4086, #45694, #15614 ),
 .UNSPECIFIED., .F., .F. ) 
 B_SPLINE_CURVE_WITH_KNOTS ( ( 4, 4 ),
 ( 0.000000000000000000, 0.4074455897393659543 ),
 .UNSPECIFIED. ) 
 CURVE ( )  GEOMETRIC_REPRESENTATION_ITEM ( )  RATIONAL_B_SPLINE_CURVE ( ( 1.000000000000000000, 0.4567392136813356873, 0.3561768502900316546, 0.6983129098260879575 ) ) 
 REPRESENTATION_ITEM ( '' )  );
#23712 = CARTESIAN_POINT ( 'NONE',  ( -10.83529129721023487, -11.33175171474136533, 67.75831252372202584 ) ) ;
#23713 = AXIS2_PLACEMENT_3D ( 'NONE', #32637, #29672, #10963 ) ;
#23714 = ORIENTED_EDGE ( 'NONE', *, *, #20670, .T. ) ;
#23715 = AXIS2_PLACEMENT_3D ( 'NONE', #47215, #36580, #2865 ) ;
#23716 = CARTESIAN_POINT ( 'NONE',  ( -20.92219709818629170, -8.231526085280929550, 60.04136453195106782 ) ) ;
#23717 = FACE_OUTER_BOUND ( 'NONE', #45606, .T. ) ;
#23718 = ORIENTED_EDGE ( 'NONE', *, *, #33650, .F. ) ;
#23719 = FACE_OUTER_BOUND ( 'NONE', #18653, .T. ) ;
#23720 = AXIS2_PLACEMENT_3D ( 'NONE', #8263, #1591, #23281 ) ;
#23721 = CARTESIAN_POINT ( 'NONE',  ( -10.12326195556307695, -13.32541703369907893, 74.86313051124790263 ) ) ;
#23722 =( BOUNDED_CURVE ( )  B_SPLINE_CURVE ( 3, ( #4809, #15621, #11959, #12673 ),
 .UNSPECIFIED., .F., .T. ) 
 B_SPLINE_CURVE_WITH_KNOTS ( ( 4, 4 ),
 ( 0.4074455897393560178, 0.5000000000000000000 ),
 .UNSPECIFIED. ) 
 CURVE ( )  GEOMETRIC_REPRESENTATION_ITEM ( )  RATIONAL_B_SPLINE_CURVE ( ( 0.6983129098260760781, 0.7760317562606792174, 0.8765941196519858591, 0.9999999999999930056 ) ) 
 REPRESENTATION_ITEM ( '' )  );
#23723 = VERTEX_POINT ( 'NONE', #26733 ) ;
#23724 = CARTESIAN_POINT ( 'NONE',  ( -10.38078070663892660, -14.50222156296673148, 67.85800126083267969 ) ) ;
#23725 = CARTESIAN_POINT ( 'NONE',  ( -12.41310947992116098, -19.76871611099698001, 61.68206578716802113 ) ) ;
#23726 = CARTESIAN_POINT ( 'NONE',  ( -18.75796263175485734, -7.882761566875607251, 74.14064681633755072 ) ) ;
#23727 = ORIENTED_EDGE ( 'NONE', *, *, #14735, .F. ) ;
#23728 = DIRECTION ( 'NONE',  ( 0.9687793358424822143, -0.2479245821708672415, 0.000000000000000000 ) ) ;
#23729 = CARTESIAN_POINT ( 'NONE',  ( -21.99213670719075253, -20.17946569659695655, 59.04970794435396897 ) ) ;
#23730 = AXIS2_PLACEMENT_3D ( 'NONE', #47377, #36270, #25445 ) ;
#23731 = DIRECTION ( 'NONE',  ( 6.374839753205896285E-22, 0.007114381193220334181, -0.9999746924698833528 ) ) ;
#23732 = CARTESIAN_POINT ( 'NONE',  ( -24.37533454541335232, -13.98391229038511163, 73.40806141292473797 ) ) ;
#23733 = DIRECTION ( 'NONE',  ( -0.7971031148784508691, 0.6038432116460915600, -6.916509187980531058E-08 ) ) ;
#23734 = DIRECTION ( 'NONE',  ( 1.224646799147353207E-16, 1.000000000000000000, -1.912410701131276611E-32 ) ) ;
#23735 = LINE ( 'NONE', #38729, #47983 ) ;
#23736 = CARTESIAN_POINT ( 'NONE',  ( -15.88659385650551670, -9.302874398569244363, 51.68646062012417985 ) ) ;
#23737 = ADVANCED_FACE ( 'NONE', ( #4557 ), #34586, .F. ) ;
#23738 = VECTOR ( 'NONE', #39693, 1000.000000000000000 ) ;
#23739 = ORIENTED_EDGE ( 'NONE', *, *, #27796, .T. ) ;
#23740 = FACE_OUTER_BOUND ( 'NONE', #33696, .T. ) ;
#23741 = CARTESIAN_POINT ( 'NONE',  ( -27.42409385541305511, -15.80920654474410725, 56.99999999999999289 ) ) ;
#23742 = ORIENTED_EDGE ( 'NONE', *, *, #23693, .T. ) ;
#23743 = CARTESIAN_POINT ( 'NONE',  ( -20.60942684424193416, -21.09890871138989965, 58.65947248567252359 ) ) ;
#23744 = CARTESIAN_POINT ( 'NONE',  ( -14.54749350918765671, -8.372447261038937327, 64.07506791522041567 ) ) ;
#23745 = LINE ( 'NONE', #38738, #23158 ) ;
#23746 = CARTESIAN_POINT ( 'NONE',  ( -12.71429358501400131, -19.98796095756949143, 68.33657440636297054 ) ) ;
#23747 = FACE_OUTER_BOUND ( 'NONE', #28528, .T. ) ;
#23748 = VERTEX_POINT ( 'NONE', #11704 ) ;
#23749 = CARTESIAN_POINT ( 'NONE',  ( -24.79887126163464828, -15.86559147609933618, 69.64033351364996349 ) ) ;
#23750 = CARTESIAN_POINT ( 'NONE',  ( -17.22364295584634775, -7.762016434835315337, 70.49035836927656362 ) ) ;
#23751 = EDGE_CURVE ( 'NONE', #30534, #24642, #45448, .T. ) ;
#23752 = AXIS2_PLACEMENT_3D ( 'NONE', #21572, #36795, #36551 ) ;
#23753 = CARTESIAN_POINT ( 'NONE',  ( -10.09142662841313332, -16.12648724910785702, 68.08429501313727883 ) ) ;
#23754 = EDGE_LOOP ( 'NONE', ( #41646, #28857, #19403, #13044, #42883 ) ) ;
#23755 = CARTESIAN_POINT ( 'NONE',  ( -17.13503149044196405, -7.764836982087095052, 70.77563787455143540 ) ) ;
#23756 = ADVANCED_FACE ( 'NONE', ( #15872 ), #8758, .T. ) ;
#23757 = VECTOR ( 'NONE', #29168, 1000.000000000000000 ) ;
#23758 = EDGE_CURVE ( 'NONE', #36333, #48460, #21863, .T. ) ;
#23759 = CARTESIAN_POINT ( 'NONE',  ( -23.91632973644556159, -12.05317525496800357, 59.89724340139424896 ) ) ;
#23760 = DIRECTION ( 'NONE',  ( -2.866981220435666553E-17, 1.000000000000000000, 1.190614954331866791E-16 ) ) ;
#23761 = CARTESIAN_POINT ( 'NONE',  ( -11.08846142298070880, -18.82290330472913098, 53.49999999999994316 ) ) ;
#23762 = EDGE_LOOP ( 'NONE', ( #44644, #25526 ) ) ;
#23763 = ORIENTED_EDGE ( 'NONE', *, *, #2089, .T. ) ;
#23764 = CARTESIAN_POINT ( 'NONE',  ( -20.83659385541304232, -8.995762431863214559, 51.38120296130585274 ) ) ;
#23765 = AXIS2_PLACEMENT_3D ( 'NONE', #43689, #12660, #39005 ) ;
#23766 = DIRECTION ( 'NONE',  ( 0.9687793358424819923, -0.2479245821708678243, 0.000000000000000000 ) ) ;
#23767 = CARTESIAN_POINT ( 'NONE',  ( -21.02205230129062485, -8.737166911425223503, 59.98558246646761916 ) ) ;
#23768 = DIRECTION ( 'NONE',  ( 0.8603613874411334406, -0.3191920208248665292, 0.3973597071195140162 ) ) ;
#23769 = CARTESIAN_POINT ( 'NONE',  ( -24.46356860818091405, -14.42337734487177947, 66.48292728742831059 ) ) ;
#23770 = ORIENTED_EDGE ( 'NONE', *, *, #92, .F. ) ;
#23771 = CARTESIAN_POINT ( 'NONE',  ( -24.17969144601942233, -17.95015662838525117, 59.04732501252154009 ) ) ;
#23772 = CARTESIAN_POINT ( 'NONE',  ( -24.72409385541305582, -14.80920654474413745, 60.01764705882352047 ) ) ;
#23773 = EDGE_LOOP ( 'NONE', ( #21869, #28064, #10755, #39523, #41233 ) ) ;
#23774 = CARTESIAN_POINT ( 'NONE',  ( -10.33531692083374587, -17.10115316349580894, 57.87255846826901262 ) ) ;
#23775 = DIRECTION ( 'NONE',  ( -0.1675476790616295397, 0.9858639740050658684, -1.006000811662239041E-16 ) ) ;
#23776 = ORIENTED_EDGE ( 'NONE', *, *, #17576, .T. ) ;
#23777 = CARTESIAN_POINT ( 'NONE',  ( -10.34546495671637700, -12.48638223296730487, 60.94853567734574540 ) ) ;
#23778 = AXIS2_PLACEMENT_3D ( 'NONE', #6484, #33036, #9931 ) ;
#23779 = EDGE_CURVE ( 'NONE', #47586, #19229, #46420, .T. ) ;
#23780 = CARTESIAN_POINT ( 'NONE',  ( -10.00117625416208433, -15.44487358686203571, 57.68297391752145842 ) ) ;
#23781 = DIRECTION ( 'NONE',  ( -0.000000000000000000, 1.000000000000000000, -0.000000000000000000 ) ) ;
#23782 = ORIENTED_EDGE ( 'NONE', *, *, #18531, .T. ) ;
#23783 = DIRECTION ( 'NONE',  ( 0.000000000000000000, -1.000000000000000000, 0.000000000000000000 ) ) ;
#23784 = CARTESIAN_POINT ( 'NONE',  ( -20.88891245741970693, -21.40461089374386461, 58.76662411742747594 ) ) ;
#23785 = CARTESIAN_POINT ( 'NONE',  ( -23.80941655268207668, -18.64734661885979961, 72.80722282987319716 ) ) ;
#23786 = FACE_OUTER_BOUND ( 'NONE', #30744, .T. ) ;
#23787 = APPLICATION_PROTOCOL_DEFINITION ( 'draft international standard', 'automotive_design', 1998, #8652 ) ;
#23788 = CARTESIAN_POINT ( 'NONE',  ( -14.22441497990486958, -8.081217732231424478, 67.44470516081543110 ) ) ;
#23789 = CARTESIAN_POINT ( 'NONE',  ( -17.19167086870822203, -7.760035283349824731, 66.90551000485606892 ) ) ;
#23790 = CARTESIAN_POINT ( 'NONE',  ( -24.39763799706551950, -15.84669482609578317, 69.54779622430706354 ) ) ;
#23791 = ORIENTED_EDGE ( 'NONE', *, *, #31104, .F. ) ;
#23792 = LINE ( 'NONE', #11980, #6401 ) ;
#23793 =( BOUNDED_CURVE ( )  B_SPLINE_CURVE ( 3, ( #16771, #1522, #42421, #8691 ),
 .UNSPECIFIED., .F., .F. ) 
 B_SPLINE_CURVE_WITH_KNOTS ( ( 4, 4 ),
 ( 0.5000000000000000000, 0.9074455897393663983 ),
 .UNSPECIFIED. ) 
 CURVE ( )  GEOMETRIC_REPRESENTATION_ITEM ( )  RATIONAL_B_SPLINE_CURVE ( ( 1.000000000000007994, 0.4567392136813297476, 0.3561768502900237165, 0.6983129098260987266 ) ) 
 REPRESENTATION_ITEM ( '' )  );
#23794 = VERTEX_POINT ( 'NONE', #19833 ) ;
#23795 = CARTESIAN_POINT ( 'NONE',  ( -21.52726260838264949, -9.076274878514672295, 70.13132538915753855 ) ) ;
#23796 = LINE ( 'NONE', #5078, #726 ) ;
#23797 = ORIENTED_EDGE ( 'NONE', *, *, #41449, .F. ) ;
#23798 = B_SPLINE_CURVE_WITH_KNOTS ( 'NONE', 3,
 ( #2895, #6607, #40816, #25324, #40102, #10779, #47722, #25799, #25553, #44057 ),
 .UNSPECIFIED., .F., .F.,
 ( 4, 2, 2, 2, 4 ),
 ( 0.000000000000000000, 0.2500000000000000000, 0.5000000000000000000, 0.7500000000000000000, 1.000000000000000000 ),
 .UNSPECIFIED. ) ;
#23799 = PLANE ( 'NONE',  #16907 ) ;
#23800 = FACE_BOUND ( 'NONE', #8651, .T. ) ;
#23801 = ORIENTED_EDGE ( 'NONE', *, *, #4122, .F. ) ;
#23802 = ORIENTED_EDGE ( 'NONE', *, *, #38164, .F. ) ;
#23803 = VERTEX_POINT ( 'NONE', #34832 ) ;
#23804 = EDGE_CURVE ( 'NONE', #16133, #8440, #23722, .T. ) ;
#23805 = CARTESIAN_POINT ( 'NONE',  ( 18.07590614458695200, 1.637417875877629436, 51.62951866002712364 ) ) ;
#23806 = CARTESIAN_POINT ( 'NONE',  ( -21.68034385541343312, -9.360768649636696637, 51.01397948906189583 ) ) ;
#23807 = EDGE_CURVE ( 'NONE', #19706, #40467, #45930, .T. ) ;
#23808 = FACE_OUTER_BOUND ( 'NONE', #32578, .T. ) ;
#23809 = CARTESIAN_POINT ( 'NONE',  ( -14.51896091561126489, -8.440036020032167130, 67.54358485890664099 ) ) ;
#23810 = CARTESIAN_POINT ( 'NONE',  ( -12.68381401182790569, -19.95991009262169413, 68.33657438305763776 ) ) ;
#23811 = CARTESIAN_POINT ( 'NONE',  ( -10.74141550158114455, -16.89327759150595654, 57.98760574264920109 ) ) ;
#23812 = ORIENTED_EDGE ( 'NONE', *, *, #20874, .T. ) ;
#23813 = VERTEX_POINT ( 'NONE', #31142 ) ;
#23814 = EDGE_CURVE ( 'NONE', #28527, #28606, #19089, .T. ) ;
#23815 = CARTESIAN_POINT ( 'NONE',  ( -22.10534385650551670, -8.801233750844183135, 48.81488406609782515 ) ) ;
#23816 = CARTESIAN_POINT ( 'NONE',  ( -21.59671027634132656, -20.98115415594247324, 72.56800473755950520 ) ) ;
#23817 = CARTESIAN_POINT ( 'NONE',  ( -12.64995480627295521, -19.99670077279894898, 68.48657438322858582 ) ) ;
#23818 = CARTESIAN_POINT ( 'NONE',  ( -21.60699152411756074, -9.194825043480776117, 70.35962493737054047 ) ) ;
#23819 = ORIENTED_EDGE ( 'NONE', *, *, #15829, .F. ) ;
#23820 = EDGE_CURVE ( 'NONE', #35582, #24088, #18403, .T. ) ;
#23821 = CARTESIAN_POINT ( 'NONE',  ( -22.44284385650551528, -8.811426318492348031, 52.18089403414751359 ) ) ;
#23822 = ORIENTED_EDGE ( 'NONE', *, *, #30640, .T. ) ;
#23823 = CARTESIAN_POINT ( 'NONE',  ( -23.05110005139504636, -10.64472189410646230, 59.61820115093192385 ) ) ;
#23824 = CARTESIAN_POINT ( 'NONE',  ( -12.48641702280725951, -19.77161301655056036, 64.88291470187951404 ) ) ;
#23825 = ORIENTED_EDGE ( 'NONE', *, *, #11737, .T. ) ;
#23826 = CARTESIAN_POINT ( 'NONE',  ( -11.63855442814814367, -18.75048355864383609, 68.50073137068018525 ) ) ;
#23827 = B_SPLINE_CURVE_WITH_KNOTS ( 'NONE', 3,
 ( #41855, #8130, #4413, #19433, #34438, #31974, #27556, #23875, #9819, #35417 ),
 .UNSPECIFIED., .F., .F.,
 ( 4, 2, 2, 2, 4 ),
 ( 0.6272669072878033214, 0.7522669073073137147, 0.8772669073268239970, 1.002266907346334390, 1.127266907365844784 ),
 .UNSPECIFIED. ) ;
#23828 = CARTESIAN_POINT ( 'NONE',  ( -10.78898398081525301, -17.19290454168847404, 61.44271037915215317 ) ) ;
#23829 = CARTESIAN_POINT ( 'NONE',  ( -10.42774853574490201, -14.58114972691745947, 68.14334793592969675 ) ) ;
#23830 = FACE_OUTER_BOUND ( 'NONE', #45018, .T. ) ;
#23831 = VERTEX_POINT ( 'NONE', #31641 ) ;
#23832 = CARTESIAN_POINT ( 'NONE',  ( -15.97284114023201695, -21.71201116376809992, 58.58585868367167393 ) ) ;
#23833 =( BOUNDED_CURVE ( )  B_SPLINE_CURVE ( 3, ( #5565, #35576, #890, #8515 ),
 .UNSPECIFIED., .F., .F. ) 
 B_SPLINE_CURVE_WITH_KNOTS ( ( 4, 4 ),
 ( -7.993605777301127091E-15, 0.2013579207903272439 ),
 .UNSPECIFIED. ) 
 CURVE ( )  GEOMETRIC_REPRESENTATION_ITEM ( )  RATIONAL_B_SPLINE_CURVE ( ( 1.000000000000000000, 0.9966241020034157794, 0.9966241020034157794, 1.000000000000000000 ) ) 
 REPRESENTATION_ITEM ( '' )  );
#23834 = EDGE_CURVE ( 'NONE', #38000, #28514, #28968, .T. ) ;
#23835 = CARTESIAN_POINT ( 'NONE',  ( -17.46222794319647775, -7.759011850482251837, 67.03511641684839617 ) ) ;
#23836 = CARTESIAN_POINT ( 'NONE',  ( -20.10974094956083746, -7.859941204851112140, 73.85950125338895589 ) ) ;
#23837 = ORIENTED_EDGE ( 'NONE', *, *, #17489, .T. ) ;
#23838 = PLANE ( 'NONE',  #44065 ) ;
#23839 = ORIENTED_EDGE ( 'NONE', *, *, #32412, .F. ) ;
#23840 = CARTESIAN_POINT ( 'NONE',  ( -19.22059177161013110, -7.579041592493069857, 63.53114993777460029 ) ) ;
#23841 = CARTESIAN_POINT ( 'NONE',  ( -14.65746096889331263, -8.316078616448901784, 57.00567256703398300 ) ) ;
#23842 = ORIENTED_EDGE ( 'NONE', *, *, #21154, .T. ) ;
#23843 = DIRECTION ( 'NONE',  ( 0.9687793358424821033, -0.2479245821708677133, 0.000000000000000000 ) ) ;
#23844 = CARTESIAN_POINT ( 'NONE',  ( -24.64680953583212286, -12.98235456786829367, 62.99297500150433393 ) ) ;
#23845 = CARTESIAN_POINT ( 'NONE',  ( -16.17583575424048092, -10.27959207348368587, 52.02966884056656482 ) ) ;
#23846 = CYLINDRICAL_SURFACE ( 'NONE', #26667, 0.1499999999999963862 ) ;
#23847 = EDGE_LOOP ( 'NONE', ( #8531, #36471, #38259, #10702 ) ) ;
#23848 = CARTESIAN_POINT ( 'NONE',  ( -23.66043351732632871, -18.11420823279021519, 59.14811234476497503 ) ) ;
#23849 = CARTESIAN_POINT ( 'NONE',  ( -15.18822458420557453, -21.91583580787659713, 68.76867073792189444 ) ) ;
#23850 = CARTESIAN_POINT ( 'NONE',  ( -17.42409385541299471, -14.80920654474434883, 62.02966884056656482 ) ) ;
#23851 = CARTESIAN_POINT ( 'NONE',  ( -15.43182990062313742, -8.046249867383863830, 74.36513541778452918 ) ) ;
#23852 = B_SPLINE_CURVE_WITH_KNOTS ( 'NONE', 1,
 ( #41463, #30887 ),
 .UNSPECIFIED., .F., .F.,
 ( 2, 2 ),
 ( 0.000000000000000000, 1.000000000000000000 ),
 .UNSPECIFIED. ) ;
#23853 = ORIENTED_EDGE ( 'NONE', *, *, #19836, .F. ) ;
#23854 = EDGE_CURVE ( 'NONE', #25935, #16796, #23999, .T. ) ;
#23855 = CARTESIAN_POINT ( 'NONE',  ( -10.64264583514116147, -11.72452599650507565, 74.66566005422028240 ) ) ;
#23856 =( BOUNDED_SURFACE ( )  B_SPLINE_SURFACE ( 3, 1, ( 
 ( #4488, #19026 ),
 ( #26911, #38204 ),
 ( #4742, #7966 ),
 ( #45149, #37473 ),
 ( #3765, #802 ),
 ( #18777, #15067 ),
 ( #4019, #11392 ) ),
 .UNSPECIFIED., .T., .F., .F. ) 
 B_SPLINE_SURFACE_WITH_KNOTS ( ( 4, 3, 4 ),
 ( 2, 2 ),
 ( 0.000000000000000000, 0.5000000000000000000, 1.000000000000000000 ),
 ( 0.000000000000000000, 1.000000000000000000 ),
 .UNSPECIFIED. ) 
 GEOMETRIC_REPRESENTATION_ITEM ( )  RATIONAL_B_SPLINE_SURFACE ( (
 ( 1.000000000000000000, 1.000000000000000000),
 ( 0.3333333333333335369, 0.3333333333333330373),
 ( 0.3333333333333335369, 0.3333333333333330373),
 ( 1.000000000000000000, 1.000000000000000000),
 ( 0.3333333333333333703, 0.3333333333333333703),
 ( 0.3333333333333333703, 0.3333333333333333703),
 ( 1.000000000000000000, 1.000000000000000000) ) ) 
 REPRESENTATION_ITEM ( '' )  SURFACE ( )  );
#23857 = CARTESIAN_POINT ( 'NONE',  ( -24.74075724160099554, -16.21284971877490122, 62.77824058731629009 ) ) ;
#23858 = VERTEX_POINT ( 'NONE', #2073 ) ;
#23859 = ORIENTED_EDGE ( 'NONE', *, *, #47997, .T. ) ;
#23860 = CARTESIAN_POINT ( 'NONE',  ( -20.60942684424193416, -21.09890871138989965, 58.65947248567252359 ) ) ;
#23861 = CARTESIAN_POINT ( 'NONE',  ( -13.07007069224803786, -8.763865476245500830, 64.16592477169881192 ) ) ;
#23862 = CARTESIAN_POINT ( 'NONE',  ( -10.42619869066336591, -14.62054329830827193, 71.61166091316889037 ) ) ;
#23863 = CARTESIAN_POINT ( 'NONE',  ( -21.62409385650551741, -6.426201560718812544, 50.50509628382439331 ) ) ;
#23864 = LINE ( 'NONE', #5144, #38497 ) ;
#23865 = DIRECTION ( 'NONE',  ( 0.9577883914167855117, 0.2682351919075576796, 0.1033986416233888400 ) ) ;
#23866 = CARTESIAN_POINT ( 'NONE',  ( -18.63708974648904615, -7.458494484969275362, 74.01877187527500723 ) ) ;
#23867 = CARTESIAN_POINT ( 'NONE',  ( -23.70580769785572883, -18.01777564070315663, 59.30378467840713341 ) ) ;
#23868 = ORIENTED_EDGE ( 'NONE', *, *, #19788, .F. ) ;
#23869 = VERTEX_POINT ( 'NONE', #9955 ) ;
#23870 = EDGE_CURVE ( 'NONE', #18335, #24420, #24256, .T. ) ;
#23871 = DIRECTION ( 'NONE',  ( -3.071710424422018668E-17, 6.404604876783312462E-16, 1.000000000000000000 ) ) ;
#23872 = DIRECTION ( 'NONE',  ( 0.000000000000000000, 0.000000000000000000, 1.000000000000000000 ) ) ;
#23873 = EDGE_CURVE ( 'NONE', #2100, #5464, #43700, .T. ) ;
#23874 = DIRECTION ( 'NONE',  ( -0.8447509909909771686, 0.5351595679979589404, 0.000000000000000000 ) ) ;
#23875 = CARTESIAN_POINT ( 'NONE',  ( -24.55229515441413923, -12.64323416470515582, 69.87268757599312607 ) ) ;
#23876 = EDGE_CURVE ( 'NONE', #33222, #32753, #13689, .T. ) ;
#23877 = LINE ( 'NONE', #15726, #45720 ) ;
#23878 = VERTEX_POINT ( 'NONE', #39263 ) ;
#23879 = CARTESIAN_POINT ( 'NONE',  ( -14.99986034619465158, -21.37608775269596961, 61.65102924131838336 ) ) ;
#23880 = CARTESIAN_POINT ( 'NONE',  ( -24.46812100523181499, -14.51191712007779522, 66.19764790277996269 ) ) ;
#23881 = DIRECTION ( 'NONE',  ( 1.000000000000000000, -4.164305804376849172E-17, 1.614929280266638808E-16 ) ) ;
#23882 = CARTESIAN_POINT ( 'NONE',  ( -24.46506355971582991, -17.24406257311080992, 72.99840714145864240 ) ) ;
#23883 = EDGE_CURVE ( 'NONE', #16869, #38050, #4537, .T. ) ;
#23884 = VERTEX_POINT ( 'NONE', #27932 ) ;
#23885 = ADVANCED_FACE ( 'NONE', ( #6012 ), #9484, .T. ) ;
#23886 = CARTESIAN_POINT ( 'NONE',  ( -20.78451513435706133, -21.00713107796517320, 62.12943504870421663 ) ) ;
#23887 = DIRECTION ( 'NONE',  ( -1.000000000000000000, -1.669677910507523057E-21, -6.493791346278465266E-22 ) ) ;
#23888 = EDGE_CURVE ( 'NONE', #10981, #38205, #17788, .T. ) ;
#23889 = ADVANCED_FACE ( 'NONE', ( #31876 ), #43209, .T. ) ;
#23890 = ORIENTED_EDGE ( 'NONE', *, *, #25774, .F. ) ;
#23891 = CARTESIAN_POINT ( 'NONE',  ( -12.88852986233651876, -20.14113829381898668, 71.82156135014017195 ) ) ;
#23892 = CARTESIAN_POINT ( 'NONE',  ( -22.09360120700997854, -20.02631313764212706, 65.81494753366123973 ) ) ;
#23893 = ORIENTED_EDGE ( 'NONE', *, *, #41325, .T. ) ;
#23894 = CARTESIAN_POINT ( 'NONE',  ( -21.89826263122328953, -8.852228171720549099, 66.84645388252840803 ) ) ;
#23895 = ORIENTED_EDGE ( 'NONE', *, *, #36502, .F. ) ;
#23896 = CARTESIAN_POINT ( 'NONE',  ( -17.09909385759799250, -8.105421454601382081, 49.25000573077640098 ) ) ;
#23897 = CARTESIAN_POINT ( 'NONE',  ( -21.67609690912980014, -8.690862426448951794, 73.78784151156415305 ) ) ;
#23898 = ORIENTED_EDGE ( 'NONE', *, *, #32523, .F. ) ;
#23899 = CARTESIAN_POINT ( 'NONE',  ( -17.42409385541300182, -14.80920654474440745, 53.27966884056655061 ) ) ;
#23900 = CARTESIAN_POINT ( 'NONE',  ( -10.27345454978659944, -12.71824136398891980, 64.45331520391344782 ) ) ;
#23901 = VECTOR ( 'NONE', #757, 1000.000000000000000 ) ;
#23902 = CARTESIAN_POINT ( 'NONE',  ( -15.69284385650551350, -7.406986770994972602, 48.81910596585309747 ) ) ;
#23903 = ORIENTED_EDGE ( 'NONE', *, *, #45645, .T. ) ;
#23904 = CARTESIAN_POINT ( 'NONE',  ( -38.65852941833841783, -25.10920654474410441, 76.99999999999998579 ) ) ;
#23905 = CARTESIAN_POINT ( 'NONE',  ( -19.17247957453286844, -7.567181637230756763, 63.61584517348745038 ) ) ;
#23906 = LINE ( 'NONE', #24142, #25835 ) ;
#23907 = VERTEX_POINT ( 'NONE', #47626 ) ;
#23908 = CARTESIAN_POINT ( 'NONE',  ( -17.42409385541299471, -14.80920654474435594, 52.02966884056656482 ) ) ;
#23909 = CARTESIAN_POINT ( 'NONE',  ( -23.83833616213321704, -17.61232902345998141, 62.77360984984811410 ) ) ;
#23910 = CARTESIAN_POINT ( 'NONE',  ( -15.38034385541287463, -9.360768649639723549, 51.01397948905911761 ) ) ;
#23911 = CARTESIAN_POINT ( 'NONE',  ( -12.91576191806997365, -9.388722997169709927, 71.13453240065665284 ) ) ;
#23912 = CARTESIAN_POINT ( 'NONE',  ( -19.23866403772855449, -21.62168293227472660, 58.67507384656568092 ) ) ;
#23913 = EDGE_CURVE ( 'NONE', #10765, #5443, #133, .T. ) ;
#23914 = EDGE_LOOP ( 'NONE', ( #2731, #9510 ) ) ;
#23915 = ORIENTED_EDGE ( 'NONE', *, *, #25222, .F. ) ;
#23916 = CARTESIAN_POINT ( 'NONE',  ( -23.75972628784533569, -10.79550978475970346, 53.49999999999994316 ) ) ;
#23917 = CARTESIAN_POINT ( 'NONE',  ( -15.09857480863590062, -8.145354156905789011, 60.46428990550709415 ) ) ;
#23918 = ORIENTED_EDGE ( 'NONE', *, *, #28547, .T. ) ;
#23919 = CARTESIAN_POINT ( 'NONE',  ( -24.49635653881819408, -12.46679777644911447, 73.35730153580948354 ) ) ;
#23920 = DIRECTION ( 'NONE',  ( 0.000000000000000000, 0.000000000000000000, -1.000000000000000000 ) ) ;
#23921 = CARTESIAN_POINT ( 'NONE',  ( -21.99284385759798965, -8.630756214087126565, 51.74842643355248129 ) ) ;
#23922 = CARTESIAN_POINT ( 'NONE',  ( -12.60227155074094441, -19.95281705956671559, 68.35129494334645983 ) ) ;
#23923 = CARTESIAN_POINT ( 'NONE',  ( -11.23768813171194836, -11.42793793434924154, 64.44322231037519089 ) ) ;
#23924 = ORIENTED_EDGE ( 'NONE', *, *, #22928, .F. ) ;
#23925 = EDGE_CURVE ( 'NONE', #25179, #9970, #13612, .T. ) ;
#23926 = CARTESIAN_POINT ( 'NONE',  ( -22.52619951119469022, -19.67884242972143483, 69.05929390617204433 ) ) ;
#23927 = CARTESIAN_POINT ( 'NONE',  ( -20.73702204056089826, -8.642680056431577995, 59.84125279967195610 ) ) ;
#23928 = CARTESIAN_POINT ( 'NONE',  ( -12.32158608955787393, -9.943909642237139579, 60.57390139315987909 ) ) ;
#23929 = CARTESIAN_POINT ( 'NONE',  ( -24.72409385541305582, -14.80920654474423159, 69.97058823529410176 ) ) ;
#23930 = CARTESIAN_POINT ( 'NONE',  ( -12.96596342764269316, -9.347744029417796696, 71.14925352873375175 ) ) ;
#23931 = VERTEX_POINT ( 'NONE', #47144 ) ;
#23932 = ORIENTED_EDGE ( 'NONE', *, *, #4313, .F. ) ;
#23933 = VECTOR ( 'NONE', #28206, 1000.000000000000000 ) ;
#23934 = ORIENTED_EDGE ( 'NONE', *, *, #44575, .T. ) ;
#23935 = CARTESIAN_POINT ( 'NONE',  ( -23.04402284766838349, -19.06632961612601918, 59.16938527523783620 ) ) ;
#23936 = AXIS2_PLACEMENT_3D ( 'NONE', #9907, #42913, #20745 ) ;
#23937 = CARTESIAN_POINT ( 'NONE',  ( -24.09502166851904903, -12.68799014041620055, 69.78745416573572413 ) ) ;
#23938 = EDGE_LOOP ( 'NONE', ( #43529, #39876, #19417, #44369, #46971 ) ) ;
#23939 = B_SPLINE_CURVE_WITH_KNOTS ( 'NONE', 1,
 ( #9432, #9678 ),
 .UNSPECIFIED., .F., .F.,
 ( 2, 2 ),
 ( 0.000000000000000000, 1.000000000000000000 ),
 .UNSPECIFIED. ) ;
#23940 = ADVANCED_FACE ( 'NONE', ( #6261 ), #29148, .T. ) ;
#23941 = CARTESIAN_POINT ( 'NONE',  ( -21.89826351590202336, -8.852228842849337198, 66.84645279485334868 ) ) ;
#23942 = FACE_OUTER_BOUND ( 'NONE', #13771, .T. ) ;
#23943 = EDGE_CURVE ( 'NONE', #8183, #37009, #25219, .T. ) ;
#23944 = EDGE_CURVE ( 'NONE', #10723, #31686, #25456, .T. ) ;
#23945 = ORIENTED_EDGE ( 'NONE', *, *, #22863, .F. ) ;
#23946 = CARTESIAN_POINT ( 'NONE',  ( -20.95083147400204382, -8.246703318114343872, 60.01938016961330646 ) ) ;
#23947 = CARTESIAN_POINT ( 'NONE',  ( -19.23951954158338751, -22.03540154427634334, 58.71162761787055473 ) ) ;
#23948 = ORIENTED_EDGE ( 'NONE', *, *, #31774, .T. ) ;
#23949 = CARTESIAN_POINT ( 'NONE',  ( -11.37640603946425522, -11.28103799867411894, 64.25955191458184856 ) ) ;
#23950 = LINE ( 'NONE', #8694, #44798 ) ;
#23951 = ORIENTED_EDGE ( 'NONE', *, *, #7749, .F. ) ;
#23952 = EDGE_CURVE ( 'NONE', #15615, #4181, #28728, .T. ) ;
#23953 = CARTESIAN_POINT ( 'NONE',  ( -22.79734292848665689, -10.24514101169484448, 66.84182257473258915 ) ) ;
#23954 = DIRECTION ( 'NONE',  ( 3.071710424422018668E-17, -6.404604876783312462E-16, -1.000000000000000000 ) ) ;
#23955 = CARTESIAN_POINT ( 'NONE',  ( -19.45676940763031837, -21.56358822076535375, 58.73327141882466407 ) ) ;
#23956 = ORIENTED_EDGE ( 'NONE', *, *, #6598, .F. ) ;
#23957 = CARTESIAN_POINT ( 'NONE',  ( -46.92409385541305511, -15.81020654474410847, 61.49999999999999289 ) ) ;
#23958 = DIRECTION ( 'NONE',  ( -0.000000000000000000, -1.000000000000000000, -0.000000000000000000 ) ) ;
#23959 = CARTESIAN_POINT ( 'NONE',  ( -17.87433636498385781, -21.79471166626661827, 58.59656648677060531 ) ) ;
#23960 = LINE ( 'NONE', #45396, #47854 ) ;
#23961 = CARTESIAN_POINT ( 'NONE',  ( -24.32752865423570654, -15.96790753223159598, 66.36324927017490438 ) ) ;
#23962 = CARTESIAN_POINT ( 'NONE',  ( -50.42609385541305755, -14.80920654474410902, 57.89999999999999147 ) ) ;
#23963 = ORIENTED_EDGE ( 'NONE', *, *, #23162, .F. ) ;
#23964 = CARTESIAN_POINT ( 'NONE',  ( -20.92409385541305511, -10.60920654474410618, 80.49999999999998579 ) ) ;
#23965 = CARTESIAN_POINT ( 'NONE',  ( -10.98557813051190202, -17.68114236276378293, 71.56718193507127523 ) ) ;
#23966 = CARTESIAN_POINT ( 'NONE',  ( -24.86610167639389246, -14.46236660854407674, 66.29797298380238146 ) ) ;
#23967 = AXIS2_PLACEMENT_3D ( 'NONE', #39043, #31421, #46454 ) ;
#23968 = CARTESIAN_POINT ( 'NONE',  ( -14.19679379891342741, -21.02091897117797004, 71.99895702512269224 ) ) ;
#23969 = CARTESIAN_POINT ( 'NONE',  ( -16.50534385650551883, -8.801233750844183135, 48.81488406609782515 ) ) ;
#23970 = EDGE_CURVE ( 'NONE', #22263, #9283, #13857, .T. ) ;
#23971 = AXIS2_PLACEMENT_3D ( 'NONE', #3176, #24867, #18182 ) ;
#23972 = ORIENTED_EDGE ( 'NONE', *, *, #4051, .T. ) ;
#23973 = DIRECTION ( 'NONE',  ( -5.731567514496413899E-31, -1.020425574103664789E-16, -1.000000000000000000 ) ) ;
#23974 = CARTESIAN_POINT ( 'NONE',  ( -19.17247849636888901, -7.567181371456696226, 63.61584626116109575 ) ) ;
#23975 = VERTEX_POINT ( 'NONE', #22488 ) ;
#23976 = CARTESIAN_POINT ( 'NONE',  ( -24.45714095472541771, -14.31630891555219165, 69.66747352629326429 ) ) ;
#23977 = LINE ( 'NONE', #37318, #29812 ) ;
#23978 = CARTESIAN_POINT ( 'NONE',  ( -11.25989503537269698, -11.38792718504117829, 64.29882039368452240 ) ) ;
#23979 = CARTESIAN_POINT ( 'NONE',  ( -22.94192455449829993, -9.803488759991966006, 70.05532601532212311 ) ) ;
#23980 = CARTESIAN_POINT ( 'NONE',  ( -12.67665486305926237, -12.56770637434968485, 49.52966884056655772 ) ) ;
#23981 =( BOUNDED_SURFACE ( )  B_SPLINE_SURFACE ( 3, 1, ( 
 ( #13230, #16455 ),
 ( #31487, #12775 ),
 ( #34930, #9093 ),
 ( #39360, #27789 ),
 ( #35169, #28282 ),
 ( #42334, #24602 ),
 ( #15965, #16202 ) ),
 .UNSPECIFIED., .T., .F., .F. ) 
 B_SPLINE_SURFACE_WITH_KNOTS ( ( 4, 3, 4 ),
 ( 2, 2 ),
 ( 0.000000000000000000, 0.5000000000000000000, 1.000000000000000000 ),
 ( 0.000000000000000000, 1.000000000000000000 ),
 .UNSPECIFIED. ) 
 GEOMETRIC_REPRESENTATION_ITEM ( )  RATIONAL_B_SPLINE_SURFACE ( (
 ( 1.000000000000000000, 1.000000000000000000),
 ( 0.3333333333333335369, 0.3333333333333330373),
 ( 0.3333333333333335369, 0.3333333333333330373),
 ( 1.000000000000000000, 1.000000000000000000),
 ( 0.3333333333333333703, 0.3333333333333333703),
 ( 0.3333333333333333703, 0.3333333333333333703),
 ( 1.000000000000000000, 1.000000000000000000) ) ) 
 REPRESENTATION_ITEM ( '' )  SURFACE ( )  );
#23982 = ORIENTED_EDGE ( 'NONE', *, *, #37134, .T. ) ;
#23983 = CARTESIAN_POINT ( 'NONE',  ( -24.79781836340079337, -15.87314503134675014, 69.64812095075065201 ) ) ;
#23984 = DIRECTION ( 'NONE',  ( 1.000000000000000000, -6.517531090241554163E-16, 3.534154189880001717E-15 ) ) ;
#23985 = CARTESIAN_POINT ( 'NONE',  ( -12.50648677543191134, -9.746390325112967545, 60.70350793514798937 ) ) ;
#23986 = EDGE_CURVE ( 'NONE', #48343, #1260, #32549, .T. ) ;
#23987 = ORIENTED_EDGE ( 'NONE', *, *, #44706, .T. ) ;
#23988 = DIRECTION ( 'NONE',  ( 2.723496474639940985E-06, 1.584719855340916648E-07, 0.9999999999962787545 ) ) ;
#23989 = CARTESIAN_POINT ( 'NONE',  ( -24.20884313412962285, -11.73171478914054155, 59.59740407230526671 ) ) ;
#23990 = LINE ( 'NONE', #46641, #15064 ) ;
#23991 = CARTESIAN_POINT ( 'NONE',  ( -21.78913961794832588, -8.771810275399618106, 70.24637145832762997 ) ) ;
#23992 = CARTESIAN_POINT ( 'NONE',  ( -10.71495605983455590, -12.81234157828920850, 64.26836111193937029 ) ) ;
#23993 =( BOUNDED_SURFACE ( )  B_SPLINE_SURFACE ( 3, 1, ( 
 ( #23600, #34409 ),
 ( #30266, #33936 ),
 ( #45286, #22620 ),
 ( #3917, #19166 ),
 ( #38109, #464 ),
 ( #8577, #37874 ),
 ( #11535, #7616 ) ),
 .UNSPECIFIED., .T., .F., .F. ) 
 B_SPLINE_SURFACE_WITH_KNOTS ( ( 4, 3, 4 ),
 ( 2, 2 ),
 ( 0.000000000000000000, 0.5000000000000000000, 1.000000000000000000 ),
 ( 0.000000000000000000, 1.000000000000000000 ),
 .UNSPECIFIED. ) 
 GEOMETRIC_REPRESENTATION_ITEM ( )  RATIONAL_B_SPLINE_SURFACE ( (
 ( 1.000000000000000000, 1.000000000000000000),
 ( 0.3333333333333335369, 0.3333333333333330373),
 ( 0.3333333333333335369, 0.3333333333333330373),
 ( 1.000000000000000000, 1.000000000000000000),
 ( 0.3333333333333333703, 0.3333333333333333703),
 ( 0.3333333333333333703, 0.3333333333333333703),
 ( 1.000000000000000000, 1.000000000000000000) ) ) 
 REPRESENTATION_ITEM ( '' )  SURFACE ( )  );
#23994 = ORIENTED_EDGE ( 'NONE', *, *, #17378, .F. ) ;
#23995 = ORIENTED_EDGE ( 'NONE', *, *, #12269, .T. ) ;
#23996 = CARTESIAN_POINT ( 'NONE',  ( -20.04909385541304445, -8.112991634885936776, 51.74999426922421719 ) ) ;
#23997 = CARTESIAN_POINT ( 'NONE',  ( -24.87123160714014958, -14.59964084223042491, 62.89791924484052998 ) ) ;
#23998 = CARTESIAN_POINT ( 'NONE',  ( -20.02766308627097303, -8.311286154507662616, 73.72096589762166730 ) ) ;
#23999 =( BOUNDED_CURVE ( )  B_SPLINE_CURVE ( 3, ( #13626, #35797, #1592, #28185 ),
 .UNSPECIFIED., .F., .F. ) 
 B_SPLINE_CURVE_WITH_KNOTS ( ( 4, 4 ),
 ( 0.5000000000000000000, 0.9074455897393656212 ),
 .UNSPECIFIED. ) 
 CURVE ( )  GEOMETRIC_REPRESENTATION_ITEM ( )  RATIONAL_B_SPLINE_CURVE ( ( 1.000000000000009992, 0.4567392136813407388, 0.3561768502900264366, 0.6983129098260781875 ) ) 
 REPRESENTATION_ITEM ( '' )  );
#24000 = CIRCLE ( 'NONE', #12967, 7.500000000000002665 ) ;
#24001 = LINE ( 'NONE', #43445, #3281 ) ;
#24002 = EDGE_CURVE ( 'NONE', #35502, #21615, #32826, .T. ) ;
#24003 = DIRECTION ( 'NONE',  ( 1.000000000000000000, 2.866981220435666553E-17, 0.000000000000000000 ) ) ;
#24004 = AXIS2_PLACEMENT_3D ( 'NONE', #19477, #4714, #4461 ) ;
#24005 = ORIENTED_EDGE ( 'NONE', *, *, #24132, .T. ) ;
#24006 = CARTESIAN_POINT ( 'NONE',  ( -12.40133225487197066, -17.08293507921495191, 53.69233794759168887 ) ) ;
#24007 = CARTESIAN_POINT ( 'NONE',  ( -18.05316936118225968, -22.23335149483498085, 65.53187476518867527 ) ) ;
#24008 = VERTEX_POINT ( 'NONE', #28903 ) ;
#24009 = CARTESIAN_POINT ( 'NONE',  ( -21.84891708756835982, -9.316868653145983004, 67.07638807817237137 ) ) ;
#24010 = PLANE ( 'NONE',  #9438 ) ;
#24011 = VERTEX_POINT ( 'NONE', #44918 ) ;
#24012 = ADVANCED_FACE ( 'NONE', ( #10205 ), #29631, .T. ) ;
#24013 = B_SPLINE_CURVE_WITH_KNOTS ( 'NONE', 3,
 ( #40437, #13353, #2537, #10171, #36712, #31848, #13110, #32091, #5981, #24714 ),
 .UNSPECIFIED., .F., .F.,
 ( 4, 2, 2, 2, 4 ),
 ( 0.000000000000000000, 0.2500000000000000000, 0.5000000000000000000, 0.7500000000000000000, 1.000000000000000000 ),
 .UNSPECIFIED. ) ;
#24014 = ADVANCED_FACE ( 'NONE', ( #22247 ), #6984, .T. ) ;
#24015 = PLANE ( 'NONE',  #18989 ) ;
#24016 = CARTESIAN_POINT ( 'NONE',  ( -14.78766009005058635, -21.34800739930362568, 58.45145834864037937 ) ) ;
#24017 = ORIENTED_EDGE ( 'NONE', *, *, #28188, .T. ) ;
#24018 = CARTESIAN_POINT ( 'NONE',  ( -17.77920954038207668, -22.25082405446125122, 58.59048702730397196 ) ) ;
#24019 = ADVANCED_FACE ( 'NONE', ( #33294 ), #34039, .T. ) ;
#24020 = CARTESIAN_POINT ( 'NONE',  ( -11.86838291625971742, -9.845553222893467904, 64.14418898700822069 ) ) ;
#24021 = EDGE_CURVE ( 'NONE', #35561, #11000, #35619, .T. ) ;
#24022 = CARTESIAN_POINT ( 'NONE',  ( -10.34976723757024253, -12.47327135604617787, 60.89879317984863860 ) ) ;
#24023 = CARTESIAN_POINT ( 'NONE',  ( -24.30537518760159088, -16.09989623713234863, 66.29154897911506339 ) ) ;
#24024 = EDGE_LOOP ( 'NONE', ( #4193, #26351, #34762, #9541, #20220 ) ) ;
#24025 = CARTESIAN_POINT ( 'NONE',  ( -10.31364510401727053, -17.03300888149450998, 57.80265138661536639 ) ) ;
#24026 = CARTESIAN_POINT ( 'NONE',  ( -24.83515304063678286, -14.04764234229505959, 73.23776096988058271 ) ) ;
#24027 = FACE_OUTER_BOUND ( 'NONE', #2709, .T. ) ;
#24028 = CARTESIAN_POINT ( 'NONE',  ( -13.95487512861695834, -17.97781459419518058, 52.02966884056656482 ) ) ;
#24029 = FACE_OUTER_BOUND ( 'NONE', #41364, .T. ) ;
#24030 = CARTESIAN_POINT ( 'NONE',  ( -11.42128300986745515, -11.20812281556079171, 60.67885827005227384 ) ) ;
#24031 = EDGE_CURVE ( 'NONE', #6094, #20234, #1983, .T. ) ;
#24032 = CARTESIAN_POINT ( 'NONE',  ( -24.37499929849812119, -16.00910627056057223, 69.83307750944575787 ) ) ;
#24033 = ORIENTED_EDGE ( 'NONE', *, *, #24228, .F. ) ;
#24034 = CARTESIAN_POINT ( 'NONE',  ( -12.10507042601503080, -10.25792974195034901, 67.51513498652721523 ) ) ;
#24035 = EDGE_LOOP ( 'NONE', ( #2885, #19999 ) ) ;
#24036 = CARTESIAN_POINT ( 'NONE',  ( -11.79630000206883977, -19.05592701419838519, 71.97213747039440079 ) ) ;
#24037 = CARTESIAN_POINT ( 'NONE',  ( -20.64108208740726624, -21.08661300460041232, 62.41471558431330635 ) ) ;
#24038 = VERTEX_POINT ( 'NONE', #41692 ) ;
#24039 = CARTESIAN_POINT ( 'NONE',  ( -23.52949419687348964, -11.28347464189849525, 70.17738639980606763 ) ) ;
#24040 = AXIS2_PLACEMENT_3D ( 'NONE', #41176, #40679, #3748 ) ;
#24041 = FACE_BOUND ( 'NONE', #16492, .T. ) ;
#24042 = VERTEX_POINT ( 'NONE', #42179 ) ;
#24043 = ORIENTED_EDGE ( 'NONE', *, *, #42286, .T. ) ;
#24044 = ORIENTED_EDGE ( 'NONE', *, *, #47941, .T. ) ;
#24045 = CARTESIAN_POINT ( 'NONE',  ( -10.01366804335076210, -15.58332129913256381, 61.22444385224647334 ) ) ;
#24046 = CARTESIAN_POINT ( 'NONE',  ( -16.03034385759799463, -6.857644439848019857, 49.98602051094139398 ) ) ;
#24047 = CARTESIAN_POINT ( 'NONE',  ( -21.21196263389317949, -8.922607336573463499, 73.71014652413226997 ) ) ;
#24048 = CARTESIAN_POINT ( 'NONE',  ( -12.62620118243013856, -19.90688802239219868, 68.35274030346421625 ) ) ;
#24049 = DIRECTION ( 'NONE',  ( 0.4415479322351505975, 0.8912598635915908174, 0.1033986416233889788 ) ) ;
#24050 = ORIENTED_EDGE ( 'NONE', *, *, #4779, .F. ) ;
#24051 = ORIENTED_EDGE ( 'NONE', *, *, #29389, .T. ) ;
#24052 = CARTESIAN_POINT ( 'NONE',  ( -21.76784385650551101, -6.428312510596451368, 51.20221977374900035 ) ) ;
#24053 = CARTESIAN_POINT ( 'NONE',  ( -21.39967327233876659, -20.63170314183283693, 72.80974286114339122 ) ) ;
#24054 = CARTESIAN_POINT ( 'NONE',  ( -17.63665770386090514, -10.11555421891855922, 52.02966884056656482 ) ) ;
#24055 = CARTESIAN_POINT ( 'NONE',  ( -24.07511766164941491, -16.99203022981017952, 72.89838494284886394 ) ) ;
#24056 = EDGE_CURVE ( 'NONE', #18974, #1509, #12371, .T. ) ;
#24057 = CARTESIAN_POINT ( 'NONE',  ( -13.91784385650551670, -9.790100578890868377, 49.79778022625163203 ) ) ;
#24058 = ORIENTED_EDGE ( 'NONE', *, *, #41790, .T. ) ;
#24059 = CARTESIAN_POINT ( 'NONE',  ( -29.92409385541305156, -6.859206544744110623, 47.99999999999997868 ) ) ;
#24060 = EDGE_CURVE ( 'NONE', #35848, #18422, #33743, .T. ) ;
#24061 = LINE ( 'NONE', #43003, #10373 ) ;
#24062 = CARTESIAN_POINT ( 'NONE',  ( -24.47325573560893730, -17.21999967669226450, 73.08347230323211363 ) ) ;
#24063 = ORIENTED_EDGE ( 'NONE', *, *, #28982, .F. ) ;
#24064 = CARTESIAN_POINT ( 'NONE',  ( -18.44528782684011858, -21.78515541812411982, 72.29983070759432451 ) ) ;
#24065 = CARTESIAN_POINT ( 'NONE',  ( -22.30326020397728115, -9.709333660337318150, 73.63728338005337548 ) ) ;
#24066 = CARTESIAN_POINT ( 'NONE',  ( -24.16575376147898169, -12.74704232990201724, 69.77243002240838621 ) ) ;
#24067 = CARTESIAN_POINT ( 'NONE',  ( -22.18998830427771196, -20.00468049915955859, 65.71893796558269685 ) ) ;
#24068 = EDGE_CURVE ( 'NONE', #23164, #27130, #38801, .T. ) ;
#24069 = ORIENTED_EDGE ( 'NONE', *, *, #38450, .F. ) ;
#24070 = CARTESIAN_POINT ( 'NONE',  ( -19.89283007060495123, -10.81159512726059191, 49.52966884056655772 ) ) ;
#24071 = EDGE_CURVE ( 'NONE', #33156, #41728, #7281, .T. ) ;
#24072 = CARTESIAN_POINT ( 'NONE',  ( -22.87317432090156899, -19.20579874941482856, 59.07337760154523920 ) ) ;
#24073 = CARTESIAN_POINT ( 'NONE',  ( 6.575906144586949331, -6.109215713985405749, 50.50605614422795497 ) ) ;
#24074 = ORIENTED_EDGE ( 'NONE', *, *, #22499, .F. ) ;
#24075 = DIRECTION ( 'NONE',  ( -0.2664710960620865765, 0.9638429098994649724, -4.833213314675864069E-08 ) ) ;
#24076 = ORIENTED_EDGE ( 'NONE', *, *, #11581, .T. ) ;
#24077 = CARTESIAN_POINT ( 'NONE',  ( -16.36003703953564070, -21.72797270546592330, 62.05568179787937311 ) ) ;
#24078 = EDGE_CURVE ( 'NONE', #34107, #2258, #21401, .T. ) ;
#24079 = ORIENTED_EDGE ( 'NONE', *, *, #41861, .T. ) ;
#24080 = CARTESIAN_POINT ( 'NONE',  ( -16.36834346081282732, -22.18410778960565466, 61.94063409281806543 ) ) ;
#24081 = CARTESIAN_POINT ( 'NONE',  ( -12.18719842096713357, -10.08886484896570934, 64.04386393395434141 ) ) ;
#24082 = CARTESIAN_POINT ( 'NONE',  ( -10.80773916950031399, -18.37978238154741462, 54.02312124697530749 ) ) ;
#24083 = ORIENTED_EDGE ( 'NONE', *, *, #39163, .F. ) ;
#24084 = CARTESIAN_POINT ( 'NONE',  ( -10.63418523514201652, -17.87528017975677130, 71.61072290056861789 ) ) ;
#24085 = EDGE_CURVE ( 'NONE', #9159, #4206, #45390, .T. ) ;
#24086 = CARTESIAN_POINT ( 'NONE',  ( -20.72450927900464634, -21.03929139025763106, 58.93003081252663833 ) ) ;
#24087 = CARTESIAN_POINT ( 'NONE',  ( -22.22951888192506686, -9.116124670579511147, 59.91445369977274282 ) ) ;
#24088 = VERTEX_POINT ( 'NONE', #11902 ) ;
#24089 = B_SPLINE_CURVE_WITH_KNOTS ( 'NONE', 1,
 ( #47588, #20756 ),
 .UNSPECIFIED., .F., .F.,
 ( 2, 2 ),
 ( 0.000000000000000000, 1.000000000000000000 ),
 .UNSPECIFIED. ) ;
#24090 = CARTESIAN_POINT ( 'NONE',  ( -21.69457540385530336, -9.196023516753362159, 70.54621400560100142 ) ) ;
#24091 = ORIENTED_EDGE ( 'NONE', *, *, #19300, .F. ) ;
#24092 = ORIENTED_EDGE ( 'NONE', *, *, #10488, .F. ) ;
#24093 = DIRECTION ( 'NONE',  ( -0.9998756790481364565, -0.01576789294826319576, -3.907472230461691850E-09 ) ) ;
#24094 = CARTESIAN_POINT ( 'NONE',  ( -13.22529448846758804, -9.145569705956512863, 64.19474388871357462 ) ) ;
#24095 = CARTESIAN_POINT ( 'NONE',  ( -10.96069698787312596, -18.51437578577013809, 57.92219301334858272 ) ) ;
#24096 = CARTESIAN_POINT ( 'NONE',  ( -19.31784385650551528, -9.790100578890868377, 49.79778022625163203 ) ) ;
#24097 = CARTESIAN_POINT ( 'NONE',  ( -12.12786991918758339, -13.32596279628197600, 53.49999999999995026 ) ) ;
#24098 = DIRECTION ( 'NONE',  ( 0.1555549491741979040, 0.4192882752801622703, 0.8944271909999156334 ) ) ;
#24099 = CARTESIAN_POINT ( 'NONE',  ( -24.28579947082789303, -13.18942387424446316, 62.84736316175410309 ) ) ;
#24100 = CARTESIAN_POINT ( 'NONE',  ( -18.72680718162379065, -7.880610904852765941, 70.67068030199192208 ) ) ;
#24101 = AXIS2_PLACEMENT_3D ( 'NONE', #25044, #39327, #39569 ) ;
#24102 = VECTOR ( 'NONE', #44524, 1000.000000000000114 ) ;
#24103 = ORIENTED_EDGE ( 'NONE', *, *, #44209, .F. ) ;
#24104 = EDGE_LOOP ( 'NONE', ( #39761, #33295, #27827, #31673 ) ) ;
#24105 = CARTESIAN_POINT ( 'NONE',  ( -24.43827367352892210, -15.52193379869737200, 73.28831629023289906 ) ) ;
#24106 =( NAMED_UNIT ( * ) PLANE_ANGLE_UNIT ( ) SI_UNIT ( $, .RADIAN. ) );
#24107 = CARTESIAN_POINT ( 'NONE',  ( -22.69284385541299542, -8.630756214087158540, 51.74842643355255944 ) ) ;
#24108 = CARTESIAN_POINT ( 'NONE',  ( -14.90981281861414587, -21.39562369906352757, 61.78600440604535748 ) ) ;
#24109 = DIRECTION ( 'NONE',  ( -1.000000000000000000, 3.159776991290051445E-16, -3.534154189880001717E-15 ) ) ;
#24110 = EDGE_CURVE ( 'NONE', #33575, #17355, #5157, .T. ) ;
#24111 = VERTEX_POINT ( 'NONE', #20011 ) ;
#24112 = CARTESIAN_POINT ( 'NONE',  ( -20.16542227925740249, -21.73660035250202327, 72.44832829956453679 ) ) ;
#24113 = CARTESIAN_POINT ( 'NONE',  ( -15.19549097431359463, -21.91815212410659086, 68.76088336006283441 ) ) ;
#24114 = FACE_OUTER_BOUND ( 'NONE', #22605, .T. ) ;
#24115 = CARTESIAN_POINT ( 'NONE',  ( -13.89389072038462025, -21.36980434119256600, 72.11103101793651149 ) ) ;
#24116 =( BOUNDED_SURFACE ( )  B_SPLINE_SURFACE ( 3, 1, ( 
 ( #7807, #9433 ),
 ( #19111, #37817 ),
 ( #17025, #19347 ),
 ( #13094, #34117 ),
 ( #11725, #34354 ),
 ( #408, #42916 ),
 ( #28134, #26500 ) ),
 .UNSPECIFIED., .T., .F., .F. ) 
 B_SPLINE_SURFACE_WITH_KNOTS ( ( 4, 3, 4 ),
 ( 2, 2 ),
 ( 0.000000000000000000, 0.5000000000000000000, 1.000000000000000000 ),
 ( 0.000000000000000000, 1.000000000000000000 ),
 .UNSPECIFIED. ) 
 GEOMETRIC_REPRESENTATION_ITEM ( )  RATIONAL_B_SPLINE_SURFACE ( (
 ( 1.000000000000000000, 1.000000000000000000),
 ( 0.3333333333333335369, 0.3333333333333330373),
 ( 0.3333333333333335369, 0.3333333333333330373),
 ( 1.000000000000000000, 1.000000000000000000),
 ( 0.3333333333333333703, 0.3333333333333333703),
 ( 0.3333333333333333703, 0.3333333333333333703),
 ( 1.000000000000000000, 1.000000000000000000) ) ) 
 REPRESENTATION_ITEM ( '' )  SURFACE ( )  );
#24117 = ORIENTED_EDGE ( 'NONE', *, *, #12067, .F. ) ;
#24118 = B_SPLINE_CURVE_WITH_KNOTS ( 'NONE', 1,
 ( #25161, #40409 ),
 .UNSPECIFIED., .F., .F.,
 ( 2, 2 ),
 ( 0.000000000000000000, 1.000000000000000000 ),
 .UNSPECIFIED. ) ;
#24119 = CARTESIAN_POINT ( 'NONE',  ( -20.15023299215415875, -8.307456060669188957, 70.54540580827605822 ) ) ;
#24120 = CARTESIAN_POINT ( 'NONE',  ( -24.72409385541305582, -14.90920654474412643, 59.91176470588234793 ) ) ;
#24121 = ORIENTED_EDGE ( 'NONE', *, *, #35721, .T. ) ;
#24122 = EDGE_CURVE ( 'NONE', #21656, #11148, #44864, .T. ) ;
#24123 = CARTESIAN_POINT ( 'NONE',  ( -10.10901086070973420, -13.39385379864076242, 74.79162305847758319 ) ) ;
#24124 = CARTESIAN_POINT ( 'NONE',  ( -22.65368503412153700, -20.11523923737162178, 69.37429185709522983 ) ) ;
#24125 = CARTESIAN_POINT ( 'NONE',  ( -23.51785832295892931, -11.36449550514380036, 69.89210750611785272 ) ) ;
#24126 = VERTEX_POINT ( 'NONE', #23229 ) ;
#24127 = CARTESIAN_POINT ( 'NONE',  ( -20.32439191831477032, -7.946881181506595837, 70.35762050598125938 ) ) ;
#24128 =( BOUNDED_CURVE ( )  B_SPLINE_CURVE ( 3, ( #30960, #19625, #4605, #26528 ),
 .UNSPECIFIED., .F., .F. ) 
 B_SPLINE_CURVE_WITH_KNOTS ( ( 4, 4 ),
 ( 0.5000000000000000000, 0.9074455897393722825 ),
 .UNSPECIFIED. ) 
 CURVE ( )  GEOMETRIC_REPRESENTATION_ITEM ( )  RATIONAL_B_SPLINE_CURVE ( ( 0.9999999999999737987, 0.4567392136813237524, 0.3561768502900454769, 0.6983129098261104950 ) ) 
 REPRESENTATION_ITEM ( '' )  );
#24129 = VECTOR ( 'NONE', #7444, 1000.000000000000227 ) ;
#24130 = EDGE_LOOP ( 'NONE', ( #3116, #35315, #32809, #39744, #12400 ) ) ;
#24131 = CARTESIAN_POINT ( 'NONE',  ( -17.91451193640577344, -22.24313339626381847, 61.99040498927033127 ) ) ;
#24132 = EDGE_CURVE ( 'NONE', #26764, #7211, #19276, .T. ) ;
#24133 = CARTESIAN_POINT ( 'NONE',  ( -18.53556661698576136, -22.17591588139245573, 72.40015654177148008 ) ) ;
#24134 = VERTEX_POINT ( 'NONE', #38215 ) ;
#24135 = DIRECTION ( 'NONE',  ( -5.731567514496413899E-31, -1.020425574103664789E-16, -1.000000000000000000 ) ) ;
#24136 = LINE ( 'NONE', #9362, #14727 ) ;
#24137 = CARTESIAN_POINT ( 'NONE',  ( -17.09909385650551528, -8.114302828567740988, 52.18300498402516041 ) ) ;
#24138 = VERTEX_POINT ( 'NONE', #4501 ) ;
#24139 = CARTESIAN_POINT ( 'NONE',  ( -15.08687585379459506, -21.46369733121157708, 68.99081615631787656 ) ) ;
#24140 = EDGE_CURVE ( 'NONE', #40764, #24808, #9020, .T. ) ;
#24141 = VECTOR ( 'NONE', #39830, 1000.000000000000114 ) ;
#24142 = CARTESIAN_POINT ( 'NONE',  ( -11.35824856342118494, -11.21643317443627019, 60.97885780702566905 ) ) ;
#24143 = ORIENTED_EDGE ( 'NONE', *, *, #13800, .F. ) ;
#24144 = DIRECTION ( 'NONE',  ( 0.9687793358424821033, -0.2479245821708679909, 0.000000000000000000 ) ) ;
#24145 = CARTESIAN_POINT ( 'NONE',  ( -10.44938425464750331, -17.42781160170326871, 64.88385290183622089 ) ) ;
#24146 = CARTESIAN_POINT ( 'NONE',  ( -22.14090652532222236, -20.04928072148792495, 62.51967078134249078 ) ) ;
#24147 = PLANE ( 'NONE',  #29007 ) ;
#24148 = CARTESIAN_POINT ( 'NONE',  ( -12.20309502476489882, -20.12380431889209831, 64.98179558605960437 ) ) ;
#24149 = ORIENTED_EDGE ( 'NONE', *, *, #10356, .T. ) ;
#24150 = ORIENTED_EDGE ( 'NONE', *, *, #1970, .T. ) ;
#24151 = CARTESIAN_POINT ( 'NONE',  ( -17.42409385541299471, -14.80920654474435771, 49.52966884056655772 ) ) ;
#24152 = CARTESIAN_POINT ( 'NONE',  ( -21.90458132784462109, -18.02218142073060747, 53.69233794759168887 ) ) ;
#24153 = ORIENTED_EDGE ( 'NONE', *, *, #7401, .F. ) ;
#24154 = CARTESIAN_POINT ( 'NONE',  ( -15.89079584495563502, -7.517933547575396780, 67.32662675182959333 ) ) ;
#24155 = CARTESIAN_POINT ( 'NONE',  ( -10.67383815757964527, -12.77521617179723457, 64.26836124819834595 ) ) ;
#24156 = CARTESIAN_POINT ( 'NONE',  ( -20.53034385759798752, -6.857644439848013640, 49.98602051094139398 ) ) ;
#24157 = CARTESIAN_POINT ( 'NONE',  ( -24.38756562526642213, -15.91227465074931935, 66.34852784166324113 ) ) ;
#24158 = ADVANCED_FACE ( 'NONE', ( #47081 ), #8935, .T. ) ;
#24159 = CARTESIAN_POINT ( 'NONE',  ( -17.73224099643095286, -22.30287356026373047, 47.99999999999994316 ) ) ;
#24160 = CARTESIAN_POINT ( 'NONE',  ( -15.73541995410094785, -8.015833115459232161, 70.90989886597125746 ) ) ;
#24161 = EDGE_CURVE ( 'NONE', #20341, #21691, #44146, .T. ) ;
#24162 = VERTEX_POINT ( 'NONE', #13082 ) ;
#24163 = LINE ( 'NONE', #17235, #10792 ) ;
#24164 = ADVANCED_FACE ( 'NONE', ( #13322 ), #5485, .T. ) ;
#24165 = CARTESIAN_POINT ( 'NONE',  ( -23.75972628784533569, -10.79550978475969991, 54.27966884056655061 ) ) ;
#24166 = FACE_OUTER_BOUND ( 'NONE', #41048, .T. ) ;
#24167 = CARTESIAN_POINT ( 'NONE',  ( -22.85412030071255174, -9.708305165406962089, 73.60444179007319576 ) ) ;
#24168 = CARTESIAN_POINT ( 'NONE',  ( -12.77099661245330076, -20.03938978082239331, 72.09037095764423952 ) ) ;
#24169 = ORIENTED_EDGE ( 'NONE', *, *, #33890, .F. ) ;
#24170 = CIRCLE ( 'NONE', #46968, 1.500000000000001332 ) ;
#24171 = ORIENTED_EDGE ( 'NONE', *, *, #6809, .T. ) ;
#24172 = AXIS2_PLACEMENT_3D ( 'NONE', #20177, #35190, #27807 ) ;
#24173 = EDGE_LOOP ( 'NONE', ( #33622, #21268, #10029, #5969 ) ) ;
#24174 = CARTESIAN_POINT ( 'NONE',  ( -24.46737407909346373, -14.43901797238471474, 62.59807894131280648 ) ) ;
#24175 = DIRECTION ( 'NONE',  ( -3.071710424422018668E-17, 6.404604876783312462E-16, 1.000000000000000000 ) ) ;
#24176 = AXIS2_PLACEMENT_3D ( 'NONE', #26916, #41930, #28367 ) ;
#24177 = B_SPLINE_CURVE_WITH_KNOTS ( 'NONE', 3,
 ( #38425, #7939, #15280, #37698, #27355, #26888, #8176, #34005, #23683, #30830 ),
 .UNSPECIFIED., .F., .F.,
 ( 4, 2, 2, 2, 4 ),
 ( 0.6272669072877551377, 0.7522669073072753010, 0.8772669073267955753, 1.002266907346315739, 1.127266907365835902 ),
 .UNSPECIFIED. ) ;
#24178 = ORIENTED_EDGE ( 'NONE', *, *, #38220, .F. ) ;
#24179 = CARTESIAN_POINT ( 'NONE',  ( -21.82409385759798681, -9.359200813967568422, 50.49621490985803263 ) ) ;
#24180 = CARTESIAN_POINT ( 'NONE',  ( -36.42409385541304800, -8.109206544743658540, 50.50000000000030553 ) ) ;
#24181 = ORIENTED_EDGE ( 'NONE', *, *, #36170, .T. ) ;
#24182 = CARTESIAN_POINT ( 'NONE',  ( -11.19706266256277694, -11.50303319689152737, 67.63336710488009373 ) ) ;
#24183 = DIRECTION ( 'NONE',  ( 0.7029450532227031756, 0.7112441579020042370, -7.405715380709557223E-09 ) ) ;
#24184 = EDGE_LOOP ( 'NONE', ( #22102, #8434, #471, #8329 ) ) ;
#24185 = CARTESIAN_POINT ( 'NONE',  ( -19.99669925590731268, -21.37628624441394010, 68.81993804536961079 ) ) ;
#24186 = ORIENTED_EDGE ( 'NONE', *, *, #33187, .F. ) ;
#24187 = CARTESIAN_POINT ( 'NONE',  ( -13.47893868739161860, -21.12894084225150237, 65.09354747223889603 ) ) ;
#24188 = ORIENTED_EDGE ( 'NONE', *, *, #4183, .T. ) ;
#24189 = CARTESIAN_POINT ( 'NONE',  ( -24.47432067347917695, -14.77756146504815327, 59.52828185648635184 ) ) ;
#24190 = DIRECTION ( 'NONE',  ( -1.224646799147353207E-16, -1.000000000000000000, 1.912410701131276611E-32 ) ) ;
#24191 = EDGE_CURVE ( 'NONE', #28056, #34212, #2257, .T. ) ;
#24192 = CARTESIAN_POINT ( 'NONE',  ( -24.04523827240123879, -12.53716690146120349, 73.54225551603398969 ) ) ;
#24193 = ORIENTED_EDGE ( 'NONE', *, *, #33815, .T. ) ;
#24194 = FACE_BOUND ( 'NONE', #29268, .T. ) ;
#24195 = CARTESIAN_POINT ( 'NONE',  ( -14.67111564601650997, -7.886426081561471513, 60.43500846974642116 ) ) ;
#24196 = CARTESIAN_POINT ( 'NONE',  ( -21.78444843227217120, -20.35286453386188299, 59.17931667745679647 ) ) ;
#24197 = EDGE_CURVE ( 'NONE', #45841, #34358, #10193, .T. ) ;
#24198 = CARTESIAN_POINT ( 'NONE',  ( -24.46146587544552276, -14.38248120490118787, 66.46820668217904426 ) ) ;
#24199 = CARTESIAN_POINT ( 'NONE',  ( -19.28352822169459202, -22.07505156356299381, 54.27966884056655061 ) ) ;
#24200 = CARTESIAN_POINT ( 'NONE',  ( -10.40639875119161495, -17.31059493320988807, 61.29596613180959963 ) ) ;
#24201 = ORIENTED_EDGE ( 'NONE', *, *, #31986, .T. ) ;
#24202 = CARTESIAN_POINT ( 'NONE',  ( -17.90106345612152694, -14.65920654474411045, 48.99999999999997868 ) ) ;
#24203 = VECTOR ( 'NONE', #39441, 1000.000000000000114 ) ;
#24204 = CARTESIAN_POINT ( 'NONE',  ( -11.88446955661387783, -10.44372876568607467, 67.38408161429789800 ) ) ;
#24205 = CARTESIAN_POINT ( 'NONE',  ( -24.86282145624321771, -14.39856946235243740, 66.37566895130898104 ) ) ;
#24206 = CARTESIAN_POINT ( 'NONE',  ( -19.85909425162068942, -21.37257694502213567, 72.64634926892956912 ) ) ;
#24207 = CARTESIAN_POINT ( 'NONE',  ( -22.07864594086649390, -14.26292169798353804, 52.02966884056656482 ) ) ;
#24208 = CARTESIAN_POINT ( 'NONE',  ( -15.09909385650551705, -8.114302828567740988, 52.18300498402516041 ) ) ;
#24209 = ORIENTED_EDGE ( 'NONE', *, *, #11005, .T. ) ;
#24210 = CARTESIAN_POINT ( 'NONE',  ( -22.73240514691177339, -10.24592387063649213, 66.84182232556784697 ) ) ;
#24211 = CARTESIAN_POINT ( 'NONE',  ( -24.36317976709624489, -13.54274187105164096, 59.66268222191824577 ) ) ;
#24212 = ORIENTED_EDGE ( 'NONE', *, *, #10316, .F. ) ;
#24213 = CARTESIAN_POINT ( 'NONE',  ( -8.870383383897287644, -17.98261270965173964, 54.44843099904672812 ) ) ;
#24214 = CARTESIAN_POINT ( 'NONE',  ( -10.65090795921773292, -13.04125047316982844, 67.73832310984637672 ) ) ;
#24216 = CARTESIAN_POINT ( 'NONE',  ( -23.01445215836851688, -10.50074233538543211, 66.68615203886294296 ) ) ;
#24215 =( BOUNDED_CURVE ( )  B_SPLINE_CURVE ( 3, ( #37895, #33955, #34429, #23138 ),
 .UNSPECIFIED., .F., .F. ) 
 B_SPLINE_CURVE_WITH_KNOTS ( ( 4, 4 ),
 ( 0.000000000000000000, 0.4074455897393590154 ),
 .UNSPECIFIED. ) 
 CURVE ( )  GEOMETRIC_REPRESENTATION_ITEM ( )  RATIONAL_B_SPLINE_CURVE ( ( 1.000000000000000000, 0.4567392136813477332, 0.3561768502900360955, 0.6983129098260651979 ) ) 
 REPRESENTATION_ITEM ( '' )  );
#24217 = VECTOR ( 'NONE', #13631, 1000.000000000000000 ) ;
#24218 = CARTESIAN_POINT ( 'NONE',  ( -22.89146017634119090, -10.34570183799575105, 70.15611359559922278 ) ) ;
#24219 = CARTESIAN_POINT ( 'NONE',  ( -15.40811923343077083, -21.56513327689926030, 72.06047564147742435 ) ) ;
#24220 = ORIENTED_EDGE ( 'NONE', *, *, #8676, .T. ) ;
#24221 = AXIS2_PLACEMENT_3D ( 'NONE', #26382, #6940, #33496 ) ;
#24222 = CARTESIAN_POINT ( 'NONE',  ( -22.36119861860539970, -19.84690848826603826, 72.73580505782045691 ) ) ;
#24223 = EDGE_CURVE ( 'NONE', #38799, #8569, #17362, .T. ) ;
#24224 = DIRECTION ( 'NONE',  ( 0.9180681052388952601, -0.3964226963016427852, 0.000000000000000000 ) ) ;
#24225 = B_SPLINE_CURVE_WITH_KNOTS ( 'NONE', 3,
 ( #18452, #33460, #19198, #22658, #41124, #26845, #48496, #34205, #29804, #496 ),
 .UNSPECIFIED., .F., .F.,
 ( 4, 2, 2, 2, 4 ),
 ( 0.6272669072794416767, 0.7522669073010392893, 0.8772669073226370129, 1.002266907344234736, 1.127266907365832349 ),
 .UNSPECIFIED. ) ;
#24226 = CARTESIAN_POINT ( 'NONE',  ( -24.01466881428832423, -11.33545808864497317, 66.62225715447883090 ) ) ;
#24227 = ADVANCED_FACE ( 'NONE', ( #47332 ), #35256, .T. ) ;
#24228 = EDGE_CURVE ( 'NONE', #41313, #46985, #15193, .T. ) ;
#24229 = ADVANCED_FACE ( 'NONE', ( #38957 ), #20243, .T. ) ;
#24230 = VERTEX_POINT ( 'NONE', #16290 ) ;
#24231 = CARTESIAN_POINT ( 'NONE',  ( -17.22281099395510751, -7.361840332823870625, 70.60540513140719554 ) ) ;
#24232 = CARTESIAN_POINT ( 'NONE',  ( -13.24261801534493088, -8.643248549050911222, 60.55454889300790455 ) ) ;
#24233 = CARTESIAN_POINT ( 'NONE',  ( -24.56094871161024074, -12.67152442997557138, 69.89526119744265031 ) ) ;
#24234 = PLANE ( 'NONE',  #46457 ) ;
#24235 = CARTESIAN_POINT ( 'NONE',  ( -10.72615842429304323, -12.77470339663601884, 64.26836133915887217 ) ) ;
#24236 = ORIENTED_EDGE ( 'NONE', *, *, #16767, .F. ) ;
#24237 = VERTEX_POINT ( 'NONE', #9175 ) ;
#24238 = CARTESIAN_POINT ( 'NONE',  ( -20.16159385541304161, -7.228003583438117552, 51.38655588711986155 ) ) ;
#24239 = CARTESIAN_POINT ( 'NONE',  ( -14.94951841260375680, -8.207726002052595504, 57.14999999999999147 ) ) ;
#24240 = AXIS2_PLACEMENT_3D ( 'NONE', #46835, #24913, #31576 ) ;
#24241 = B_SPLINE_CURVE_WITH_KNOTS ( 'NONE', 1,
 ( #7684, #3729 ),
 .UNSPECIFIED., .F., .F.,
 ( 2, 2 ),
 ( 0.000000000000000000, 1.000000000000000000 ),
 .UNSPECIFIED. ) ;
#24242 = FACE_OUTER_BOUND ( 'NONE', #9978, .T. ) ;
#24243 = VECTOR ( 'NONE', #11369, 1000.000000000000114 ) ;
#24244 = CARTESIAN_POINT ( 'NONE',  ( -11.93195840498443516, -10.38844327383712773, 70.98365212470247343 ) ) ;
#24245 = VECTOR ( 'NONE', #38340, 1000.000000000000114 ) ;
#24246 = AXIS2_PLACEMENT_3D ( 'NONE', #35442, #5423, #46784 ) ;
#24247 = ADVANCED_FACE ( 'NONE', ( #2015, #32059 ), #43399, .F. ) ;
#24248 = DIRECTION ( 'NONE',  ( -0.5351595679979681552, -0.8447509909909712844, 0.000000000000000000 ) ) ;
#24249 = CARTESIAN_POINT ( 'NONE',  ( -19.69746735473979271, -8.127384799358436496, 73.87663944647505332 ) ) ;
#24250 = CARTESIAN_POINT ( 'NONE',  ( -24.46244378207920533, -14.40150055328341416, 66.47732963455544564 ) ) ;
#24251 = ORIENTED_EDGE ( 'NONE', *, *, #24780, .T. ) ;
#24252 = CARTESIAN_POINT ( 'NONE',  ( -22.37418574346156674, -19.75878307522992117, 69.47417994538778885 ) ) ;
#24253 = CARTESIAN_POINT ( 'NONE',  ( -17.00708426123225436, -7.821638799215111071, 74.26018273346642218 ) ) ;
#24254 = VERTEX_POINT ( 'NONE', #10388 ) ;
#24255 = CARTESIAN_POINT ( 'NONE',  ( -13.36999615062635627, -21.05974885748268477, 61.65499767053672997 ) ) ;
#24256 = LINE ( 'NONE', #20310, #9291 ) ;
#24257 = VERTEX_POINT ( 'NONE', #22188 ) ;
#24258 = CARTESIAN_POINT ( 'NONE',  ( -10.04821600842096174, -15.85811274820897410, 64.62276192103250594 ) ) ;
#24259 = CARTESIAN_POINT ( 'NONE',  ( -23.96075635701088657, -17.45014263229036899, 66.09357239682297802 ) ) ;
#24260 = ADVANCED_FACE ( 'NONE', ( #36935 ), #48038, .F. ) ;
#24261 =( BOUNDED_CURVE ( )  B_SPLINE_CURVE ( 3, ( #36628, #29508, #32938, #40579 ),
 .UNSPECIFIED., .F., .F. ) 
 B_SPLINE_CURVE_WITH_KNOTS ( ( 4, 4 ),
 ( 0.4074455897393696180, 0.5000000000000000000 ),
 .UNSPECIFIED. ) 
 CURVE ( )  GEOMETRIC_REPRESENTATION_ITEM ( )  RATIONAL_B_SPLINE_CURVE ( ( 0.6983129098261057210, 0.7760317562607019770, 0.8765941196519980716, 0.9999999999999885647 ) ) 
 REPRESENTATION_ITEM ( '' )  );
#24262 = CARTESIAN_POINT ( 'NONE',  ( -17.42409385541299471, -14.80920654474434883, 62.02966884056656482 ) ) ;
#24263 = LINE ( 'NONE', #35568, #6386 ) ;
#24264 = ORIENTED_EDGE ( 'NONE', *, *, #23223, .F. ) ;
#24265 = LINE ( 'NONE', #20805, #10855 ) ;
#24266 = CARTESIAN_POINT ( 'NONE',  ( -24.22593759466564123, -12.94379566627669753, 70.18731784193515466 ) ) ;
#24267 = CARTESIAN_POINT ( 'NONE',  ( 18.54465614458695200, 3.140741878271521070, 50.53406581128081143 ) ) ;
#24268 = CYLINDRICAL_SURFACE ( 'NONE', #36062, 4.686499999999997002 ) ;
#24269 = DIRECTION ( 'NONE',  ( 0.000000000000000000, 0.000000000000000000, 1.000000000000000000 ) ) ;
#24270 = AXIS2_PLACEMENT_3D ( 'NONE', #22069, #3851, #25513 ) ;
#24271 = ORIENTED_EDGE ( 'NONE', *, *, #38718, .T. ) ;
#24272 = CARTESIAN_POINT ( 'NONE',  ( -12.15107435476290476, -10.20293192550022887, 67.60969940840475090 ) ) ;
#24273 = AXIS2_PLACEMENT_3D ( 'NONE', #787, #11618, #41660 ) ;
#24274 = CARTESIAN_POINT ( 'NONE',  ( -21.34371786970645957, -8.944908702776254827, 70.33952284808852085 ) ) ;
#24275 = CARTESIAN_POINT ( 'NONE',  ( -27.42409385541305511, -27.10920654474410796, 45.99999999999998579 ) ) ;
#24276 = ORIENTED_EDGE ( 'NONE', *, *, #23462, .T. ) ;
#24277 =( BOUNDED_SURFACE ( )  B_SPLINE_SURFACE ( 3, 1, ( 
 ( #43281, #5849 ),
 ( #16428, #46496 ),
 ( #46244, #35388 ),
 ( #12501, #5125 ),
 ( #39083, #20385 ),
 ( #47210, #1664 ),
 ( #46731, #16671 ) ),
 .UNSPECIFIED., .T., .F., .F. ) 
 B_SPLINE_SURFACE_WITH_KNOTS ( ( 4, 3, 4 ),
 ( 2, 2 ),
 ( 0.000000000000000000, 0.5000000000000000000, 1.000000000000000000 ),
 ( 0.000000000000000000, 1.000000000000000000 ),
 .UNSPECIFIED. ) 
 GEOMETRIC_REPRESENTATION_ITEM ( )  RATIONAL_B_SPLINE_SURFACE ( (
 ( 1.000000000000000000, 1.000000000000000000),
 ( 0.3333333333333335369, 0.3333333333333330373),
 ( 0.3333333333333335369, 0.3333333333333330373),
 ( 1.000000000000000000, 1.000000000000000000),
 ( 0.3333333333333333703, 0.3333333333333333703),
 ( 0.3333333333333333703, 0.3333333333333333703),
 ( 1.000000000000000000, 1.000000000000000000) ) ) 
 REPRESENTATION_ITEM ( '' )  SURFACE ( )  );
#24278 = CARTESIAN_POINT ( 'NONE',  ( -19.97164249076357478, -21.81019033462135326, 69.11977790463622284 ) ) ;
#24279 = VERTEX_POINT ( 'NONE', #25875 ) ;
#24280 = EDGE_CURVE ( 'NONE', #18615, #26011, #25285, .T. ) ;
#24281 = EDGE_CURVE ( 'NONE', #19220, #43790, #27438, .T. ) ;
#24282 = ORIENTED_EDGE ( 'NONE', *, *, #46303, .T. ) ;
#24283 = ORIENTED_EDGE ( 'NONE', *, *, #7382, .F. ) ;
#24284 = CARTESIAN_POINT ( 'NONE',  ( -27.42409385541305511, -10.60920654474410618, 78.99999999999998579 ) ) ;
#24285 = VECTOR ( 'NONE', #32065, 1000.000000000000000 ) ;
#24286 = CARTESIAN_POINT ( 'NONE',  ( -23.11004506455387286, -18.89484730755139097, 65.93462627863057435 ) ) ;
#24287 = CARTESIAN_POINT ( 'NONE',  ( -17.43929471692764110, -7.359095739104631662, 67.14322671830493050 ) ) ;
#24288 = CARTESIAN_POINT ( 'NONE',  ( -22.18998830427770841, -20.00468049915955859, 65.71893796558269685 ) ) ;
#24289 = CARTESIAN_POINT ( 'NONE',  ( -13.35680526357598907, -9.112014215067329559, 60.51238218377614686 ) ) ;
#24290 =( BOUNDED_CURVE ( )  B_SPLINE_CURVE ( 3, ( #18969, #48506, #25863, #26352 ),
 .UNSPECIFIED., .F., .F. ) 
 B_SPLINE_CURVE_WITH_KNOTS ( ( 4, 4 ),
 ( 0.5000000000000000000, 0.9074455897393624015 ),
 .UNSPECIFIED. ) 
 CURVE ( )  GEOMETRIC_REPRESENTATION_ITEM ( )  RATIONAL_B_SPLINE_CURVE ( ( 0.9999999999999961142, 0.4567392136813360204, 0.3561768502900343747, 0.6983129098260869583 ) ) 
 REPRESENTATION_ITEM ( '' )  );
#24291 = EDGE_LOOP ( 'NONE', ( #28974, #4489, #17404, #3103, #46340 ) ) ;
#24292 = VERTEX_POINT ( 'NONE', #2966 ) ;
#24293 = EDGE_CURVE ( 'NONE', #19018, #16518, #40176, .T. ) ;
#24294 = ADVANCED_FACE ( 'NONE', ( #3220, #29083 ), #40406, .F. ) ;
#24295 = CARTESIAN_POINT ( 'NONE',  ( -22.21784385650551741, -9.790100578890868377, 49.79778022625163203 ) ) ;
#24296 = EDGE_CURVE ( 'NONE', #20914, #35358, #43737, .T. ) ;
#24297 = CARTESIAN_POINT ( 'NONE',  ( 18.87590614458706995, 1.876874565721113663, 52.48023137145496264 ) ) ;
#24298 = B_SPLINE_CURVE_WITH_KNOTS ( 'NONE', 1,
 ( #16308, #31350 ),
 .UNSPECIFIED., .F., .F.,
 ( 2, 2 ),
 ( 0.000000000000000000, 1.000000000000000000 ),
 .UNSPECIFIED. ) ;
#24299 = CARTESIAN_POINT ( 'NONE',  ( -21.06634951290973845, -21.30826427787840771, 62.29966696806321380 ) ) ;
#24300 = CARTESIAN_POINT ( 'NONE',  ( -11.78496890316388601, -19.04062034903473943, 71.98126064821275349 ) ) ;
#24301 = CARTESIAN_POINT ( 'NONE',  ( -13.74909385650551563, -8.104110260919579645, 48.81699501597546487 ) ) ;
#24302 = ORIENTED_EDGE ( 'NONE', *, *, #24669, .T. ) ;
#24303 = CARTESIAN_POINT ( 'NONE',  ( -14.51911023200684703, -18.48675360735852280, 49.52966884056656482 ) ) ;
#24304 = EDGE_CURVE ( 'NONE', #28056, #34569, #3870, .T. ) ;
#24305 = DIRECTION ( 'NONE',  ( -0.6323592902076722311, -0.7746752403995150749, 4.984538757074984646E-08 ) ) ;
#24306 = CIRCLE ( 'NONE', #1470, 1.249999999999999556 ) ;
#24307 = FACE_OUTER_BOUND ( 'NONE', #5598, .T. ) ;
#24308 = ORIENTED_EDGE ( 'NONE', *, *, #11323, .T. ) ;
#24309 = CARTESIAN_POINT ( 'NONE',  ( -11.74354864239398033, -18.98466756590228144, 71.68685913525695241 ) ) ;
#24310 = PLANE ( 'NONE',  #29999 ) ;
#24311 = CARTESIAN_POINT ( 'NONE',  ( -10.98696356482225944, -12.05889540143101080, 74.78513726815877760 ) ) ;
#24312 = CARTESIAN_POINT ( 'NONE',  ( -12.58019717620059197, -16.04882945559874585, 53.27966884056655061 ) ) ;
#24313 = ORIENTED_EDGE ( 'NONE', *, *, #21918, .T. ) ;
#24314 = VECTOR ( 'NONE', #21597, 1000.000000000000227 ) ;
#24315 = CARTESIAN_POINT ( 'NONE',  ( -19.10440546280604934, -7.959287935654189461, 59.84604209533176089 ) ) ;
#24316 = CARTESIAN_POINT ( 'NONE',  ( -17.36015951656348832, -7.359395083792595216, 67.20534920880687935 ) ) ;
#24317 = FACE_OUTER_BOUND ( 'NONE', #371, .T. ) ;
#24318 = ORIENTED_EDGE ( 'NONE', *, *, #38034, .T. ) ;
#24319 = CARTESIAN_POINT ( 'NONE',  ( -36.42409385541304800, -9.159201730891741278, 50.49682052428079970 ) ) ;
#24320 = ORIENTED_EDGE ( 'NONE', *, *, #33371, .F. ) ;
#24321 = DIRECTION ( 'NONE',  ( -3.071710424422018668E-17, 6.404604876783312462E-16, 1.000000000000000000 ) ) ;
#24322 = CARTESIAN_POINT ( 'NONE',  ( -16.39887994223181167, -21.73372354711506560, 61.75568132718285597 ) ) ;
#24323 = EDGE_LOOP ( 'NONE', ( #26359, #42112, #10715, #34766, #47617 ) ) ;
#24324 = DIRECTION ( 'NONE',  ( -0.000000000000000000, -1.000000000000000000, -0.000000000000000000 ) ) ;
#24325 = CARTESIAN_POINT ( 'NONE',  ( -24.20601044598569374, -16.76383555912477874, 73.03903240339252534 ) ) ;
#24326 = FACE_OUTER_BOUND ( 'NONE', #28291, .T. ) ;
#24327 = ORIENTED_EDGE ( 'NONE', *, *, #5735, .T. ) ;
#24328 = CARTESIAN_POINT ( 'NONE',  ( -9.996238285358009179, -14.23362990587628296, 64.56616619773187438 ) ) ;
#24329 = CARTESIAN_POINT ( 'NONE',  ( -20.60942684424193772, -21.09890871138989965, 58.65947248567252359 ) ) ;
#24330 = EDGE_CURVE ( 'NONE', #29080, #12494, #26126, .T. ) ;
#24331 = CARTESIAN_POINT ( 'NONE',  ( -22.27163966896734593, -9.151951230621104827, 59.91509514496314637 ) ) ;
#24332 = ORIENTED_EDGE ( 'NONE', *, *, #30908, .F. ) ;
#24333 = CARTESIAN_POINT ( 'NONE',  ( -11.46028008028683942, -18.56947564720590194, 61.56238700194530367 ) ) ;
#24334 = EDGE_CURVE ( 'NONE', #16426, #2092, #48274, .T. ) ;
#24335 = ORIENTED_EDGE ( 'NONE', *, *, #39217, .F. ) ;
#24336 = VERTEX_POINT ( 'NONE', #29565 ) ;
#24337 = DIRECTION ( 'NONE',  ( 0.000000000000000000, 1.000000000000000000, -0.000000000000000000 ) ) ;
#24338 = CARTESIAN_POINT ( 'NONE',  ( -17.61266704711333375, -10.12650194148654137, 49.52966884056655772 ) ) ;
#24340 = CARTESIAN_POINT ( 'NONE',  ( -10.42558330013516255, -14.65956652655194503, 71.62782690272038622 ) ) ;
#24339 = AXIS2_PLACEMENT_3D ( 'NONE', #48061, #14775, #11128 ) ;
#24341 = CARTESIAN_POINT ( 'NONE',  ( -19.54284385650551670, -8.811426318492348031, 52.18089403414751359 ) ) ;
#24342 = CARTESIAN_POINT ( 'NONE',  ( -45.92409385541306222, -14.20920654474410760, 70.50000000000000000 ) ) ;
#24343 = CARTESIAN_POINT ( 'NONE',  ( -10.21764033814386963, -12.91954908504599331, 67.92327745040803677 ) ) ;
#24344 = CIRCLE ( 'NONE', #28277, 5.249999999999998224 ) ;
#24345 = AXIS2_PLACEMENT_3D ( 'NONE', #27829, #12569, #32011 ) ;
#24346 = CARTESIAN_POINT ( 'NONE',  ( -13.91686280105865947, -8.236299372188803147, 74.31459218752463869 ) ) ;
#24347 = VERTEX_POINT ( 'NONE', #14036 ) ;
#24348 = ORIENTED_EDGE ( 'NONE', *, *, #13669, .F. ) ;
#24349 = ADVANCED_FACE ( 'NONE', ( #2503 ), #44595, .T. ) ;
#24350 = CARTESIAN_POINT ( 'NONE',  ( -22.94085508618206859, -9.802298960702817254, 70.19673832247809742 ) ) ;
#24351 = CARTESIAN_POINT ( 'NONE',  ( 0.000000000000000000, 0.000000000000000000, 0.000000000000000000 ) ) ;
#24352 = EDGE_CURVE ( 'NONE', #29632, #188, #41264, .T. ) ;
#24353 = LINE ( 'NONE', #5153, #23646 ) ;
#24354 = DIRECTION ( 'NONE',  ( 0.000000000000000000, 0.000000000000000000, -1.000000000000000000 ) ) ;
#24355 = VECTOR ( 'NONE', #15579, 1000.000000000000000 ) ;
#24356 = CARTESIAN_POINT ( 'NONE',  ( -13.35550522631041837, -8.568183888810063209, 57.15463030501995689 ) ) ;
#24357 = CARTESIAN_POINT ( 'NONE',  ( -11.12358174778395714, -11.75903488045733347, 71.38860871064898106 ) ) ;
#24358 = ADVANCED_FACE ( 'NONE', ( #15498 ), #26612, .T. ) ;
#24359 = ORIENTED_EDGE ( 'NONE', *, *, #32338, .F. ) ;
#24360 = CARTESIAN_POINT ( 'NONE',  ( -22.95183339692489710, -10.43328498706183360, 63.07745801613410919 ) ) ;
#24361 = CARTESIAN_POINT ( 'NONE',  ( -20.66696756681432490, -21.06910030335248152, 58.64475164910061267 ) ) ;
#24362 = FACE_OUTER_BOUND ( 'NONE', #18604, .T. ) ;
#24363 = CARTESIAN_POINT ( 'NONE',  ( -13.91784385541274460, -6.860780111191973063, 51.02154966934469371 ) ) ;
#24364 = ORIENTED_EDGE ( 'NONE', *, *, #17512, .T. ) ;
#24365 = B_SPLINE_CURVE_WITH_KNOTS ( 'NONE', 3,
 ( #41537, #38068, #30227, #41051, #4354, #45251, #45013, #48426, #26272, #11493 ),
 .UNSPECIFIED., .F., .F.,
 ( 4, 2, 2, 2, 4 ),
 ( 0.6272669072877629093, 0.7522669073072766333, 0.8772669073267902462, 1.002266907346303970, 1.127266907365817694 ),
 .UNSPECIFIED. ) ;
#24366 = B_SPLINE_CURVE_WITH_KNOTS ( 'NONE', 3,
 ( #41209, #40253, #10458, #25465, #40475, #18057, #26436, #41445, #45401, #7744 ),
 .UNSPECIFIED., .F., .F.,
 ( 4, 2, 2, 2, 4 ),
 ( 0.000000000000000000, 0.2500000000000000000, 0.5000000000000000000, 0.7500000000000000000, 1.000000000000000000 ),
 .UNSPECIFIED. ) ;
#24367 = CARTESIAN_POINT ( 'NONE',  ( -30.42409385541305156, -8.109206544744111511, 50.50000000000000000 ) ) ;
#24368 = B_SPLINE_CURVE_WITH_KNOTS ( 'NONE', 3,
 ( #30001, #48212, #21867, #11519, #7846, #25564, #26540, #10785, #11037, #25807 ),
 .UNSPECIFIED., .F., .F.,
 ( 4, 2, 2, 2, 4 ),
 ( 0.000000000000000000, 0.2500000000000000000, 0.5000000000000000000, 0.7500000000000000000, 1.000000000000000000 ),
 .UNSPECIFIED. ) ;
#24369 = DIRECTION ( 'NONE',  ( 0.000000000000000000, 0.007114381193220190198, -0.9999746924698832418 ) ) ;
#24370 = CARTESIAN_POINT ( 'NONE',  ( -12.78905762515450917, -9.563515353937917851, 74.33425404606212794 ) ) ;
#24371 = VECTOR ( 'NONE', #36147, 1000.000000000000114 ) ;
#24372 = CARTESIAN_POINT ( 'NONE',  ( -8.424093855413071097, -8.109206544744111511, 51.75000000000000000 ) ) ;
#24373 = DIRECTION ( 'NONE',  ( -0.3824554607245533866, 0.9239739285077094300, -8.917814418161383551E-09 ) ) ;
#24374 = CARTESIAN_POINT ( 'NONE',  ( -21.18000274887674905, -20.77541536365158592, 69.05450184741354747 ) ) ;
#24375 = ORIENTED_EDGE ( 'NONE', *, *, #25328, .F. ) ;
#24376 = CARTESIAN_POINT ( 'NONE',  ( -13.30064747678972203, -9.086267117603348709, 67.67943031933630493 ) ) ;
#24377 = VECTOR ( 'NONE', #12710, 1000.000000000000000 ) ;
#24378 = EDGE_LOOP ( 'NONE', ( #34984, #3817, #23111, #7596 ) ) ;
#24379 = CARTESIAN_POINT ( 'NONE',  ( -10.23981800866728342, -12.83659613830724489, 67.87799002222476474 ) ) ;
#24380 = FACE_OUTER_BOUND ( 'NONE', #16378, .T. ) ;
#24381 = VERTEX_POINT ( 'NONE', #8382 ) ;
#24382 = CARTESIAN_POINT ( 'NONE',  ( -18.39951258112534305, -22.19516185762106275, 69.00009993223443416 ) ) ;
#24383 = CARTESIAN_POINT ( 'NONE',  ( -11.42104402874289804, -10.39690533886297885, 74.59918334245951144 ) ) ;
#24384 = ORIENTED_EDGE ( 'NONE', *, *, #36939, .T. ) ;
#24385 = CARTESIAN_POINT ( 'NONE',  ( -10.56627859465609376, -16.21290490039525167, 71.44750383612122846 ) ) ;
#24386 = VECTOR ( 'NONE', #23133, 1000.000000000000227 ) ;
#24387 = ADVANCED_FACE ( 'NONE', ( #45097 ), #23406, .F. ) ;
#24388 = CARTESIAN_POINT ( 'NONE',  ( -15.03263910315855512, -8.176888424288380364, 56.86472059657746314 ) ) ;
#24389 = ORIENTED_EDGE ( 'NONE', *, *, #40147, .F. ) ;
#24390 = PLANE ( 'NONE',  #42804 ) ;
#24391 = DIRECTION ( 'NONE',  ( 0.000000000000000000, 1.000000000000000000, 0.000000000000000000 ) ) ;
#24392 = CARTESIAN_POINT ( 'NONE',  ( -24.59934351769828709, -12.80445480200731012, 66.40908417132197883 ) ) ;
#24393 = FACE_OUTER_BOUND ( 'NONE', #23593, .T. ) ;
#24395 = ORIENTED_EDGE ( 'NONE', *, *, #22351, .F. ) ;
#24394 = AXIS2_PLACEMENT_3D ( 'NONE', #14111, #19906, #47408 ) ;
#24396 = VERTEX_POINT ( 'NONE', #26866 ) ;
#24397 = CARTESIAN_POINT ( 'NONE',  ( -22.67545590913884013, -19.51856332474398670, 72.64400582244574878 ) ) ;
#24398 = DIRECTION ( 'NONE',  ( -0.4251432040024066272, -0.9051260995521939190, -1.185120001106687566E-09 ) ) ;
#24399 = ORIENTED_EDGE ( 'NONE', *, *, #186, .T. ) ;
#24400 = CARTESIAN_POINT ( 'NONE',  ( -16.20274916913749408, -7.857711080649619539, 67.28440454693885897 ) ) ;
#24401 = CARTESIAN_POINT ( 'NONE',  ( -21.81751094647485445, -9.290807395701664362, 59.72171140566239700 ) ) ;
#24402 = CARTESIAN_POINT ( 'NONE',  ( -19.40534385759799463, -7.595227055684746986, 51.75156210489594599 ) ) ;
#24403 = CARTESIAN_POINT ( 'NONE',  ( -23.81054795188011397, -10.97308734706811428, 73.56204507097986323 ) ) ;
#24404 = CARTESIAN_POINT ( 'NONE',  ( -24.25070531508703553, -16.58426240227147375, 59.21512694191572024 ) ) ;
#24405 = DIRECTION ( 'NONE',  ( -3.413470714839332458E-33, 1.190614954331866791E-16, -1.000000000000000000 ) ) ;
#24406 = EDGE_LOOP ( 'NONE', ( #3189, #26008, #42257, #37534, #46681 ) ) ;
#24407 = CARTESIAN_POINT ( 'NONE',  ( -16.57554779340669882, -22.21081089906203943, 65.41059674993448425 ) ) ;
#24408 = CARTESIAN_POINT ( 'NONE',  ( -10.42615540542738195, -15.66473329960067140, 61.33789027493194368 ) ) ;
#24409 = EDGE_CURVE ( 'NONE', #14239, #37402, #3681, .T. ) ;
#24410 = AXIS2_PLACEMENT_3D ( 'NONE', #39624, #6620, #36154 ) ;
#24411 = CARTESIAN_POINT ( 'NONE',  ( -23.95183236677831928, -17.48193434775220823, 69.71339772309136151 ) ) ;
#24412 = CARTESIAN_POINT ( 'NONE',  ( -19.78614017500849087, -21.39864787494504839, 68.93482476778672208 ) ) ;
#24413 = CARTESIAN_POINT ( 'NONE',  ( -10.79250418411942292, -11.41415947502061456, 67.74051841629483306 ) ) ;
#24414 = EDGE_CURVE ( 'NONE', #40988, #19087, #9535, .T. ) ;
#24415 =( BOUNDED_CURVE ( )  B_SPLINE_CURVE ( 3, ( #30735, #14940, #29750, #26538 ),
 .UNSPECIFIED., .F., .F. ) 
 B_SPLINE_CURVE_WITH_KNOTS ( ( 4, 4 ),
 ( 0.9074455897393687298, 1.000000000000000000 ),
 .UNSPECIFIED. ) 
 CURVE ( )  GEOMETRIC_REPRESENTATION_ITEM ( )  RATIONAL_B_SPLINE_CURVE ( ( 0.6983129098261068313, 0.7760317562607100816, 0.8765941196520078416, 1.000000000000000000 ) ) 
 REPRESENTATION_ITEM ( '' )  );
#24416 = AXIS2_PLACEMENT_3D ( 'NONE', #10300, #44049, #33395 ) ;
#24417 = ORIENTED_EDGE ( 'NONE', *, *, #33248, .F. ) ;
#24418 = VERTEX_POINT ( 'NONE', #510 ) ;
#24419 = ADVANCED_FACE ( 'NONE', ( #46052 ), #45589, .T. ) ;
#24420 = VERTEX_POINT ( 'NONE', #27091 ) ;
#24421 = CARTESIAN_POINT ( 'NONE',  ( -11.14114473067313682, -10.80566704772025233, 57.32407823191172014 ) ) ;
#24422 = CARTESIAN_POINT ( 'NONE',  ( -23.64049396042644702, -11.59094511257166360, 63.02506373711870680 ) ) ;
#24423 = PLANE ( 'NONE',  #2476 ) ;
#24424 = B_SPLINE_CURVE_WITH_KNOTS ( 'NONE', 1,
 ( #44889, #41173 ),
 .UNSPECIFIED., .F., .F.,
 ( 2, 2 ),
 ( 0.000000000000000000, 1.000000000000000000 ),
 .UNSPECIFIED. ) ;
#24425 = VECTOR ( 'NONE', #41474, 1000.000000000000114 ) ;
#24426 = ADVANCED_FACE ( 'NONE', ( #27 ), #32475, .T. ) ;
#24427 = ORIENTED_EDGE ( 'NONE', *, *, #29866, .T. ) ;
#24428 = EDGE_CURVE ( 'NONE', #15180, #32458, #48576, .T. ) ;
#24429 =( BOUNDED_CURVE ( )  B_SPLINE_CURVE ( 3, ( #4472, #39172, #31068, #8670 ),
 .UNSPECIFIED., .F., .F. ) 
 B_SPLINE_CURVE_WITH_KNOTS ( ( 4, 4 ),
 ( 0.4074455897393673975, 0.5000000000000000000 ),
 .UNSPECIFIED. ) 
 CURVE ( )  GEOMETRIC_REPRESENTATION_ITEM ( )  RATIONAL_B_SPLINE_CURVE ( ( 0.6983129098260982826, 0.7760317562607005337, 0.8765941196520004031, 0.9999999999999964473 ) ) 
 REPRESENTATION_ITEM ( '' )  );
#24430 = CARTESIAN_POINT ( 'NONE',  ( -41.28806444364835215, -14.90920654474426499, 72.08823529411763786 ) ) ;
#24431 = CARTESIAN_POINT ( 'NONE',  ( -10.40860991809309155, -15.50898095412354571, 57.85320721669017985 ) ) ;
#24432 = ORIENTED_EDGE ( 'NONE', *, *, #19290, .F. ) ;
#24433 = DIRECTION ( 'NONE',  ( -0.7700094066334561838, -0.6380325334150231953, 0.000000000000000000 ) ) ;
#24434 = CARTESIAN_POINT ( 'NONE',  ( -19.56272746357835501, -21.53536514712069305, 58.68074270823246508 ) ) ;
#24435 = B_SPLINE_CURVE_WITH_KNOTS ( 'NONE', 1,
 ( #36824, #3356 ),
 .UNSPECIFIED., .F., .F.,
 ( 2, 2 ),
 ( 0.000000000000000000, 1.000000000000000000 ),
 .UNSPECIFIED. ) ;
#24436 = VERTEX_POINT ( 'NONE', #30804 ) ;
#24437 = CARTESIAN_POINT ( 'NONE',  ( -21.89826263122328953, -8.852228171720549099, 66.84645388252840803 ) ) ;
#24438 = ORIENTED_EDGE ( 'NONE', *, *, #16951, .F. ) ;
#24439 = CARTESIAN_POINT ( 'NONE',  ( -10.55435033023172764, -13.22452456802019327, 71.50268769994818285 ) ) ;
#24440 = VERTEX_POINT ( 'NONE', #19711 ) ;
#24441 = CARTESIAN_POINT ( 'NONE',  ( -24.47371109942907808, -14.90716652360855754, 59.25772288469824645 ) ) ;
#24442 = CARTESIAN_POINT ( 'NONE',  ( -20.72574062298286179, -8.580111251864034116, 59.84125250080548852 ) ) ;
#24443 = DIRECTION ( 'NONE',  ( -0.5652317888644006194, -0.8249321334856242194, 7.911723905267717726E-08 ) ) ;
#24444 = ORIENTED_EDGE ( 'NONE', *, *, #42800, .F. ) ;
#24445 = DIRECTION ( 'NONE',  ( 0.9687793358424821033, -0.2479245821708677133, 0.000000000000000000 ) ) ;
#24446 = DIRECTION ( 'NONE',  ( -5.731567514496413899E-31, -1.020425574103664789E-16, -1.000000000000000000 ) ) ;
#24447 = CARTESIAN_POINT ( 'NONE',  ( -22.10033346171958257, -20.08913226167895871, 58.64954131300479645 ) ) ;
#24448 = AXIS2_PLACEMENT_3D ( 'NONE', #45827, #18983, #33987 ) ;
#24449 = EDGE_CURVE ( 'NONE', #21913, #43447, #18977, .T. ) ;
#24450 = CARTESIAN_POINT ( 'NONE',  ( 10.57590614458695377, 1.890747609047609190, 50.53028072113853142 ) ) ;
#24451 = CARTESIAN_POINT ( 'NONE',  ( -21.18536505927766456, -21.24010891514583221, 65.84099883884408655 ) ) ;
#24452 = DIRECTION ( 'NONE',  ( -0.8201047403141394909, 0.5722134347551369737, 7.883065731424289661E-08 ) ) ;
#24453 = EDGE_LOOP ( 'NONE', ( #5258, #29141, #5187, #1827 ) ) ;
#24454 = AXIS2_PLACEMENT_3D ( 'NONE', #13665, #28712, #35840 ) ;
#24455 = FACE_OUTER_BOUND ( 'NONE', #8209, .T. ) ;
#24456 = CARTESIAN_POINT ( 'NONE',  ( -24.67067787691205893, -13.07946411363355388, 62.99410723793601363 ) ) ;
#24457 = CARTESIAN_POINT ( 'NONE',  ( -24.35706380436459995, -15.77560588608014136, 69.83307488757523629 ) ) ;
#24458 = DIRECTION ( 'NONE',  ( -0.7300417127692488961, -0.6834025882427879894, -6.612978995310452690E-09 ) ) ;
#24459 = CARTESIAN_POINT ( 'NONE',  ( -19.90432934692537614, -21.83431937171774706, 69.04987052938618319 ) ) ;
#24460 = CARTESIAN_POINT ( 'NONE',  ( -16.11159385650551457, -6.922745924619793101, 51.69366785382590024 ) ) ;
#24461 = ORIENTED_EDGE ( 'NONE', *, *, #43640, .T. ) ;
#24462 = CARTESIAN_POINT ( 'NONE',  ( -16.26183769579148475, -7.855670737815882987, 60.50028478907630358 ) ) ;
#24463 = CARTESIAN_POINT ( 'NONE',  ( -50.42609385541305755, -14.90920654474423301, 69.07058823529411029 ) ) ;
#24464 = ORIENTED_EDGE ( 'NONE', *, *, #21330, .T. ) ;
#24465 = CARTESIAN_POINT ( 'NONE',  ( -9.975558569371616002, -14.65758674969880104, 71.58428599250275681 ) ) ;
#24466 = CARTESIAN_POINT ( 'NONE',  ( -10.62784674774485971, -13.13233953042942304, 67.96505635084706398 ) ) ;
#24467 = TOROIDAL_SURFACE ( 'NONE', #3206, 1.500000000000008660, 0.5000000000000000000 ) ;
#24468 = CARTESIAN_POINT ( 'NONE',  ( -14.62687775177895766, -8.392386291203132842, 63.78978840643812021 ) ) ;
#24469 = CARTESIAN_POINT ( 'NONE',  ( -19.10440546280604934, -7.959287935654189461, 59.84604209533176089 ) ) ;
#24470 = CARTESIAN_POINT ( 'NONE',  ( -24.82869252881341637, -15.63043612719190811, 73.15303745911135991 ) ) ;
#24471 = ORIENTED_EDGE ( 'NONE', *, *, #32046, .F. ) ;
#24472 = B_SPLINE_CURVE_WITH_KNOTS ( 'NONE', 1,
 ( #20278, #13346 ),
 .UNSPECIFIED., .F., .F.,
 ( 2, 2 ),
 ( 0.000000000000000000, 1.000000000000000000 ),
 .UNSPECIFIED. ) ;
#24473 = B_SPLINE_CURVE_WITH_KNOTS ( 'NONE', 3,
 ( #2387, #31217, #23844, #38844, #25761, #6575, #6327, #21360, #25519, #17401 ),
 .UNSPECIFIED., .F., .F.,
 ( 4, 2, 2, 2, 4 ),
 ( 0.6272669072878317431, 0.7522669073073130486, 0.8772669073267944650, 1.002266907346275771, 1.127266907365757076 ),
 .UNSPECIFIED. ) ;
#24474 = EDGE_CURVE ( 'NONE', #39405, #31233, #30322, .T. ) ;
#24475 = CARTESIAN_POINT ( 'NONE',  ( -24.41273135550727957, -14.40837812317847977, 66.48292728376772232 ) ) ;
#24476 = CARTESIAN_POINT ( 'NONE',  ( -13.68201746596516699, -21.25120652447435532, 68.60625134287384697 ) ) ;
#24477 = FACE_OUTER_BOUND ( 'NONE', #42635, .T. ) ;
#24478 = ORIENTED_EDGE ( 'NONE', *, *, #25344, .T. ) ;
#24479 = VECTOR ( 'NONE', #37867, 1000.000000000000114 ) ;
#24480 = CARTESIAN_POINT ( 'NONE',  ( -23.48885007022674998, -11.31111499345109195, 73.59023240731526982 ) ) ;
#24481 = CARTESIAN_POINT ( 'NONE',  ( -24.23813412381375088, -12.99935709875259704, 66.31718868320673721 ) ) ;
#24482 = CARTESIAN_POINT ( 'NONE',  ( -13.80520660347273854, -20.80124399317547201, 65.27163466030602024 ) ) ;
#24483 = DIRECTION ( 'NONE',  ( 0.02400335114476204526, -0.9997118780597843424, -1.529429985666831130E-10 ) ) ;
#24484 = ORIENTED_EDGE ( 'NONE', *, *, #30640, .F. ) ;
#24485 = EDGE_LOOP ( 'NONE', ( #14178, #45195 ) ) ;
#24486 = CARTESIAN_POINT ( 'NONE',  ( -18.02409385541303877, -9.359200813967568422, 50.49621490985803263 ) ) ;
#24487 = ADVANCED_FACE ( 'NONE', ( #37418 ), #45333, .T. ) ;
#24488 = AXIS2_PLACEMENT_3D ( 'NONE', #44570, #21674, #18690 ) ;
#24489 = CARTESIAN_POINT ( 'NONE',  ( -21.21476609527666923, -21.22273158816933858, 65.73453942127412120 ) ) ;
#24490 = EDGE_CURVE ( 'NONE', #9114, #30036, #3016, .T. ) ;
#24491 = VECTOR ( 'NONE', #3921, 1000.000000000000000 ) ;
#24492 = CARTESIAN_POINT ( 'NONE',  ( -15.41750689856725565, -7.634439986883705842, 74.33631595678771475 ) ) ;
#24493 = EDGE_CURVE ( 'NONE', #1460, #39153, #5420, .T. ) ;
#24494 = CARTESIAN_POINT ( 'NONE',  ( -15.32409385541304481, -9.359200813967568422, 50.49621490985804684 ) ) ;
#24495 = CARTESIAN_POINT ( 'NONE',  ( -14.13966730279324935, -8.627577120331476834, 70.92060855097744820 ) ) ;
#24496 = DIRECTION ( 'NONE',  ( -1.000000000000000000, 1.224646799147353207E-16, 5.551115123125782702E-17 ) ) ;
#24497 = ORIENTED_EDGE ( 'NONE', *, *, #7164, .T. ) ;
#24498 = CARTESIAN_POINT ( 'NONE',  ( -11.35824856342118316, -11.21643317443627197, 60.97885780702567615 ) ) ;
#24499 = AXIS2_PLACEMENT_3D ( 'NONE', #36728, #48319, #3017 ) ;
#24500 = DIRECTION ( 'NONE',  ( 1.000000000000000000, -4.164305804376849172E-17, 1.614929280266638808E-16 ) ) ;
#24501 = EDGE_LOOP ( 'NONE', ( #36330, #15274, #4410, #183, #34973 ) ) ;
#24502 = FACE_OUTER_BOUND ( 'NONE', #27189, .T. ) ;
#24503 = ADVANCED_FACE ( 'NONE', ( #28055 ), #43080, .T. ) ;
#24504 = CARTESIAN_POINT ( 'NONE',  ( -23.66133310609451712, -18.88359296917171903, 69.40876596050124192 ) ) ;
#24505 = ADVANCED_FACE ( 'NONE', ( #1956 ), #13027, .T. ) ;
#24506 = ORIENTED_EDGE ( 'NONE', *, *, #9953, .F. ) ;
#24507 = DIRECTION ( 'NONE',  ( 3.549360974551883545E-17, -6.371834667872732552E-18, -1.000000000000000000 ) ) ;
#24508 = CARTESIAN_POINT ( 'NONE',  ( -18.54255121075907553, -21.71939966792950116, 72.28510895949058579 ) ) ;
#24509 = ADVANCED_FACE ( 'NONE', ( #13259 ), #23658, .T. ) ;
#24511 = EDGE_CURVE ( 'NONE', #22634, #17712, #21315, .T. ) ;
#24510 = ORIENTED_EDGE ( 'NONE', *, *, #43377, .T. ) ;
#24512 = DIRECTION ( 'NONE',  ( -0.9243256318339801991, 0.3816046728418207024, -8.614662759602030584E-09 ) ) ;
#24513 = DIRECTION ( 'NONE',  ( -3.071710424422018668E-17, 6.404604876783312462E-16, 1.000000000000000000 ) ) ;
#24514 = DIRECTION ( 'NONE',  ( 0.9687793358424821033, -0.2479245821708677133, 0.000000000000000000 ) ) ;
#24515 = CARTESIAN_POINT ( 'NONE',  ( -11.03124136535102373, -17.66077402989073875, 71.56718193465405875 ) ) ;
#24516 = ORIENTED_EDGE ( 'NONE', *, *, #19245, .T. ) ;
#24517 = PLANE ( 'NONE',  #26018 ) ;
#24518 = CARTESIAN_POINT ( 'NONE',  ( -22.34365193135296579, -19.87012687442179981, 62.39006291346853317 ) ) ;
#24519 = CARTESIAN_POINT ( 'NONE',  ( -24.51735291603774058, -12.52900075589524498, 69.88587656176791540 ) ) ;
#24520 = DIRECTION ( 'NONE',  ( -2.654446660633206478E-06, 3.134491597800584759E-06, -0.9999999999915644144 ) ) ;
#24521 = ITEM_DEFINED_TRANSFORMATION ( 'NONE', 'NONE', #10179,  #29031 ) ;
#24522 = MECHANICAL_DESIGN_GEOMETRIC_PRESENTATION_REPRESENTATION (  '', ( #45756 ), #27628 ) ;
#24523 = CARTESIAN_POINT ( 'NONE',  ( -22.10677449762105340, -15.19398901379252820, 49.52966884056655772 ) ) ;
#24524 = CARTESIAN_POINT ( 'NONE',  ( -17.43166475307565122, -7.359124600834268115, 67.13544264266099049 ) ) ;
#24525 = AXIS2_PLACEMENT_3D ( 'NONE', #1071, #30884, #20273 ) ;
#24526 = FACE_OUTER_BOUND ( 'NONE', #19871, .T. ) ;
#24527 = VERTEX_POINT ( 'NONE', #16718 ) ;
#24528 = FACE_OUTER_BOUND ( 'NONE', #24750, .T. ) ;
#24529 = CARTESIAN_POINT ( 'NONE',  ( -20.10829901998359759, -21.75890299870832578, 72.59817030071424426 ) ) ;
#24530 = CARTESIAN_POINT ( 'NONE',  ( -10.00194981992954801, -15.45342389922025639, 57.76131113159441810 ) ) ;
#24531 = ORIENTED_EDGE ( 'NONE', *, *, #13142, .T. ) ;
#24532 = DIRECTION ( 'NONE',  ( 0.8967515337576289491, -0.4425343904188010491, 9.546469656967252871E-09 ) ) ;
#24533 = ORIENTED_EDGE ( 'NONE', *, *, #19500, .F. ) ;
#24534 = EDGE_CURVE ( 'NONE', #25477, #10558, #7177, .T. ) ;
#24535 = ORIENTED_EDGE ( 'NONE', *, *, #13537, .T. ) ;
#24536 = VERTEX_POINT ( 'NONE', #46553 ) ;
#24537 = CARTESIAN_POINT ( 'NONE',  ( -13.94586905867137361, -20.88575599516291703, 72.11534825290704021 ) ) ;
#24538 = AXIS2_PLACEMENT_3D ( 'NONE', #13961, #44061, #36862 ) ;
#24539 = CARTESIAN_POINT ( 'NONE',  ( -45.92409385541306222, -14.20920654474410760, 70.50000000000000000 ) ) ;
#24540 = DIRECTION ( 'NONE',  ( -3.071710424422018668E-17, 6.404604876783312462E-16, 1.000000000000000000 ) ) ;
#24541 = CARTESIAN_POINT ( 'NONE',  ( -16.98991503782990975, -22.24662993548692214, 72.35038528954983406 ) ) ;
#24542 = CARTESIAN_POINT ( 'NONE',  ( -16.29760673242258306, -22.17363489859456038, 61.87072740723333197 ) ) ;
#24543 = ORIENTED_EDGE ( 'NONE', *, *, #39217, .T. ) ;
#24544 = EDGE_LOOP ( 'NONE', ( #957, #34223, #24676 ) ) ;
#24545 = CARTESIAN_POINT ( 'NONE',  ( -19.79909385650551457, -8.114302828567740988, 52.18300498402516041 ) ) ;
#24546 = AXIS2_PLACEMENT_3D ( 'NONE', #38222, #4506, #11653 ) ;
#24547 = DIRECTION ( 'NONE',  ( -0.6771828760946864145, 0.7358147540815750398, -3.419290845356464415E-09 ) ) ;
#24548 = LINE ( 'NONE', #39543, #6482 ) ;
#24549 = CARTESIAN_POINT ( 'NONE',  ( -13.86159385650551812, -9.295667164867525756, 49.30633214617472504 ) ) ;
#24550 = VERTEX_POINT ( 'NONE', #38658 ) ;
#24551 = CARTESIAN_POINT ( 'NONE',  ( -14.75750412239355391, -21.76563565968240965, 61.83611636703810177 ) ) ;
#24552 = CARTESIAN_POINT ( 'NONE',  ( -10.90759852523040507, -17.49952041063523822, 68.09721944423129969 ) ) ;
#24553 = VECTOR ( 'NONE', #15849, 999.9999999999998863 ) ;
#24554 = CARTESIAN_POINT ( 'NONE',  ( -22.09234551867295693, -20.09219114410425178, 62.53439162497838311 ) ) ;
#24555 =( BOUNDED_SURFACE ( )  B_SPLINE_SURFACE ( 3, 1, ( 
 ( #22638, #14711 ),
 ( #3671, #37635 ),
 ( #18678, #11313 ),
 ( #18938, #11804 ),
 ( #15223, #33951 ),
 ( #478, #45303 ),
 ( #15463, #45546 ) ),
 .UNSPECIFIED., .T., .F., .F. ) 
 B_SPLINE_SURFACE_WITH_KNOTS ( ( 4, 3, 4 ),
 ( 2, 2 ),
 ( 0.000000000000000000, 0.5000000000000000000, 1.000000000000000000 ),
 ( 0.000000000000000000, 1.000000000000000000 ),
 .UNSPECIFIED. ) 
 GEOMETRIC_REPRESENTATION_ITEM ( )  RATIONAL_B_SPLINE_SURFACE ( (
 ( 1.000000000000000000, 1.000000000000000000),
 ( 0.3333333333333335369, 0.3333333333333330373),
 ( 0.3333333333333335369, 0.3333333333333330373),
 ( 1.000000000000000000, 1.000000000000000000),
 ( 0.3333333333333333703, 0.3333333333333333703),
 ( 0.3333333333333333703, 0.3333333333333333703),
 ( 1.000000000000000000, 1.000000000000000000) ) ) 
 REPRESENTATION_ITEM ( '' )  SURFACE ( )  );
#24556 = ORIENTED_EDGE ( 'NONE', *, *, #35096, .F. ) ;
#24557 = CYLINDRICAL_SURFACE ( 'NONE', #25711, 0.1500000000000029088 ) ;
#24558 = CARTESIAN_POINT ( 'NONE',  ( -9.974456290884534226, -14.72748455880875795, 71.51278017970571454 ) ) ;
#24559 = CARTESIAN_POINT ( 'NONE',  ( -11.52461732454066023, -18.67456722079397125, 68.63178522425482697 ) ) ;
#24560 = ADVANCED_FACE ( 'NONE', ( #24380 ), #37480, .T. ) ;
#24561 = ADVANCED_FACE ( 'NONE', ( #31269 ), #42555, .T. ) ;
#24562 = CARTESIAN_POINT ( 'NONE',  ( -19.04042132780597996, -7.536568533962904048, 67.01576502235467103 ) ) ;
#24563 = ORIENTED_EDGE ( 'NONE', *, *, #26736, .T. ) ;
#24564 = CARTESIAN_POINT ( 'NONE',  ( -19.30746897944592888, -7.600422969554355923, 60.07437648108736994 ) ) ;
#24565 = CARTESIAN_POINT ( 'NONE',  ( -23.08009853854674986, -9.960157477770804846, 66.58536326842445874 ) ) ;
#24566 = EDGE_LOOP ( 'NONE', ( #15964, #46268, #20699, #8149, #35924 ) ) ;
#24567 = CARTESIAN_POINT ( 'NONE',  ( -24.45201643071094111, -14.25170847814747077, 69.65275273439885950 ) ) ;
#24568 =( BOUNDED_SURFACE ( )  B_SPLINE_SURFACE ( 3, 1, ( 
 ( #17089, #31891 ),
 ( #42740, #16851 ),
 ( #23789, #32138 ),
 ( #31403, #24524 ),
 ( #46435, #1606 ),
 ( #9008, #20326 ),
 ( #35085, #38789 ) ),
 .UNSPECIFIED., .T., .F., .F. ) 
 B_SPLINE_SURFACE_WITH_KNOTS ( ( 4, 3, 4 ),
 ( 2, 2 ),
 ( 0.000000000000000000, 0.5000000000000000000, 1.000000000000000000 ),
 ( 0.000000000000000000, 1.000000000000000000 ),
 .UNSPECIFIED. ) 
 GEOMETRIC_REPRESENTATION_ITEM ( )  RATIONAL_B_SPLINE_SURFACE ( (
 ( 1.000000000000000000, 1.000000000000000000),
 ( 0.3333333333333335369, 0.3333333333333330373),
 ( 0.3333333333333335369, 0.3333333333333330373),
 ( 1.000000000000000000, 1.000000000000000000),
 ( 0.3333333333333333703, 0.3333333333333333703),
 ( 0.3333333333333333703, 0.3333333333333333703),
 ( 1.000000000000000000, 1.000000000000000000) ) ) 
 REPRESENTATION_ITEM ( '' )  SURFACE ( )  );
#24569 = EDGE_LOOP ( 'NONE', ( #38462, #16237 ) ) ;
#24570 = DIRECTION ( 'NONE',  ( -1.081321489524789733E-05, -7.211308818607114576E-06, 0.9999999999155356756 ) ) ;
#24571 = ADVANCED_FACE ( 'NONE', ( #29696 ), #15144, .T. ) ;
#24572 = ADVANCED_FACE ( 'NONE', ( #37807 ), #44251, .T. ) ;
#24573 = CARTESIAN_POINT ( 'NONE',  ( -10.37541943412130863, -14.96049300415475436, 75.08306784598362071 ) ) ;
#24574 = EDGE_LOOP ( 'NONE', ( #24484, #29473 ) ) ;
#24575 = CARTESIAN_POINT ( 'NONE',  ( -14.62687775177895766, -8.392386291203132842, 63.78978840643812021 ) ) ;
#24576 = CARTESIAN_POINT ( 'NONE',  ( -20.20125106709443585, -21.29320546917908885, 72.40478744281909940 ) ) ;
#24577 = CARTESIAN_POINT ( 'NONE',  ( -16.93941734680483080, -7.775588144984237005, 74.24546186738449194 ) ) ;
#24578 = CARTESIAN_POINT ( 'NONE',  ( -21.17181896469314140, -21.24811525286444436, 65.74600479234126738 ) ) ;
#24579 = ORIENTED_EDGE ( 'NONE', *, *, #22919, .F. ) ;
#24580 = CARTESIAN_POINT ( 'NONE',  ( -11.01197672498280866, -17.74032467813711378, 71.85246142747085685 ) ) ;
#24581 = CARTESIAN_POINT ( 'NONE',  ( -20.82063550681992226, -21.43998110257799539, 58.90121085131534784 ) ) ;
#24582 = CARTESIAN_POINT ( 'NONE',  ( -14.10256395084115866, -8.140532207465255965, 70.84462205307964666 ) ) ;
#24583 = ORIENTED_EDGE ( 'NONE', *, *, #31158, .F. ) ;
#24584 = CARTESIAN_POINT ( 'NONE',  ( -10.61354641423966783, -11.78914506505660675, 74.68027500694958576 ) ) ;
#24585 =( BOUNDED_CURVE ( )  B_SPLINE_CURVE ( 3, ( #19571, #24006, #42948, #45922 ),
 .UNSPECIFIED., .F., .F. ) 
 B_SPLINE_CURVE_WITH_KNOTS ( ( 4, 4 ),
 ( 4.712388980384691450, 4.921828490624017505 ),
 .UNSPECIFIED. ) 
 CURVE ( )  GEOMETRIC_REPRESENTATION_ITEM ( )  RATIONAL_B_SPLINE_CURVE ( ( 1.000000000000000000, 0.9963479302455153785, 0.9963479302455153785, 1.000000000000000000 ) ) 
 REPRESENTATION_ITEM ( '' )  );
#24586 = B_SPLINE_CURVE_WITH_KNOTS ( 'NONE', 1,
 ( #9281, #38580 ),
 .UNSPECIFIED., .F., .F.,
 ( 2, 2 ),
 ( 0.000000000000000000, 1.000000000000000000 ),
 .UNSPECIFIED. ) ;
#24587 = CARTESIAN_POINT ( 'NONE',  ( -12.77796340496265692, -17.75258416873320400, 53.49899999999994549 ) ) ;
#24588 = EDGE_CURVE ( 'NONE', #22272, #23931, #25753, .T. ) ;
#24589 = EDGE_LOOP ( 'NONE', ( #13468, #5486, #32396, #7519, #23415 ) ) ;
#24590 = VERTEX_POINT ( 'NONE', #26009 ) ;
#24591 = CARTESIAN_POINT ( 'NONE',  ( -14.74690658000796439, -21.27702444416618732, 58.16617884968206198 ) ) ;
#24592 = DIRECTION ( 'NONE',  ( -0.5540494244615070674, 0.8324837747691379297, -2.496966302803655883E-17 ) ) ;
#24593 = CARTESIAN_POINT ( 'NONE',  ( -19.85909425162068942, -21.37257694502213567, 72.64634926892956912 ) ) ;
#24594 = CARTESIAN_POINT ( 'NONE',  ( -20.04909385650551457, -8.104110260919579645, 48.81699501597546487 ) ) ;
#24595 = DIRECTION ( 'NONE',  ( 1.000000000000000000, -4.164305804376849788E-17, 1.614929280266638808E-16 ) ) ;
#24596 = DIRECTION ( 'NONE',  ( 9.588441152175118139E-09, 2.115493544230230216E-07, 0.9999999999999775735 ) ) ;
#24597 = CARTESIAN_POINT ( 'NONE',  ( -23.77312829587014420, -18.70709569252041859, 72.87872954713984086 ) ) ;
#24598 = DIRECTION ( 'NONE',  ( -0.9118114225829225816, -0.4106092176842893182, -5.589476761700638731E-08 ) ) ;
#24599 = CARTESIAN_POINT ( 'NONE',  ( -16.72074880447151202, -22.22598103032179395, 68.88898962838827345 ) ) ;
#24600 = ORIENTED_EDGE ( 'NONE', *, *, #27890, .F. ) ;
#24601 = VERTEX_POINT ( 'NONE', #45225 ) ;
#24602 = CARTESIAN_POINT ( 'NONE',  ( -11.03149232240643052, -10.98320184173030256, 60.93531726291125494 ) ) ;
#24603 = CARTESIAN_POINT ( 'NONE',  ( -22.80534385541300324, -7.595227055684715900, 51.75156210489603126 ) ) ;
#24604 = CARTESIAN_POINT ( 'NONE',  ( -19.77283897654775657, -21.87935945976245122, 65.50840285157048015 ) ) ;
#24605 = CARTESIAN_POINT ( 'NONE',  ( -14.33701861991839976, -19.05567172067550530, 50.77966884056656482 ) ) ;
#24606 = CARTESIAN_POINT ( 'NONE',  ( -20.72450927900464634, -21.03929139025763106, 58.93003081252663833 ) ) ;
#24607 = CARTESIAN_POINT ( 'NONE',  ( -21.39909385650551599, -8.114302828567740988, 52.18300498402516041 ) ) ;
#24608 = ORIENTED_EDGE ( 'NONE', *, *, #16957, .F. ) ;
#24609 = CARTESIAN_POINT ( 'NONE',  ( -15.09857480863590062, -8.145354156905789011, 60.46428990550709415 ) ) ;
#24610 = CARTESIAN_POINT ( 'NONE',  ( -11.07163856976715977, -18.70144880307400470, 61.47049154680724570 ) ) ;
#24611 = ORIENTED_EDGE ( 'NONE', *, *, #24191, .T. ) ;
#24612 = CARTESIAN_POINT ( 'NONE',  ( -11.17855950479832927, -18.87086615690261482, 64.86211796126700335 ) ) ;
#24613 = DIRECTION ( 'NONE',  ( 3.413470714839332458E-33, -1.190614954331866791E-16, 1.000000000000000000 ) ) ;
#24614 = CARTESIAN_POINT ( 'NONE',  ( -19.98190323201305318, -8.235588387909094976, 70.25100363142931315 ) ) ;
#24615 = EDGE_CURVE ( 'NONE', #34640, #8636, #39077, .T. ) ;
#24616 = CARTESIAN_POINT ( 'NONE',  ( -10.56409641782382813, -13.17052685802803680, 75.09306420679733662 ) ) ;
#24617 = CARTESIAN_POINT ( 'NONE',  ( -36.42409385541304800, -9.359200813967566646, 50.49621490985803263 ) ) ;
#24618 = CARTESIAN_POINT ( 'NONE',  ( -14.82114783504062139, -7.828710491958731588, 56.94976379657543220 ) ) ;
#24619 = CARTESIAN_POINT ( 'NONE',  ( -24.79781836340079337, -15.87314503134675014, 69.64812095075065201 ) ) ;
#24620 = VERTEX_POINT ( 'NONE', #168 ) ;
#24621 = CARTESIAN_POINT ( 'NONE',  ( -20.85666804334717739, -20.91165978247425272, 65.77381081790800010 ) ) ;
#24622 = VERTEX_POINT ( 'NONE', #41026 ) ;
#24623 = FACE_OUTER_BOUND ( 'NONE', #13557, .T. ) ;
#24624 = EDGE_CURVE ( 'NONE', #11860, #22569, #22679, .T. ) ;
#24625 = EDGE_CURVE ( 'NONE', #2258, #34107, #5439, .T. ) ;
#24626 = CARTESIAN_POINT ( 'NONE',  ( -10.01440787728688520, -14.03439562150409969, 61.03325889150411143 ) ) ;
#24627 = ORIENTED_EDGE ( 'NONE', *, *, #7851, .F. ) ;
#24628 = EDGE_CURVE ( 'NONE', #18657, #4575, #4103, .T. ) ;
#24629 = CARTESIAN_POINT ( 'NONE',  ( -13.78034385650551563, -6.424090610841176385, 49.80797279389978627 ) ) ;
#24630 = B_SPLINE_CURVE_WITH_KNOTS ( 'NONE', 3,
 ( #17118, #9771, #24785, #39787, #10717, #7035, #21797, #48146, #25734, #6784 ),
 .UNSPECIFIED., .F., .F.,
 ( 4, 2, 2, 2, 4 ),
 ( 0.000000000000000000, 0.2500000000000000000, 0.5000000000000000000, 0.7500000000000000000, 1.000000000000000000 ),
 .UNSPECIFIED. ) ;
#24631 = ORIENTED_EDGE ( 'NONE', *, *, #42888, .F. ) ;
#24632 = CARTESIAN_POINT ( 'NONE',  ( -14.96339028783852676, -21.42433367428847291, 68.72025781230657060 ) ) ;
#24633 = EDGE_CURVE ( 'NONE', #241, #2214, #9334, .T. ) ;
#24634 = CARTESIAN_POINT ( 'NONE',  ( -17.63906322355374101, -7.762336171902432191, 63.55616794089306865 ) ) ;
#24635 = PLANE ( 'NONE',  #15626 ) ;
#24636 = ORIENTED_EDGE ( 'NONE', *, *, #6379, .T. ) ;
#24637 = CARTESIAN_POINT ( 'NONE',  ( -16.27008412796014625, -7.904986034540439022, 60.20028479263386600 ) ) ;
#24638 = DIRECTION ( 'NONE',  ( -0.000000000000000000, -1.000000000000000000, -0.000000000000000000 ) ) ;
#24639 = FACE_OUTER_BOUND ( 'NONE', #11029, .T. ) ;
#24640 = DIRECTION ( 'NONE',  ( 0.9687793358424821033, -0.2479245821708679909, 0.000000000000000000 ) ) ;
#24641 = EDGE_CURVE ( 'NONE', #11090, #38015, #6921, .T. ) ;
#24642 = VERTEX_POINT ( 'NONE', #26247 ) ;
#24643 = ORIENTED_EDGE ( 'NONE', *, *, #36623, .F. ) ;
#24644 = B_SPLINE_CURVE_WITH_KNOTS ( 'NONE', 3,
 ( #27882, #35510, #46614, #2264, #12857, #28847, #39208, #13088, #43153, #39932 ),
 .UNSPECIFIED., .F., .F.,
 ( 4, 2, 2, 2, 4 ),
 ( 0.000000000000000000, 0.2500000000000000000, 0.5000000000000000000, 0.7500000000000000000, 1.000000000000000000 ),
 .UNSPECIFIED. ) ;
#24645 = PLANE ( 'NONE',  #38502 ) ;
#24646 = CARTESIAN_POINT ( 'NONE',  ( -20.89619716791787596, -20.95408004043368067, 69.19883325555726117 ) ) ;
#24647 = ORIENTED_EDGE ( 'NONE', *, *, #17446, .T. ) ;
#24648 = CARTESIAN_POINT ( 'NONE',  ( -24.34870638818816957, -15.83419385995577677, 66.28998161055176297 ) ) ;
#24649 = CARTESIAN_POINT ( 'NONE',  ( -19.28643955730387916, -21.55824949740921426, 62.22333559350940391 ) ) ;
#24650 = CARTESIAN_POINT ( 'NONE',  ( -19.57409385759799036, -6.859212275519751323, 50.50378509014259265 ) ) ;
#24651 = CARTESIAN_POINT ( 'NONE',  ( -23.78676187654788521, -10.93361199230012559, 73.54688693628270357 ) ) ;
#24652 = CARTESIAN_POINT ( 'NONE',  ( -41.92385313143115155, -14.90920654474422058, 67.00192579185520003 ) ) ;
#24653 = CYLINDRICAL_SURFACE ( 'NONE', #39663, 5.249999999999998224 ) ;
#24654 = VERTEX_POINT ( 'NONE', #14394 ) ;
#24655 = CARTESIAN_POINT ( 'NONE',  ( -16.57554779340669882, -22.21081089906203943, 65.41059674993448425 ) ) ;
#24656 = CARTESIAN_POINT ( 'NONE',  ( -13.05361004613213893, -8.775835911160044134, 64.00972289988426667 ) ) ;
#24657 = CARTESIAN_POINT ( 'NONE',  ( -22.85875596884486072, -9.713182710008496201, 73.62127706024359952 ) ) ;
#24658 = CARTESIAN_POINT ( 'NONE',  ( -17.42409385541299471, -14.80920654474435771, 49.52966884056655772 ) ) ;
#24659 = ORIENTED_EDGE ( 'NONE', *, *, #2103, .T. ) ;
#24660 = VERTEX_POINT ( 'NONE', #41261 ) ;
#24661 = ORIENTED_EDGE ( 'NONE', *, *, #38371, .F. ) ;
#24662 = CARTESIAN_POINT ( 'NONE',  ( -17.70854774853812330, -7.363889232077062807, 63.73712292196469065 ) ) ;
#24663 = FILL_AREA_STYLE ('',( #13298 ) ) ;
#24664 = CARTESIAN_POINT ( 'NONE',  ( -15.64104502085146642, -10.46221995643221092, 52.02966884056656482 ) ) ;
#24665 = EDGE_CURVE ( 'NONE', #2342, #36695, #6803, .T. ) ;
#24666 = ORIENTED_EDGE ( 'NONE', *, *, #9405, .T. ) ;
#24667 = CARTESIAN_POINT ( 'NONE',  ( -24.25719835994319951, -13.28920697710681864, 59.36267871205171076 ) ) ;
#24668 = DIRECTION ( 'NONE',  ( -3.071710424422018668E-17, 6.404604876783312462E-16, 1.000000000000000000 ) ) ;
#24669 = EDGE_CURVE ( 'NONE', #37207, #21625, #8905, .T. ) ;
#24670 = AXIS2_PLACEMENT_3D ( 'NONE', #15993, #25040, #40057 ) ;
#24671 = VERTEX_POINT ( 'NONE', #21819 ) ;
#24672 = CARTESIAN_POINT ( 'NONE',  ( -12.36794899618824317, -19.72224014812425708, 61.69678633597966666 ) ) ;
#24673 = CARTESIAN_POINT ( 'NONE',  ( -17.78489980232956569, -21.80118272162682658, 61.94706151667214300 ) ) ;
#24674 = ORIENTED_EDGE ( 'NONE', *, *, #47032, .F. ) ;
#24675 = CARTESIAN_POINT ( 'NONE',  ( -21.90433870182133802, -8.856837556793539790, 66.85424130413866806 ) ) ;
#24676 = ORIENTED_EDGE ( 'NONE', *, *, #21805, .T. ) ;
#24677 = DIRECTION ( 'NONE',  ( -3.071710424422018668E-17, 6.404604876783312462E-16, 1.000000000000000000 ) ) ;
#24678 = VERTEX_POINT ( 'NONE', #3349 ) ;
#24679 = CARTESIAN_POINT ( 'NONE',  ( -11.93063564843302160, -19.84155427294366092, 58.12693572425718003 ) ) ;
#24680 = DIRECTION ( 'NONE',  ( -4.115385489420004910E-17, -0.9999954153791273948, -0.003028072113811714535 ) ) ;
#24681 = CARTESIAN_POINT ( 'NONE',  ( -19.30128557755455176, -21.60500301973953086, 58.81035253397666196 ) ) ;
#24682 = ORIENTED_EDGE ( 'NONE', *, *, #38795, .F. ) ;
#24683 = CARTESIAN_POINT ( 'NONE',  ( -45.92409385541305511, -15.81020654474410847, 70.50000000000000000 ) ) ;
#24684 = DIRECTION ( 'NONE',  ( -3.071710424422018668E-17, 6.404604876783312462E-16, 1.000000000000000000 ) ) ;
#24685 = EDGE_CURVE ( 'NONE', #12034, #35350, #18956, .T. ) ;
#24686 = CARTESIAN_POINT ( 'NONE',  ( -12.55411140858086760, -19.90724249994213935, 65.15202838036978505 ) ) ;
#24687 = EDGE_CURVE ( 'NONE', #36936, #7665, #38910, .T. ) ;
#24688 =( BOUNDED_SURFACE ( )  B_SPLINE_SURFACE ( 3, 1, ( 
 ( #7141, #22158 ),
 ( #18434, #13998 ),
 ( #10352, #25365 ),
 ( #29787, #6647 ),
 ( #14246, #33443 ),
 ( #29295, #44332 ),
 ( #40603, #6888 ) ),
 .UNSPECIFIED., .T., .F., .F. ) 
 B_SPLINE_SURFACE_WITH_KNOTS ( ( 4, 3, 4 ),
 ( 2, 2 ),
 ( 0.000000000000000000, 0.5000000000000000000, 1.000000000000000000 ),
 ( 0.000000000000000000, 1.000000000000000000 ),
 .UNSPECIFIED. ) 
 GEOMETRIC_REPRESENTATION_ITEM ( )  RATIONAL_B_SPLINE_SURFACE ( (
 ( 1.000000000000000000, 1.000000000000000000),
 ( 0.3333333333333335369, 0.3333333333333330373),
 ( 0.3333333333333335369, 0.3333333333333330373),
 ( 1.000000000000000000, 1.000000000000000000),
 ( 0.3333333333333333703, 0.3333333333333333703),
 ( 0.3333333333333333703, 0.3333333333333333703),
 ( 1.000000000000000000, 1.000000000000000000) ) ) 
 REPRESENTATION_ITEM ( '' )  SURFACE ( )  );
#24689 = CARTESIAN_POINT ( 'NONE',  ( -11.41497376296057098, -19.21309731666858411, 71.80190493362104576 ) ) ;
#24690 = DIRECTION ( 'NONE',  ( 3.413470714839332458E-33, -1.190614954331866791E-16, 1.000000000000000000 ) ) ;
#24691 = EDGE_LOOP ( 'NONE', ( #1182, #18310, #16919, #7231, #5172 ) ) ;
#24692 = CARTESIAN_POINT ( 'NONE',  ( -14.84764829735760827, -8.246537290690364230, 60.33468334944129197 ) ) ;
#24693 = CARTESIAN_POINT ( 'NONE',  ( -11.82258790637234291, -19.00740242323033513, 71.98685835211126971 ) ) ;
#24694 = CARTESIAN_POINT ( 'NONE',  ( -12.23220206747517835, -19.57856285391799034, 58.22682373937799127 ) ) ;
#24695 = CARTESIAN_POINT ( 'NONE',  ( -13.19632391105088409, -20.94361350779438879, 58.18503525494669049 ) ) ;
#24696 = ADVANCED_FACE ( 'NONE', ( #35078 ), #4567, .T. ) ;
#24697 = CARTESIAN_POINT ( 'NONE',  ( -17.83034385759799179, -6.857644439848014528, 49.98602051094139398 ) ) ;
#24698 = CARTESIAN_POINT ( 'NONE',  ( -24.29232294273250758, -16.16103065725259214, 62.59328677063434299 ) ) ;
#24699 = ORIENTED_EDGE ( 'NONE', *, *, #41674, .F. ) ;
#24700 = LINE ( 'NONE', #35751, #40856 ) ;
#24701 = CARTESIAN_POINT ( 'NONE',  ( -24.81704557732260952, -15.73545128243976521, 73.18959105933400622 ) ) ;
#24702 = EDGE_LOOP ( 'NONE', ( #39656, #14406, #12427, #25897, #22012 ) ) ;
#24703 = LINE ( 'NONE', #13101, #28453 ) ;
#24704 = CARTESIAN_POINT ( 'NONE',  ( -19.96994574550859980, -21.32983827578761193, 72.40478737306770540 ) ) ;
#24705 = FACE_OUTER_BOUND ( 'NONE', #27488, .T. ) ;
#24706 = CARTESIAN_POINT ( 'NONE',  ( -23.08487763607990928, -19.01185175973044039, 62.36879011380454330 ) ) ;
#24707 = CARTESIAN_POINT ( 'NONE',  ( -16.99752982347189345, -22.24711114454501626, 72.34260117165817405 ) ) ;
#24708 = EDGE_CURVE ( 'NONE', #2695, #47031, #3059, .T. ) ;
#24709 =( BOUNDED_SURFACE ( )  B_SPLINE_SURFACE ( 3, 1, ( 
 ( #14915, #11256 ),
 ( #29973, #22836 ),
 ( #45483, #189 ),
 ( #34131, #3875 ),
 ( #11742, #26270 ),
 ( #37572, #30225 ),
 ( #43912, #12483 ) ),
 .UNSPECIFIED., .T., .F., .F. ) 
 B_SPLINE_SURFACE_WITH_KNOTS ( ( 4, 3, 4 ),
 ( 2, 2 ),
 ( 0.000000000000000000, 0.5000000000000000000, 1.000000000000000000 ),
 ( 0.000000000000000000, 1.000000000000000000 ),
 .UNSPECIFIED. ) 
 GEOMETRIC_REPRESENTATION_ITEM ( )  RATIONAL_B_SPLINE_SURFACE ( (
 ( 1.000000000000000000, 1.000000000000000000),
 ( 0.3333333333333335369, 0.3333333333333330373),
 ( 0.3333333333333335369, 0.3333333333333330373),
 ( 1.000000000000000000, 1.000000000000000000),
 ( 0.3333333333333333703, 0.3333333333333333703),
 ( 0.3333333333333333703, 0.3333333333333333703),
 ( 1.000000000000000000, 1.000000000000000000) ) ) 
 REPRESENTATION_ITEM ( '' )  SURFACE ( )  );
#24710 = ORIENTED_EDGE ( 'NONE', *, *, #4418, .T. ) ;
#24711 = CARTESIAN_POINT ( 'NONE',  ( -24.41053240502948896, -14.37272825023783618, 66.19795200961559090 ) ) ;
#24712 = CARTESIAN_POINT ( 'NONE',  ( -17.08574859075978480, -7.366143556642608559, 74.14673579026420214 ) ) ;
#24713 = CIRCLE ( 'NONE', #48373, 2.000000000000000444 ) ;
#24714 = CARTESIAN_POINT ( 'NONE',  ( -23.75797280549784318, -17.78947120508452429, 59.30378417803890301 ) ) ;
#24715 = ORIENTED_EDGE ( 'NONE', *, *, #18102, .F. ) ;
#24716 = AXIS2_PLACEMENT_3D ( 'NONE', #46369, #12626, #1539 ) ;
#24717 = DIRECTION ( 'NONE',  ( 1.000000000000000000, -0.000000000000000000, -2.406186529621654511E-16 ) ) ;
#24718 = DIRECTION ( 'NONE',  ( 0.9729319276368276759, 0.2310918955413240050, -6.827553174550346358E-08 ) ) ;
#24719 = CARTESIAN_POINT ( 'NONE',  ( -23.46018740455247809, -11.26354644359006585, 73.64576786816009246 ) ) ;
#24720 = CARTESIAN_POINT ( 'NONE',  ( -24.17041903051225304, -17.96986306003213940, 59.10354794152625857 ) ) ;
#24721 = CARTESIAN_POINT ( 'NONE',  ( -17.42409385541300892, -14.80920654474439679, 56.49999999999994316 ) ) ;
#24722 = DIRECTION ( 'NONE',  ( -0.1240347345892086062, 1.145860353393066553E-16, -0.9922778767136676281 ) ) ;
#24723 =( BOUNDED_SURFACE ( )  B_SPLINE_SURFACE ( 3, 1, ( 
 ( #14529, #36390 ),
 ( #24848, #2900 ),
 ( #39857, #20908 ),
 ( #32932, #36622 ),
 ( #20673, #2670 ),
 ( #5889, #13018 ),
 ( #2188, #28044 ) ),
 .UNSPECIFIED., .T., .F., .F. ) 
 B_SPLINE_SURFACE_WITH_KNOTS ( ( 4, 3, 4 ),
 ( 2, 2 ),
 ( 0.000000000000000000, 0.5000000000000000000, 1.000000000000000000 ),
 ( 0.000000000000000000, 1.000000000000000000 ),
 .UNSPECIFIED. ) 
 GEOMETRIC_REPRESENTATION_ITEM ( )  RATIONAL_B_SPLINE_SURFACE ( (
 ( 1.000000000000000000, 1.000000000000000000),
 ( 0.3333333333333335369, 0.3333333333333330373),
 ( 0.3333333333333335369, 0.3333333333333330373),
 ( 1.000000000000000000, 1.000000000000000000),
 ( 0.3333333333333333703, 0.3333333333333333703),
 ( 0.3333333333333333703, 0.3333333333333333703),
 ( 1.000000000000000000, 1.000000000000000000) ) ) 
 REPRESENTATION_ITEM ( '' )  SURFACE ( )  );
#24724 = VERTEX_POINT ( 'NONE', #30688 ) ;
#24725 = ORIENTED_EDGE ( 'NONE', *, *, #24624, .T. ) ;
#24726 = CARTESIAN_POINT ( 'NONE',  ( -18.24909385541304374, -8.112991634885936776, 51.74999426922421719 ) ) ;
#24727 = FACE_OUTER_BOUND ( 'NONE', #29185, .T. ) ;
#24728 = B_SPLINE_CURVE_WITH_KNOTS ( 'NONE', 3,
 ( #22853, #34145, #27014, #42530, #34635, #23573, #19876, #42037, #45975, #1143 ),
 .UNSPECIFIED., .F., .F.,
 ( 4, 2, 2, 2, 4 ),
 ( 0.000000000000000000, 0.2500000000000000000, 0.5000000000000000000, 0.7500000000000000000, 1.000000000000000000 ),
 .UNSPECIFIED. ) ;
#24729 = CARTESIAN_POINT ( 'NONE',  ( -15.81671074304997582, -7.936704070960259649, 74.22418700304095296 ) ) ;
#24730 = ADVANCED_FACE ( 'NONE', ( #45941 ), #15381, .T. ) ;
#24731 = DIRECTION ( 'NONE',  ( 0.9687793358424821033, -0.2479245821708677133, 0.000000000000000000 ) ) ;
#24732 = DIRECTION ( 'NONE',  ( 0.9942595023566569434, -0.1069955231469581769, 3.800058679842193584E-08 ) ) ;
#24733 = ORIENTED_EDGE ( 'NONE', *, *, #35597, .F. ) ;
#24734 = CARTESIAN_POINT ( 'NONE',  ( -14.42409385541304090, -9.359200813967568422, 50.49621490985801842 ) ) ;
#24735 = DIRECTION ( 'NONE',  ( -6.867234345585435779E-33, 2.395284034871316381E-16, -1.000000000000000000 ) ) ;
#24736 = VERTEX_POINT ( 'NONE', #35329 ) ;
#24737 = DIRECTION ( 'NONE',  ( -0.8651630202045380580, 0.5014907262059380422, 5.433021001366389699E-08 ) ) ;
#24738 = CARTESIAN_POINT ( 'NONE',  ( -17.42409385541299471, -14.80920654474435594, 52.02966884056656482 ) ) ;
#24739 = AXIS2_PLACEMENT_3D ( 'NONE', #46079, #4968, #35223 ) ;
#24740 = ORIENTED_EDGE ( 'NONE', *, *, #48514, .T. ) ;
#24741 = DIRECTION ( 'NONE',  ( 0.4433615477241706904, -0.8963428685495450354, 2.661652803430218851E-08 ) ) ;
#24742 = CARTESIAN_POINT ( 'NONE',  ( -14.72778380697628187, -21.32322314059345558, 58.16617885012796307 ) ) ;
#24743 = VERTEX_POINT ( 'NONE', #42494 ) ;
#24744 = DIRECTION ( 'NONE',  ( -3.071710424422018668E-17, 6.404604876783312462E-16, 1.000000000000000000 ) ) ;
#24745 = AXIS2_PLACEMENT_3D ( 'NONE', #28981, #6583, #39822 ) ;
#24746 = ADVANCED_FACE ( 'NONE', ( #16365 ), #34348, .F. ) ;
#24747 = CARTESIAN_POINT ( 'NONE',  ( -24.14854887165027009, -16.95319183457820955, 69.56907079017828721 ) ) ;
#24748 = CARTESIAN_POINT ( 'NONE',  ( -16.63457431780823725, -21.76466301827511174, 65.22564349372431991 ) ) ;
#24749 = CARTESIAN_POINT ( 'NONE',  ( 10.57590614458695377, 0.6407533398237040823, 50.52649563099625851 ) ) ;
#24750 = EDGE_LOOP ( 'NONE', ( #27688, #42480, #30344, #6991 ) ) ;
#24751 = DIRECTION ( 'NONE',  ( -0.04108628546905851442, -0.9991556020692448081, 4.908153721456304258E-18 ) ) ;
#24752 = CARTESIAN_POINT ( 'NONE',  ( -17.42409385541299471, -14.80920654474435771, 49.52966884056655772 ) ) ;
#24753 = FACE_OUTER_BOUND ( 'NONE', #20117, .T. ) ;
#24754 = EDGE_CURVE ( 'NONE', #30663, #32429, #11885, .T. ) ;
#24755 = CARTESIAN_POINT ( 'NONE',  ( -13.42364920204782841, -9.064338107659910548, 49.69363550579117117 ) ) ;
#24756 = CARTESIAN_POINT ( 'NONE',  ( -22.33041777183100507, -20.41561037748852669, 62.34943743628787161 ) ) ;
#24757 = CARTESIAN_POINT ( 'NONE',  ( -16.32575768948312600, -7.844986739114469643, 60.21500614002425777 ) ) ;
#24758 = CYLINDRICAL_SURFACE ( 'NONE', #45637, 5.249999999999998224 ) ;
#24759 = ORIENTED_EDGE ( 'NONE', *, *, #16746, .F. ) ;
#24760 = DIRECTION ( 'NONE',  ( 2.866981220435666553E-17, -1.000000000000000000, -1.190614954331866791E-16 ) ) ;
#24761 = ADVANCED_FACE ( 'NONE', ( #8507 ), #30929, .T. ) ;
#24762 = CARTESIAN_POINT ( 'NONE',  ( -12.77796340496265870, -17.75258416873320400, 53.49999999999995026 ) ) ;
#24763 = CARTESIAN_POINT ( 'NONE',  ( -10.00054666056749575, -15.43791465228438931, 57.74605562754308608 ) ) ;
#24764 = ORIENTED_EDGE ( 'NONE', *, *, #25130, .T. ) ;
#24765 = CARTESIAN_POINT ( 'NONE',  ( -21.08382089131013259, -22.19632712819893428, 53.49999999999995026 ) ) ;
#24766 = ORIENTED_EDGE ( 'NONE', *, *, #31245, .T. ) ;
#24767 = ORIENTED_EDGE ( 'NONE', *, *, #35850, .T. ) ;
#24768 = ORIENTED_EDGE ( 'NONE', *, *, #25544, .T. ) ;
#24769 = CARTESIAN_POINT ( 'NONE',  ( -13.94586845990913737, -20.88575566452655607, 72.03680843657026855 ) ) ;
#24770 = CARTESIAN_POINT ( 'NONE',  ( -12.89674140296688520, -8.892592839661450199, 67.57281105838596602 ) ) ;
#24771 = LINE ( 'NONE', #21784, #41667 ) ;
#24772 = ADVANCED_FACE ( 'NONE', ( #42247 ), #27459, .T. ) ;
#24773 = CARTESIAN_POINT ( 'NONE',  ( -24.71495620756359557, -13.27698325404237956, 59.48551063991843790 ) ) ;
#24774 = DIRECTION ( 'NONE',  ( 0.9687793358424819923, -0.2479245821708678243, 0.000000000000000000 ) ) ;
#24775 = EDGE_CURVE ( 'NONE', #40286, #32734, #46273, .T. ) ;
#24776 = ORIENTED_EDGE ( 'NONE', *, *, #27122, .T. ) ;
#24777 = ORIENTED_EDGE ( 'NONE', *, *, #20267, .F. ) ;
#24778 = VECTOR ( 'NONE', #15697, 1000.000000000000000 ) ;
#24779 = CARTESIAN_POINT ( 'NONE',  ( -17.88659385650551670, -9.302874398569244363, 51.68646062012417985 ) ) ;
#24780 = EDGE_CURVE ( 'NONE', #41647, #13929, #46429, .T. ) ;
#24781 = LINE ( 'NONE', #1874, #35432 ) ;
#24782 = CARTESIAN_POINT ( 'NONE',  ( -50.42609385541305755, -14.80920654474424225, 70.97647058823527288 ) ) ;
#24783 = CARTESIAN_POINT ( 'NONE',  ( -19.51784385650551457, -9.790100578890868377, 49.79778022625163203 ) ) ;
#24784 = ORIENTED_EDGE ( 'NONE', *, *, #30180, .T. ) ;
#24785 = CARTESIAN_POINT ( 'NONE',  ( -24.36735374303742319, -15.69913859885677176, 69.54809873558210143 ) ) ;
#24786 = CARTESIAN_POINT ( 'NONE',  ( -24.87394656424350359, -14.85804368301403500, 59.34325982243593245 ) ) ;
#24787 =( BOUNDED_SURFACE ( )  B_SPLINE_SURFACE ( 3, 1, ( 
 ( #23599, #24080 ),
 ( #42561, #1412 ),
 ( #704, #34666 ),
 ( #42063, #942 ),
 ( #46730, #15941 ),
 ( #12500, #8336 ),
 ( #31216, #35141 ) ),
 .UNSPECIFIED., .T., .F., .F. ) 
 B_SPLINE_SURFACE_WITH_KNOTS ( ( 4, 3, 4 ),
 ( 2, 2 ),
 ( 0.000000000000000000, 0.5000000000000000000, 1.000000000000000000 ),
 ( 0.000000000000000000, 1.000000000000000000 ),
 .UNSPECIFIED. ) 
 GEOMETRIC_REPRESENTATION_ITEM ( )  RATIONAL_B_SPLINE_SURFACE ( (
 ( 1.000000000000000000, 1.000000000000000000),
 ( 0.3333333333333335369, 0.3333333333333330373),
 ( 0.3333333333333335369, 0.3333333333333330373),
 ( 1.000000000000000000, 1.000000000000000000),
 ( 0.3333333333333333703, 0.3333333333333333703),
 ( 0.3333333333333333703, 0.3333333333333333703),
 ( 1.000000000000000000, 1.000000000000000000) ) ) 
 REPRESENTATION_ITEM ( '' )  SURFACE ( )  );
#24788 = ORIENTED_EDGE ( 'NONE', *, *, #27618, .T. ) ;
#24789 = B_SPLINE_CURVE_WITH_KNOTS ( 'NONE', 3,
 ( #26263, #12639, #45897, #41278, #23491, #16310, #45004, #48666, #37320, #14649 ),
 .UNSPECIFIED., .F., .F.,
 ( 4, 2, 2, 2, 4 ),
 ( 0.6272669072877501417, 0.7522669073072613122, 0.8772669073267724826, 1.002266907346283542, 1.127266907365794824 ),
 .UNSPECIFIED. ) ;
#24790 = CARTESIAN_POINT ( 'NONE',  ( -22.09234551867295338, -20.09219114410425178, 62.53439162497838311 ) ) ;
#24791 = B_SPLINE_CURVE_WITH_KNOTS ( 'NONE', 3,
 ( #46615, #5241, #27883, #1537, #9905, #42911, #36228, #16546, #31586, #6206 ),
 .UNSPECIFIED., .F., .F.,
 ( 4, 2, 2, 2, 4 ),
 ( 0.000000000000000000, 0.2500000000000000000, 0.5000000000000000000, 0.7500000000000000000, 1.000000000000000000 ),
 .UNSPECIFIED. ) ;
#24792 = CARTESIAN_POINT ( 'NONE',  ( -17.42409385541299471, -14.80920654474434883, 62.02966884056656482 ) ) ;
#24793 = ORIENTED_EDGE ( 'NONE', *, *, #23533, .T. ) ;
#24794 = DIRECTION ( 'NONE',  ( 1.504942871710700414E-06, -3.061075848816703091E-06, 0.9999999999941824314 ) ) ;
#24795 = CARTESIAN_POINT ( 'NONE',  ( -11.37092239977862640, -11.18788622403751276, 64.44882256896082140 ) ) ;
#24796 = DIRECTION ( 'NONE',  ( 0.9687793358424817702, -0.2479245821708688791, 0.000000000000000000 ) ) ;
#24797 = ORIENTED_EDGE ( 'NONE', *, *, #2101, .T. ) ;
#24798 = CARTESIAN_POINT ( 'NONE',  ( -24.09792882696954663, -17.08130396874204138, 73.03336032035906555 ) ) ;
#24799 = VERTEX_POINT ( 'NONE', #8049 ) ;
#24800 = CARTESIAN_POINT ( 'NONE',  ( -14.99706723701585354, -21.85287888328288375, 65.29092001793476641 ) ) ;
#24802 = EDGE_CURVE ( 'NONE', #25977, #34579, #1936, .T. ) ;
#24801 = ORIENTED_EDGE ( 'NONE', *, *, #36383, .F. ) ;
#24803 = FACE_OUTER_BOUND ( 'NONE', #9507, .T. ) ;
#24804 = CARTESIAN_POINT ( 'NONE',  ( -21.85024312005885250, -20.23279700434262907, 59.04826358179722945 ) ) ;
#24805 = VECTOR ( 'NONE', #2926, 1000.000000000000114 ) ;
#24806 = CARTESIAN_POINT ( 'NONE',  ( -13.18362886651731358, -8.683667069837246899, 60.62445550483372614 ) ) ;
#24807 = CARTESIAN_POINT ( 'NONE',  ( -14.30855566557790404, -8.484641631233271752, 70.74429704309763167 ) ) ;
#24808 = VERTEX_POINT ( 'NONE', #15884 ) ;
#24809 = DIRECTION ( 'NONE',  ( -0.9998756790481364565, -0.01576789294826319576, -3.907472230461691850E-09 ) ) ;
#24810 = CARTESIAN_POINT ( 'NONE',  ( -23.97043363090852353, -12.17094895590152426, 59.62668449103946955 ) ) ;
#24811 = DIRECTION ( 'NONE',  ( -4.267285103686820140E-17, 1.935130192142698731E-16, 1.000000000000000000 ) ) ;
#24812 = ORIENTED_EDGE ( 'NONE', *, *, #6068, .F. ) ;
#24813 = CARTESIAN_POINT ( 'NONE',  ( -10.17894133981683247, -13.07414026325376177, 71.30854345628114288 ) ) ;
#24814 = CARTESIAN_POINT ( 'NONE',  ( -24.31944129331298399, -13.32629719641017729, 63.24753052856355140 ) ) ;
#24815 = VERTEX_POINT ( 'NONE', #1602 ) ;
#24816 = ORIENTED_EDGE ( 'NONE', *, *, #48610, .T. ) ;
#24817 = CARTESIAN_POINT ( 'NONE',  ( -23.71751471349159601, -11.63122711669449316, 63.23746208799618529 ) ) ;
#24818 = CARTESIAN_POINT ( 'NONE',  ( -17.42409385541299471, -14.80920654474435771, 49.52966884056655772 ) ) ;
#24819 = CARTESIAN_POINT ( 'NONE',  ( -13.18473975798692877, -20.93551490194142062, 58.23145353898504339 ) ) ;
#24820 = CARTESIAN_POINT ( 'NONE',  ( -16.84284385650551741, -8.811426318492348031, 52.18089403414752070 ) ) ;
#24821 = CARTESIAN_POINT ( 'NONE',  ( -21.88700264784966976, -8.843686206210612966, 66.80003455143545921 ) ) ;
#24822 = CARTESIAN_POINT ( 'NONE',  ( -10.40860991809309155, -15.50898095412354571, 57.85320721669017985 ) ) ;
#24823 = CARTESIAN_POINT ( 'NONE',  ( -10.78978129946085929, -12.42417050351721919, 57.47857332104950956 ) ) ;
#24824 = CARTESIAN_POINT ( 'NONE',  ( -12.20924706590383302, -20.12979026787678549, 65.06013176247181207 ) ) ;
#24825 = B_SPLINE_CURVE_WITH_KNOTS ( 'NONE', 3,
 ( #32761, #17499, #14026, #24673, #24906, #39676, #29076, #5948, #20967, #17256 ),
 .UNSPECIFIED., .F., .F.,
 ( 4, 2, 2, 2, 4 ),
 ( 0.000000000000000000, 0.2500000000000000000, 0.5000000000000000000, 0.7500000000000000000, 1.000000000000000000 ),
 .UNSPECIFIED. ) ;
#24826 = EDGE_CURVE ( 'NONE', #8859, #30479, #16370, .T. ) ;
#24827 = CARTESIAN_POINT ( 'NONE',  ( -16.73751461255839601, -22.22750928065944009, 68.89571854458313283 ) ) ;
#24828 = ORIENTED_EDGE ( 'NONE', *, *, #35181, .T. ) ;
#24829 = VERTEX_POINT ( 'NONE', #2082 ) ;
#24830 = CARTESIAN_POINT ( 'NONE',  ( -36.42409385541304800, -8.109206544743658540, 50.50000000000030553 ) ) ;
#24831 = ADVANCED_FACE ( 'NONE', ( #39516 ), #47152, .T. ) ;
#24832 = EDGE_CURVE ( 'NONE', #3957, #3366, #24265, .T. ) ;
#24833 = CARTESIAN_POINT ( 'NONE',  ( -21.96907604098356970, -20.13311438280304344, 59.04977527294225581 ) ) ;
#24834 = CARTESIAN_POINT ( 'NONE',  ( -15.88656107989463706, -7.980151544674868980, 67.14007279409138107 ) ) ;
#24835 = CARTESIAN_POINT ( 'NONE',  ( -12.01648241349452917, -10.28590705807702932, 67.49896869922172016 ) ) ;
#24836 = LINE ( 'NONE', #39846, #39403 ) ;
#24837 =( BOUNDED_CURVE ( )  B_SPLINE_CURVE ( 2, ( #15066, #26910, #22982, #26414, #38455, #4741, #801, #3764, #4487 ),
 .UNSPECIFIED., .F., .F. ) 
 B_SPLINE_CURVE_WITH_KNOTS ( ( 3, 2, 2, 2, 3 ),
 ( 0.8333333333333334814, 0.8437500000000001110, 0.8541666666666667407, 0.8645833333333333703, 0.8750000000000000000 ),
 .UNSPECIFIED. ) 
 CURVE ( )  GEOMETRIC_REPRESENTATION_ITEM ( )  RATIONAL_B_SPLINE_CURVE ( ( 0.9999999999999992228, 0.9238795325112875156, 1.000000000000000000, 0.9238795325112867385, 1.000000000000000000, 0.9238795325112867385, 1.000000000000000000, 0.9238795325112867385, 1.000000000000000000 ) ) 
 REPRESENTATION_ITEM ( '' )  );
#24838 = CARTESIAN_POINT ( 'NONE',  ( -20.21784385650551386, -9.790100578890868377, 49.79778022625163203 ) ) ;
#24839 = CIRCLE ( 'NONE', #33447, 1.250000000000001110 ) ;
#24840 = VERTEX_POINT ( 'NONE', #13393 ) ;
#24841 = CARTESIAN_POINT ( 'NONE',  ( -15.05456328141641542, -21.39602539821822091, 61.86273865514400683 ) ) ;
#24842 = CARTESIAN_POINT ( 'NONE',  ( -10.21583571369164467, -12.92629908267978323, 67.86019570968910841 ) ) ;
#24843 = CARTESIAN_POINT ( 'NONE',  ( -17.65810221059773610, -7.762793303104816189, 63.56529088875731759 ) ) ;
#24844 = CARTESIAN_POINT ( 'NONE',  ( -18.20795910203089818, -22.21802180157784079, 65.48385643348356666 ) ) ;
#24845 = ORIENTED_EDGE ( 'NONE', *, *, #31850, .T. ) ;
#24846 =( BOUNDED_CURVE ( )  B_SPLINE_CURVE ( 3, ( #15042, #7450, #30591, #41903 ),
 .UNSPECIFIED., .F., .F. ) 
 B_SPLINE_CURVE_WITH_KNOTS ( ( 4, 4 ),
 ( 0.4074455897393572390, 0.5000000000000000000 ),
 .UNSPECIFIED. ) 
 CURVE ( )  GEOMETRIC_REPRESENTATION_ITEM ( )  RATIONAL_B_SPLINE_CURVE ( ( 0.6983129098260801859, 0.7760317562606920960, 0.8765941196520000700, 1.000000000000007772 ) ) 
 REPRESENTATION_ITEM ( '' )  );
#24847 = DIRECTION ( 'NONE',  ( 0.000000000000000000, 0.9999954153791273948, 0.003028072113820366902 ) ) ;
#24848 = CARTESIAN_POINT ( 'NONE',  ( -17.45593231491017505, -7.751306502474292870, 60.23627933525208533 ) ) ;
#24849 = ADVANCED_FACE ( 'NONE', ( #6517 ), #417, .T. ) ;
#24850 = CARTESIAN_POINT ( 'NONE',  ( -15.62778143507988560, -7.578882312233643503, 70.78802623904546465 ) ) ;
#24851 = CARTESIAN_POINT ( 'NONE',  ( -11.11547657867172134, -10.84637923393623993, 57.30879572875446826 ) ) ;
#24852 = CARTESIAN_POINT ( 'NONE',  ( -10.33531725737393181, -17.10115422170377641, 57.87255955594724810 ) ) ;
#24853 = VERTEX_POINT ( 'NONE', #21298 ) ;
#24854 = CARTESIAN_POINT ( 'NONE',  ( -19.30272045617997634, -8.014115550771091279, 59.96092997145632353 ) ) ;
#24855 = VERTEX_POINT ( 'NONE', #35805 ) ;
#24856 = CARTESIAN_POINT ( 'NONE',  ( -21.57995947450667984, -9.113990939708573435, 70.14604673427196246 ) ) ;
#24857 = CARTESIAN_POINT ( 'NONE',  ( -14.90534385759799463, -7.595227055684746986, 51.75156210489594599 ) ) ;
#24858 = ORIENTED_EDGE ( 'NONE', *, *, #47661, .F. ) ;
#24859 = CARTESIAN_POINT ( 'NONE',  ( -20.37299750454370439, -8.405577324698720432, 66.78104082189589974 ) ) ;
#24860 = CARTESIAN_POINT ( 'NONE',  ( -13.17364477763805652, -9.395196358873663556, 49.41429196092195042 ) ) ;
#24861 = ADVANCED_FACE ( 'NONE', ( #21045 ), #36292, .T. ) ;
#24862 = VERTEX_POINT ( 'NONE', #32133 ) ;
#24863 = CARTESIAN_POINT ( 'NONE',  ( -18.79452142415569682, -7.944218599080984156, 70.38684728956484093 ) ) ;
#24864 = CARTESIAN_POINT ( 'NONE',  ( -10.65167304149821881, -11.70447990960673046, 74.69806764605195326 ) ) ;
#24865 = DIRECTION ( 'NONE',  ( 1.616182858256118536E-16, 0.003028072113822188795, -0.9999954153791273948 ) ) ;
#24866 = EDGE_LOOP ( 'NONE', ( #16374, #10049 ) ) ;
#24867 = DIRECTION ( 'NONE',  ( -0.9848822020395751053, 0.1732254256905498280, 7.367703375004543066E-08 ) ) ;
#24868 = DIRECTION ( 'NONE',  ( 1.000000000000000000, -4.164305804376849172E-17, 1.614929280266638808E-16 ) ) ;
#24869 = CIRCLE ( 'NONE', #31155, 2.000000000000000000 ) ;
#24870 = CARTESIAN_POINT ( 'NONE',  ( -24.09883172553966091, -12.52826034843049996, 69.77242826584058832 ) ) ;
#24871 = FACE_OUTER_BOUND ( 'NONE', #7999, .T. ) ;
#24872 = ORIENTED_EDGE ( 'NONE', *, *, #18291, .T. ) ;
#24873 = EDGE_LOOP ( 'NONE', ( #28814, #40284, #20222, #15062, #10505 ) ) ;
#24874 = CARTESIAN_POINT ( 'NONE',  ( -21.36420383812641077, -21.13211724076752773, 69.31096130815059553 ) ) ;
#24875 = EDGE_LOOP ( 'NONE', ( #23076, #34955, #3162, #43478, #23457 ) ) ;
#24876 = CARTESIAN_POINT ( 'NONE',  ( -15.00927913818083859, -10.79274639537912783, 49.52966884056655772 ) ) ;
#24877 = CARTESIAN_POINT ( 'NONE',  ( -20.30534385759798965, -7.595227055684746986, 51.75156210489594599 ) ) ;
#24878 = LINE ( 'NONE', #39892, #6923 ) ;
#24879 = B_SPLINE_CURVE_WITH_KNOTS ( 'NONE', 1,
 ( #44087, #29522 ),
 .UNSPECIFIED., .F., .F.,
 ( 2, 2 ),
 ( 0.000000000000000000, 1.000000000000000000 ),
 .UNSPECIFIED. ) ;
#24880 = CARTESIAN_POINT ( 'NONE',  ( -17.42409385541299471, -14.80920654474435594, 52.02966884056656482 ) ) ;
#24881 = CARTESIAN_POINT ( 'NONE',  ( -20.57278697373333998, -8.057206101692887756, 66.89608655064280640 ) ) ;
#24882 = ORIENTED_EDGE ( 'NONE', *, *, #23184, .F. ) ;
#24883 = CARTESIAN_POINT ( 'NONE',  ( -20.66848101912799862, -8.549761622307151754, 60.12653141481577990 ) ) ;
#24884 = EDGE_CURVE ( 'NONE', #8174, #14528, #38281, .T. ) ;
#24885 = ADVANCED_FACE ( 'NONE', ( #20575 ), #9493, .T. ) ;
#24886 = DIRECTION ( 'NONE',  ( 0.9687793358424804380, -0.2479245821708739583, 0.000000000000000000 ) ) ;
#24887 = CARTESIAN_POINT ( 'NONE',  ( -17.42409385541299471, -14.80920654474434883, 62.02966884056656482 ) ) ;
#24888 = CARTESIAN_POINT ( 'NONE',  ( -13.57572078670752447, -20.65643022133334128, 61.81646323932617548 ) ) ;
#24889 = ORIENTED_EDGE ( 'NONE', *, *, #21891, .T. ) ;
#24890 = EDGE_CURVE ( 'NONE', #19021, #13315, #15476, .T. ) ;
#24891 = EDGE_CURVE ( 'NONE', #6295, #28161, #31650, .T. ) ;
#24892 = EDGE_LOOP ( 'NONE', ( #48145, #14698, #12662, #5227, #47362 ) ) ;
#24893 = FACE_OUTER_BOUND ( 'NONE', #30708, .T. ) ;
#24894 = CARTESIAN_POINT ( 'NONE',  ( -17.42409385541305511, -14.80920654474410725, 79.00000000000000000 ) ) ;
#24895 = EDGE_CURVE ( 'NONE', #13929, #1563, #41557, .T. ) ;
#24896 = CARTESIAN_POINT ( 'NONE',  ( -23.92719435707370224, -11.17417392741853988, 70.00715344888816105 ) ) ;
#24897 = EDGE_CURVE ( 'NONE', #30760, #45046, #25228, .T. ) ;
#24898 = ORIENTED_EDGE ( 'NONE', *, *, #12885, .F. ) ;
#24899 = DIRECTION ( 'NONE',  ( 0.8603395911234834603, 0.5097212845717522534, 0.000000000000000000 ) ) ;
#24900 = AXIS2_PLACEMENT_3D ( 'NONE', #21209, #21921, #40162 ) ;
#24901 = VECTOR ( 'NONE', #8136, 1000.000000000000114 ) ;
#24902 = DIRECTION ( 'NONE',  ( -0.9974380310868018462, -0.07153582418399356824, 3.008056591778322057E-08 ) ) ;
#24903 = EDGE_CURVE ( 'NONE', #24008, #6937, #47843, .T. ) ;
#24904 = EDGE_LOOP ( 'NONE', ( #41630, #46929, #25256, #33667, #20812 ) ) ;
#24905 = FACE_OUTER_BOUND ( 'NONE', #46889, .T. ) ;
#24906 = CARTESIAN_POINT ( 'NONE',  ( -17.76877427553128896, -21.80232428101829711, 61.98608964106817609 ) ) ;
#24907 = CARTESIAN_POINT ( 'NONE',  ( -23.38560432932743538, -19.27844084936127800, 58.99755287451023378 ) ) ;
#24908 = ORIENTED_EDGE ( 'NONE', *, *, #10177, .F. ) ;
#24909 = DIRECTION ( 'NONE',  ( -0.3824554607245533866, 0.9239739285077093189, -8.917814418161381897E-09 ) ) ;
#24910 = ORIENTED_EDGE ( 'NONE', *, *, #25442, .T. ) ;
#24911 = CYLINDRICAL_SURFACE ( 'NONE', #33070, 5.249999999999998224 ) ;
#24912 = DIRECTION ( 'NONE',  ( 1.616182858256114592E-16, 0.003028072113811714535, -0.9999954153791273948 ) ) ;
#24913 = DIRECTION ( 'NONE',  ( 1.000000000000000000, -4.164305804376849172E-17, 1.614929280266638808E-16 ) ) ;
#24914 = ORIENTED_EDGE ( 'NONE', *, *, #17601, .F. ) ;
#24915 = CARTESIAN_POINT ( 'NONE',  ( -19.36683724782897897, -21.58655468785150688, 62.00975759738177118 ) ) ;
#24916 = CARTESIAN_POINT ( 'NONE',  ( -50.42409385541304800, -25.10920654474410441, 74.99999999999998579 ) ) ;
#24917 = DIRECTION ( 'NONE',  ( 1.000000000000000000, 2.866981220435670867E-17, -3.652049423109068320E-16 ) ) ;
#24918 = DIRECTION ( 'NONE',  ( 0.6827297667453423591, 0.7306709694519485376, 5.176517822219622992E-09 ) ) ;
#24919 = CARTESIAN_POINT ( 'NONE',  ( -21.70267066777908838, -12.86772875551263873, 52.02966884056656482 ) ) ;
#24920 = ORIENTED_EDGE ( 'NONE', *, *, #22163, .F. ) ;
#24921 = CARTESIAN_POINT ( 'NONE',  ( -22.49805064719525305, -9.986866608920609067, 73.48161091687566682 ) ) ;
#24922 = CARTESIAN_POINT ( 'NONE',  ( -17.42409385541300892, -14.80920654474439324, 75.49999999999994316 ) ) ;
#24923 = FACE_OUTER_BOUND ( 'NONE', #10006, .T. ) ;
#24924 = CARTESIAN_POINT ( 'NONE',  ( -12.82020749880560651, -17.33244462614775827, 50.77966884056655772 ) ) ;
#24925 = CARTESIAN_POINT ( 'NONE',  ( -24.72409385541305582, -15.80920654474410725, 65.99999999999998579 ) ) ;
#24926 = CARTESIAN_POINT ( 'NONE',  ( -13.86159385650551812, -9.295667164867525756, 49.30633214617472504 ) ) ;
#24927 = ORIENTED_EDGE ( 'NONE', *, *, #16936, .T. ) ;
#24928 = ORIENTED_EDGE ( 'NONE', *, *, #17911, .F. ) ;
#24929 = CARTESIAN_POINT ( 'NONE',  ( -14.03870967672415304, -8.172720116890397790, 70.91453050697840865 ) ) ;
#24930 = DIRECTION ( 'NONE',  ( 0.1847813031241905823, -0.9827796650397888634, 7.910442904995644076E-08 ) ) ;
#24931 = ORIENTED_EDGE ( 'NONE', *, *, #9683, .F. ) ;
#24932 = CARTESIAN_POINT ( 'NONE',  ( -23.98503169607928953, -17.39005800936845603, 66.22885190747201989 ) ) ;
#24934 = CARTESIAN_POINT ( 'NONE',  ( -24.72409385541305582, -15.80920654474410725, 65.99999999999998579 ) ) ;
#24933 = CYLINDRICAL_SURFACE ( 'NONE', #29028, 0.1500000000000015488 ) ;
#24935 = CARTESIAN_POINT ( 'NONE',  ( -13.01616685277437391, -9.306763517318227485, 70.86397465682092900 ) ) ;
#24936 = CARTESIAN_POINT ( 'NONE',  ( -19.24025795797341942, -7.996846695050864540, 60.24620885950562865 ) ) ;
#24937 = CARTESIAN_POINT ( 'NONE',  ( -17.92193035392796929, -21.84160718002658541, 61.87535923543195082 ) ) ;
#24938 = EDGE_CURVE ( 'NONE', #43029, #36353, #16847, .T. ) ;
#24939 = EDGE_LOOP ( 'NONE', ( #29025, #43013, #15499, #25036, #19743 ) ) ;
#24940 = FACE_BOUND ( 'NONE', #40238, .T. ) ;
#24941 = CARTESIAN_POINT ( 'NONE',  ( -40.92409385541305511, -15.80920654474410725, 74.99999999999998579 ) ) ;
#24942 = AXIS2_PLACEMENT_3D ( 'NONE', #16745, #38688, #8664 ) ;
#24943 = CARTESIAN_POINT ( 'NONE',  ( -46.92409385541305511, -17.80920654474410370, 60.24999999999999289 ) ) ;
#24944 = CARTESIAN_POINT ( 'NONE',  ( -20.49170831689750827, -8.461258797198503601, 63.59649424907591708 ) ) ;
#24945 = EDGE_CURVE ( 'NONE', #4984, #3647, #2215, .T. ) ;
#24946 = EDGE_LOOP ( 'NONE', ( #18922, #30601, #14121, #12931, #38339 ) ) ;
#24947 = CARTESIAN_POINT ( 'NONE',  ( -11.97224129167519280, -8.309940731205241349, 54.49999999999995026 ) ) ;
#24948 = VECTOR ( 'NONE', #2961, 999.9999999999998863 ) ;
#24949 = CARTESIAN_POINT ( 'NONE',  ( -16.95842795909200618, -7.774453609861648573, 74.25458489456045186 ) ) ;
#24950 = CARTESIAN_POINT ( 'NONE',  ( -20.87593624383936941, -21.41133309587159417, 58.83749320122741722 ) ) ;
#24951 = LINE ( 'NONE', #2053, #40153 ) ;
#24952 = LINE ( 'NONE', #2549, #40158 ) ;
#24953 = ORIENTED_EDGE ( 'NONE', *, *, #24409, .T. ) ;
#24954 = VERTEX_POINT ( 'NONE', #44435 ) ;
#24955 = CARTESIAN_POINT ( 'NONE',  ( -19.37409385541304374, -6.859212275519751323, 50.50378509014259265 ) ) ;
#24956 = CARTESIAN_POINT ( 'NONE',  ( -10.00368807899092971, -15.89896712085359098, 47.99999999999994316 ) ) ;
#24957 = EDGE_CURVE ( 'NONE', #20146, #37066, #7253, .T. ) ;
#24958 = LINE ( 'NONE', #21988, #41787 ) ;
#24959 = ADVANCED_FACE ( 'NONE', ( #15089 ), #105, .T. ) ;
#24960 = FACE_OUTER_BOUND ( 'NONE', #11340, .T. ) ;
#24961 = CARTESIAN_POINT ( 'NONE',  ( -24.38391081516821401, -14.06024225110868464, 73.12271507915593816 ) ) ;
#24962 = ORIENTED_EDGE ( 'NONE', *, *, #33099, .F. ) ;
#24963 = CARTESIAN_POINT ( 'NONE',  ( -20.98580030992770418, -20.83533690608478040, 65.88453944791919525 ) ) ;
#24964 = DIRECTION ( 'NONE',  ( -3.071710424422018668E-17, 6.404604876783312462E-16, 1.000000000000000000 ) ) ;
#24965 = ADVANCED_FACE ( 'NONE', ( #10684 ), #33302, .T. ) ;
#24966 =( BOUNDED_CURVE ( )  B_SPLINE_CURVE ( 3, ( #9854, #40133, #24870, #36411 ),
 .UNSPECIFIED., .F., .F. ) 
 B_SPLINE_CURVE_WITH_KNOTS ( ( 4, 4 ),
 ( 0.000000000000000000, 0.4074455897393582937 ),
 .UNSPECIFIED. ) 
 CURVE ( )  GEOMETRIC_REPRESENTATION_ITEM ( )  RATIONAL_B_SPLINE_CURVE ( ( 1.000000000000000000, 0.4567392136813337444, 0.3561768502900309330, 0.6983129098260915102 ) ) 
 REPRESENTATION_ITEM ( '' )  );
#24967 = VERTEX_POINT ( 'NONE', #41444 ) ;
#24968 = CARTESIAN_POINT ( 'NONE',  ( -24.42173158938954813, -14.58342408866059614, 66.25462932207040012 ) ) ;
#24969 = CARTESIAN_POINT ( 'NONE',  ( -17.82409385541305369, -14.80920654474410725, 52.21286476528345588 ) ) ;
#24970 = AXIS2_PLACEMENT_3D ( 'NONE', #17428, #22103, #32460 ) ;
#24971 = AXIS2_PLACEMENT_3D ( 'NONE', #22667, #37665, #3960 ) ;
#24972 = VERTEX_POINT ( 'NONE', #18295 ) ;
#24973 = DIRECTION ( 'NONE',  ( 0.000000000000000000, 0.000000000000000000, -1.000000000000000000 ) ) ;
#24974 = DIRECTION ( 'NONE',  ( 1.000000000000000000, -0.000000000000000000, 0.000000000000000000 ) ) ;
#24975 = VERTEX_POINT ( 'NONE', #10457 ) ;
#24976 = CARTESIAN_POINT ( 'NONE',  ( -12.43150676794136089, -13.18545343111794033, 49.52966884056655772 ) ) ;
#24977 = CARTESIAN_POINT ( 'NONE',  ( -24.84263255441417328, -14.11714595057820354, 73.30926835346492965 ) ) ;
#24978 = VECTOR ( 'NONE', #15083, 999.9999999999998863 ) ;
#24979 =( BOUNDED_CURVE ( )  B_SPLINE_CURVE ( 2, ( #7238, #18784, #11397, #37731, #18282, #7973, #30375, #48579, #25683 ),
 .UNSPECIFIED., .F., .F. ) 
 B_SPLINE_CURVE_WITH_KNOTS ( ( 3, 2, 2, 2, 3 ),
 ( 0.3333333333333332593, 0.3437499999999998890, 0.3541666666666665741, 0.3645833333333331483, 0.3749999999999998335 ),
 .UNSPECIFIED. ) 
 CURVE ( )  GEOMETRIC_REPRESENTATION_ITEM ( )  RATIONAL_B_SPLINE_CURVE ( ( 1.000000000000000444, 0.9238795325112862944, 1.000000000000000000, 0.9238795325112867385, 1.000000000000000000, 0.9238795325112867385, 1.000000000000000000, 0.9238795325112879597, 0.9999999999999987788 ) ) 
 REPRESENTATION_ITEM ( '' )  );
#24980 = CARTESIAN_POINT ( 'NONE',  ( -16.74292201677715752, -21.77598521546333643, 65.41667504381256038 ) ) ;
#24981 = FACE_OUTER_BOUND ( 'NONE', #43387, .T. ) ;
#24982 = ORIENTED_EDGE ( 'NONE', *, *, #28242, .F. ) ;
#24983 = CARTESIAN_POINT ( 'NONE',  ( -23.79168800850164800, -18.67653690130417132, 72.91368233453137293 ) ) ;
#24984 =( BOUNDED_CURVE ( )  B_SPLINE_CURVE ( 3, ( #10071, #20676, #1949, #9603 ),
 .UNSPECIFIED., .F., .F. ) 
 B_SPLINE_CURVE_WITH_KNOTS ( ( 4, 4 ),
 ( 0.000000000000000000, 0.4074455897393627346 ),
 .UNSPECIFIED. ) 
 CURVE ( )  GEOMETRIC_REPRESENTATION_ITEM ( )  RATIONAL_B_SPLINE_CURVE ( ( 1.000000000000000000, 0.4567392136813296366, 0.3561768502900294342, 0.6983129098260993928 ) ) 
 REPRESENTATION_ITEM ( '' )  );
#24985 = CARTESIAN_POINT ( 'NONE',  ( -45.92409385541305511, -17.80920654474410370, 71.75000000000000000 ) ) ;
#24986 = CARTESIAN_POINT ( 'NONE',  ( -12.27604185553471616, -19.62628656662749549, 58.21210303282668264 ) ) ;
#24987 = CARTESIAN_POINT ( 'NONE',  ( -19.81804402429900236, -8.174913897241847138, 73.60608030023824710 ) ) ;
#24988 = CARTESIAN_POINT ( 'NONE',  ( -22.63659385650551670, -6.915538690918074494, 49.31353937987644542 ) ) ;
#24989 = CARTESIAN_POINT ( 'NONE',  ( -16.57921203443829583, -21.81142124131518756, 69.11049422539112186 ) ) ;
#24990 = DIRECTION ( 'NONE',  ( 0.8565259173193582320, -0.5161040137028850561, 6.301967848571305848E-08 ) ) ;
#24991 = ORIENTED_EDGE ( 'NONE', *, *, #23609, .T. ) ;
#24992 = CARTESIAN_POINT ( 'NONE',  ( -16.57554889599778747, -22.21081103083016117, 65.41059783760971413 ) ) ;
#24993 = CARTESIAN_POINT ( 'NONE',  ( -12.05615918852498680, -19.97535170061420828, 61.51183199568394144 ) ) ;
#24994 = CARTESIAN_POINT ( 'NONE',  ( -13.34910555009277111, -20.50135914746042687, 58.33033577015955728 ) ) ;
#24995 = ADVANCED_FACE ( 'NONE', ( #14579 ), #37010, .T. ) ;
#24996 = ORIENTED_EDGE ( 'NONE', *, *, #11533, .T. ) ;
#24997 = CARTESIAN_POINT ( 'NONE',  ( -10.04612636579397389, -15.84390794478046338, 64.64738251167817396 ) ) ;
#24998 =( BOUNDED_CURVE ( )  B_SPLINE_CURVE ( 3, ( #46891, #38769, #13131, #28182 ),
 .UNSPECIFIED., .F., .F. ) 
 B_SPLINE_CURVE_WITH_KNOTS ( ( 4, 4 ),
 ( 0.5000000000000000000, 0.9074455897393592929 ),
 .UNSPECIFIED. ) 
 CURVE ( )  GEOMETRIC_REPRESENTATION_ITEM ( )  RATIONAL_B_SPLINE_CURVE ( ( 1.000000000000007550, 0.4567392136813483439, 0.3561768502900309330, 0.6983129098260637546 ) ) 
 REPRESENTATION_ITEM ( '' )  );
#24999 = ORIENTED_EDGE ( 'NONE', *, *, #31669, .T. ) ;
#25000 = ORIENTED_EDGE ( 'NONE', *, *, #41438, .F. ) ;
#25001 = EDGE_LOOP ( 'NONE', ( #17221, #31954, #21289, #22279, #42176 ) ) ;
#25002 = CARTESIAN_POINT ( 'NONE',  ( -21.09639645740537617, -17.74003392703708926, 49.52966884056655772 ) ) ;
#25003 = VECTOR ( 'NONE', #35069, 1000.000000000000000 ) ;
#25004 = CARTESIAN_POINT ( 'NONE',  ( -24.22092292145011072, -12.93687797069018153, 66.60246741374322710 ) ) ;
#25005 = CYLINDRICAL_SURFACE ( 'NONE', #15, 0.1500000000000008549 ) ;
#25006 = CARTESIAN_POINT ( 'NONE',  ( -22.62394951084894146, -10.04809318868971424, 70.29706442286226320 ) ) ;
#25007 = VECTOR ( 'NONE', #22556, 1000.000000000000227 ) ;
#25008 = AXIS2_PLACEMENT_3D ( 'NONE', #9670, #24684, #12854 ) ;
#25009 = ORIENTED_EDGE ( 'NONE', *, *, #21348, .F. ) ;
#25010 = ORIENTED_EDGE ( 'NONE', *, *, #15721, .F. ) ;
#25011 = CARTESIAN_POINT ( 'NONE',  ( -18.50534385650551883, -8.801233750844183135, 48.81488406609782515 ) ) ;
#25012 = EDGE_CURVE ( 'NONE', #46722, #37730, #40717, .T. ) ;
#25013 = CARTESIAN_POINT ( 'NONE',  ( -19.80621920301059902, -19.48766556757794177, 52.02966884056656482 ) ) ;
#25014 = VECTOR ( 'NONE', #41391, 1000.000000000000000 ) ;
#25015 = CARTESIAN_POINT ( 'NONE',  ( -24.06395315815399272, -17.02595776467518363, 73.18336026098602076 ) ) ;
#25016 = ADVANCED_FACE ( 'NONE', ( #40474 ), #2804, .T. ) ;
#25017 = CARTESIAN_POINT ( 'NONE',  ( -18.22409385650551528, -6.426201560718813433, 50.50509628382439331 ) ) ;
#25018 = CIRCLE ( 'NONE', #47780, 2.000000000000003109 ) ;
#25019 = ORIENTED_EDGE ( 'NONE', *, *, #37606, .T. ) ;
#25020 = EDGE_CURVE ( 'NONE', #32027, #47544, #33067, .T. ) ;
#25021 = CARTESIAN_POINT ( 'NONE',  ( -23.30963478160716562, -18.69084381296369557, 69.30844128244088154 ) ) ;
#25022 = EDGE_CURVE ( 'NONE', #19030, #13430, #30145, .T. ) ;
#25023 = ORIENTED_EDGE ( 'NONE', *, *, #11020, .F. ) ;
#25024 = FACE_OUTER_BOUND ( 'NONE', #32944, .T. ) ;
#25025 = EDGE_LOOP ( 'NONE', ( #21893, #30222 ) ) ;
#25026 = DIRECTION ( 'NONE',  ( 0.9629498065864410261, 0.2696806815386222911, 3.246020392366875918E-17 ) ) ;
#25027 = CARTESIAN_POINT ( 'NONE',  ( -11.29476715451500723, -19.04418240398407391, 68.47335581180095687 ) ) ;
#25028 = CARTESIAN_POINT ( 'NONE',  ( -21.09639645740537617, -17.74003392703708926, 49.52966884056655772 ) ) ;
#25029 = VERTEX_POINT ( 'NONE', #29400 ) ;
#25030 = VECTOR ( 'NONE', #12078, 1000.000000000000114 ) ;
#25031 = CARTESIAN_POINT ( 'NONE',  ( -19.24025795797341942, -7.996846695050864540, 60.24620885950562865 ) ) ;
#25032 = VECTOR ( 'NONE', #2530, 1000.000000000000000 ) ;
#25033 = ADVANCED_FACE ( 'NONE', ( #36519 ), #21767, .T. ) ;
#25034 = CARTESIAN_POINT ( 'NONE',  ( -33.42409385541304800, -8.109206544743658540, 50.50000000000030553 ) ) ;
#25035 = FACE_OUTER_BOUND ( 'NONE', #13578, .T. ) ;
#25036 = ORIENTED_EDGE ( 'NONE', *, *, #47532, .F. ) ;
#25037 = CARTESIAN_POINT ( 'NONE',  ( -20.64396943983181743, -21.02470340508176250, 58.94475165022391394 ) ) ;
#25038 = AXIS2_PLACEMENT_3D ( 'NONE', #11733, #41776, #37079 ) ;
#25040 = DIRECTION ( 'NONE',  ( -3.071710424422018668E-17, 6.404604876783312462E-16, 1.000000000000000000 ) ) ;
#25039 = AXIS2_PLACEMENT_3D ( 'NONE', #34170, #41830, #23116 ) ;
#25041 = ADVANCED_FACE ( 'NONE', ( #29897 ), #48111, .T. ) ;
#25042 = ORIENTED_EDGE ( 'NONE', *, *, #12884, .F. ) ;
#25043 = CARTESIAN_POINT ( 'NONE',  ( -15.15660932275500095, -21.48492473237050859, 65.39124617759186719 ) ) ;
#25044 = CARTESIAN_POINT ( 'NONE',  ( -18.53201889041905659, -7.846807422456379300, 73.99064401781672018 ) ) ;
#25045 = ORIENTED_EDGE ( 'NONE', *, *, #31080, .T. ) ;
#25046 = DIRECTION ( 'NONE',  ( 0.7224352045700188629, 0.6914386272098739239, -9.340627245513718311E-09 ) ) ;
#25047 = CARTESIAN_POINT ( 'NONE',  ( -13.57572078670752447, -20.65643022133334128, 61.81646323932617548 ) ) ;
#25048 = B_SPLINE_CURVE_WITH_KNOTS ( 'NONE', 1,
 ( #25237, #8837 ),
 .UNSPECIFIED., .F., .F.,
 ( 2, 2 ),
 ( 0.000000000000000000, 1.000000000000000000 ),
 .UNSPECIFIED. ) ;
#25049 = EDGE_LOOP ( 'NONE', ( #32849, #15570, #32845, #23577, #14255 ) ) ;
#25050 = CYLINDRICAL_SURFACE ( 'NONE', #3226, 2.500000000000000444 ) ;
#25051 = VECTOR ( 'NONE', #30200, 1000.000000000000000 ) ;
#25052 = CARTESIAN_POINT ( 'NONE',  ( -18.97799580819609844, -7.523008705935653850, 67.09345912586260852 ) ) ;
#25053 = ADVANCED_FACE ( 'NONE', ( #37494 ), #36753, .T. ) ;
#25054 = CARTESIAN_POINT ( 'NONE',  ( -23.38308684513804891, -18.48213489539728371, 69.48475052504386440 ) ) ;
#25055 = ORIENTED_EDGE ( 'NONE', *, *, #9875, .T. ) ;
#25056 = CARTESIAN_POINT ( 'NONE',  ( -10.18401502636761968, -13.05277926903019470, 71.32333192088977114 ) ) ;
#25057 = CARTESIAN_POINT ( 'NONE',  ( -24.77581774434673889, -16.01560321267006159, 66.16986595299408691 ) ) ;
#25058 = EDGE_LOOP ( 'NONE', ( #43947, #45838 ) ) ;
#25059 = VERTEX_POINT ( 'NONE', #18798 ) ;
#25060 = CARTESIAN_POINT ( 'NONE',  ( -10.70034849704600788, -12.85632423166505944, 67.92759470734964111 ) ) ;
#25061 = CARTESIAN_POINT ( 'NONE',  ( -15.69736699998981422, -8.025519224215527103, 70.60989840319118116 ) ) ;
#25062 = CARTESIAN_POINT ( 'NONE',  ( -13.18342752238402582, -20.93459749068556874, 58.09004124675303160 ) ) ;
#25063 = CARTESIAN_POINT ( 'NONE',  ( -10.48020486909296523, -13.57339180249324784, 74.56328874061136958 ) ) ;
#25064 = DIRECTION ( 'NONE',  ( -5.731567514496413899E-31, -1.020425574103664789E-16, -1.000000000000000000 ) ) ;
#25065 = CYLINDRICAL_SURFACE ( 'NONE', #29898, 0.1499999999999995226 ) ;
#25066 = CYLINDRICAL_SURFACE ( 'NONE', #39699, 5.249999999999998224 ) ;
#25067 = EDGE_CURVE ( 'NONE', #24678, #42690, #18543, .T. ) ;
#25068 = CARTESIAN_POINT ( 'NONE',  ( -17.84735443592641602, -7.371153788697909270, 60.19565345827741965 ) ) ;
#25069 = ORIENTED_EDGE ( 'NONE', *, *, #961, .T. ) ;
#25070 = ORIENTED_EDGE ( 'NONE', *, *, #45007, .F. ) ;
#25071 = CARTESIAN_POINT ( 'NONE',  ( -24.46809763383182101, -15.25302497427750303, 73.15870697135122214 ) ) ;
#25072 = CARTESIAN_POINT ( 'NONE',  ( 25.57590614458706568, 1.904620652374673151, 48.58033007082241994 ) ) ;
#25073 = VECTOR ( 'NONE', #21229, 1000.000000000000000 ) ;
#25074 = CARTESIAN_POINT ( 'NONE',  ( -14.92764441971231726, -21.34891144748960201, 61.93600440564248544 ) ) ;
#25075 = CARTESIAN_POINT ( 'NONE',  ( -10.97013626231024830, -17.52378408739619431, 71.75645163686851902 ) ) ;
#25076 =( BOUNDED_CURVE ( )  B_SPLINE_CURVE ( 3, ( #11296, #44796, #22882, #45050 ),
 .UNSPECIFIED., .F., .F. ) 
 B_SPLINE_CURVE_WITH_KNOTS ( ( 4, 4 ),
 ( 6.147240100468662760, 6.419130513890517697 ),
 .UNSPECIFIED. ) 
 CURVE ( )  GEOMETRIC_REPRESENTATION_ITEM ( )  RATIONAL_B_SPLINE_CURVE ( ( 1.000000000000000000, 0.9938491152766115722, 0.9938491152766115722, 1.000000000000000000 ) ) 
 REPRESENTATION_ITEM ( '' )  );
#25077 = CARTESIAN_POINT ( 'NONE',  ( -21.43863153483710349, -12.36809147865652925, 49.52966884056655772 ) ) ;
#25078 = CARTESIAN_POINT ( 'NONE',  ( -19.14909385650551954, -8.104110260919579645, 48.81699501597546487 ) ) ;
#25079 = VECTOR ( 'NONE', #31409, 1000.000000000000000 ) ;
#25080 = ORIENTED_EDGE ( 'NONE', *, *, #21678, .F. ) ;
#25081 = EDGE_CURVE ( 'NONE', #7578, #8735, #33548, .T. ) ;
#25082 = CARTESIAN_POINT ( 'NONE',  ( -15.10203878652056630, -21.46900354431040725, 61.52111843893123933 ) ) ;
#25083 =( NAMED_UNIT ( * ) PLANE_ANGLE_UNIT ( ) SI_UNIT ( $, .RADIAN. ) );
#25084 = EDGE_CURVE ( 'NONE', #29468, #19879, #20552, .T. ) ;
#25085 = CARTESIAN_POINT ( 'NONE',  ( -14.72744631621160494, -8.295007313424175521, 60.60524229057013201 ) ) ;
#25086 = CARTESIAN_POINT ( 'NONE',  ( -11.21364313603757168, -18.92425114470789538, 64.93981204116175832 ) ) ;
#25087 = AXIS2_PLACEMENT_3D ( 'NONE', #20137, #1173, #5622 ) ;
#25088 = ORIENTED_EDGE ( 'NONE', *, *, #11527, .F. ) ;
#25089 = CARTESIAN_POINT ( 'NONE',  ( -13.76849323099554567, -20.83774554052356365, 65.27156739751333703 ) ) ;
#25090 = PLANE ( 'NONE',  #38448 ) ;
#25091 = EDGE_CURVE ( 'NONE', #10114, #2367, #43636, .T. ) ;
#25092 = LINE ( 'NONE', #40348, #23624 ) ;
#25093 = VERTEX_POINT ( 'NONE', #42436 ) ;
#25094 = DIRECTION ( 'NONE',  ( 0.07061531369766044230, 0.9975036227860933913, 1.268851335910971019E-08 ) ) ;
#25095 = EDGE_CURVE ( 'NONE', #45181, #26808, #4760, .T. ) ;
#25096 = ORIENTED_EDGE ( 'NONE', *, *, #12349, .F. ) ;
#25097 = DIRECTION ( 'NONE',  ( -0.000000000000000000, -1.000000000000000000, -0.000000000000000000 ) ) ;
#25098 = DIRECTION ( 'NONE',  ( 0.000000000000000000, 0.000000000000000000, 1.000000000000000000 ) ) ;
#25099 = ORIENTED_EDGE ( 'NONE', *, *, #19073, .F. ) ;
#25100 = EDGE_CURVE ( 'NONE', #115, #38493, #23480, .T. ) ;
#25101 = EDGE_CURVE ( 'NONE', #15953, #1752, #17970, .T. ) ;
#25102 = EDGE_CURVE ( 'NONE', #32937, #37435, #43008, .T. ) ;
#25103 = CARTESIAN_POINT ( 'NONE',  ( -11.05034076241727625, -11.79557573020262318, 71.37388789199357575 ) ) ;
#25104 = CARTESIAN_POINT ( 'NONE',  ( -12.61446418420489124, -20.49964817803554595, 71.91998392462126333 ) ) ;
#25105 = VERTEX_POINT ( 'NONE', #19286 ) ;
#25106 = DIRECTION ( 'NONE',  ( 0.5589780652556124441, -0.8291824422665291516, 7.938832475108296738E-08 ) ) ;
#25107 = CARTESIAN_POINT ( 'NONE',  ( -16.93025400261081614, -7.375423323426211653, 74.12051638600156878 ) ) ;
#25108 = CARTESIAN_POINT ( 'NONE',  ( -45.92409385541306222, 12.69079345525585545, 70.50000000000000000 ) ) ;
#25109 = ORIENTED_EDGE ( 'NONE', *, *, #37983, .T. ) ;
#25110 = CARTESIAN_POINT ( 'NONE',  ( -17.11594671439511828, -7.315539529225058679, 54.27966884056655061 ) ) ;
#25111 = AXIS2_PLACEMENT_3D ( 'NONE', #6235, #43181, #17297 ) ;
#25112 = AXIS2_PLACEMENT_3D ( 'NONE', #45833, #41151, #38169 ) ;
#25113 = CARTESIAN_POINT ( 'NONE',  ( -24.72409385541305582, -15.80920654474410725, 65.99999999999998579 ) ) ;
#25114 = CARTESIAN_POINT ( 'NONE',  ( -23.29918339618657086, -19.39037464299967439, 58.99915238703562181 ) ) ;
#25115 = CARTESIAN_POINT ( 'NONE',  ( -23.38410522734749009, -10.33907873996118276, 59.71708144416061970 ) ) ;
#25116 = ORIENTED_EDGE ( 'NONE', *, *, #33091, .T. ) ;
#25117 = ORIENTED_EDGE ( 'NONE', *, *, #32459, .T. ) ;
#25118 = CARTESIAN_POINT ( 'NONE',  ( -22.53429316287767392, -9.952421288698296564, 73.63161091678163928 ) ) ;
#25119 = CARTESIAN_POINT ( 'NONE',  ( -21.42336286209559759, -21.09487474236010485, 69.23945462178221533 ) ) ;
#25120 = VERTEX_POINT ( 'NONE', #27165 ) ;
#25121 = CARTESIAN_POINT ( 'NONE',  ( -10.44568875397917296, -15.81166898614220706, 64.50771614034250945 ) ) ;
#25122 = AXIS2_PLACEMENT_3D ( 'NONE', #23487, #38484, #36240 ) ;
#25123 = CARTESIAN_POINT ( 'NONE',  ( -20.02409385759798965, -9.359200813967568422, 50.49621490985803263 ) ) ;
#25124 = CARTESIAN_POINT ( 'NONE',  ( -10.03035368457962662, -15.72374687363213575, 61.22284448286259817 ) ) ;
#25125 =( BOUNDED_CURVE ( )  B_SPLINE_CURVE ( 3, ( #37517, #41230, #45913, #7518 ),
 .UNSPECIFIED., .F., .F. ) 
 B_SPLINE_CURVE_WITH_KNOTS ( ( 4, 4 ),
 ( 0.000000000000000000, 0.4074455897393693959 ),
 .UNSPECIFIED. ) 
 CURVE ( )  GEOMETRIC_REPRESENTATION_ITEM ( )  RATIONAL_B_SPLINE_CURVE ( ( 1.000000000000000000, 0.4567392136813228087, 0.3561768502900268807, 0.6983129098261122714 ) ) 
 REPRESENTATION_ITEM ( '' )  );
#25126 = CARTESIAN_POINT ( 'NONE',  ( -16.93783521594581387, -21.79229702504021304, 68.80446639304301470 ) ) ;
#25127 = LINE ( 'NONE', #9865, #33337 ) ;
#25128 = ORIENTED_EDGE ( 'NONE', *, *, #11208, .F. ) ;
#25129 = CARTESIAN_POINT ( 'NONE',  ( -13.38462656077074442, -20.58719956993326861, 58.19650077713541947 ) ) ;
#25130 = EDGE_CURVE ( 'NONE', #4347, #3170, #34514, .T. ) ;
#25131 = CARTESIAN_POINT ( 'NONE',  ( -13.95122194917832914, -8.664767797030865637, 70.88524802578001527 ) ) ;
#25132 = CARTESIAN_POINT ( 'NONE',  ( -14.81380287721095357, -8.256357904232213940, 63.88158797558475754 ) ) ;
#25133 = DIRECTION ( 'NONE',  ( 2.866981220435666553E-17, -1.000000000000000000, -1.190614954331866791E-16 ) ) ;
#25134 =( BOUNDED_SURFACE ( )  B_SPLINE_SURFACE ( 3, 1, ( 
 ( #10667, #40692 ),
 ( #3022, #18277 ),
 ( #48573, #44649 ),
 ( #25931, #37228 ),
 ( #22477, #47616 ),
 ( #13847, #25207 ),
 ( #17790, #30125 ) ),
 .UNSPECIFIED., .T., .F., .F. ) 
 B_SPLINE_SURFACE_WITH_KNOTS ( ( 4, 3, 4 ),
 ( 2, 2 ),
 ( 0.000000000000000000, 0.5000000000000000000, 1.000000000000000000 ),
 ( 0.000000000000000000, 1.000000000000000000 ),
 .UNSPECIFIED. ) 
 GEOMETRIC_REPRESENTATION_ITEM ( )  RATIONAL_B_SPLINE_SURFACE ( (
 ( 1.000000000000000000, 1.000000000000000000),
 ( 0.3333333333333335369, 0.3333333333333330373),
 ( 0.3333333333333335369, 0.3333333333333330373),
 ( 1.000000000000000000, 1.000000000000000000),
 ( 0.3333333333333333703, 0.3333333333333333703),
 ( 0.3333333333333333703, 0.3333333333333333703),
 ( 1.000000000000000000, 1.000000000000000000) ) ) 
 REPRESENTATION_ITEM ( '' )  SURFACE ( )  );
#25135 = ORIENTED_EDGE ( 'NONE', *, *, #38105, .T. ) ;
#25136 = VERTEX_POINT ( 'NONE', #35022 ) ;
#25137 = CARTESIAN_POINT ( 'NONE',  ( -24.46506320217640962, -17.24406362331221132, 72.99840605271779737 ) ) ;
#25138 =( NAMED_UNIT ( * ) SI_UNIT ( $, .STERADIAN. ) SOLID_ANGLE_UNIT ( ) );
#25139 = AXIS2_PLACEMENT_3D ( 'NONE', #41931, #8207, #23224 ) ;
#25140 = DIRECTION ( 'NONE',  ( 8.560949391518745609E-06, -2.380493834460222846E-06, 0.9999999999605218015 ) ) ;
#25141 = ORIENTED_EDGE ( 'NONE', *, *, #38238, .F. ) ;
#25142 = VECTOR ( 'NONE', #10753, 1000.000000000000000 ) ;
#25143 = CARTESIAN_POINT ( 'NONE',  ( -24.24928796324336133, -13.25435532323388976, 59.37770298071973230 ) ) ;
#25144 = CARTESIAN_POINT ( 'NONE',  ( -23.75797251732913296, -17.78947179557082592, 59.00378417803962350 ) ) ;
#25145 = ORIENTED_EDGE ( 'NONE', *, *, #34457, .F. ) ;
#25146 = CARTESIAN_POINT ( 'NONE',  ( -11.27262641912073882, -11.35749776731469218, 67.91864759325788725 ) ) ;
#25147 = AXIS2_PLACEMENT_3D ( 'NONE', #2286, #32343, #47365 ) ;
#25148 = CARTESIAN_POINT ( 'NONE',  ( -12.99758137947571157, -9.386477775907486887, 71.14925353122600882 ) ) ;
#25149 = CARTESIAN_POINT ( 'NONE',  ( -23.37084835027744489, -10.32157900363995573, 59.70229188760873740 ) ) ;
#25150 = ORIENTED_EDGE ( 'NONE', *, *, #15112, .T. ) ;
#25151 = CARTESIAN_POINT ( 'NONE',  ( -24.11794058161805054, -12.76166764465371628, 69.77243002474142486 ) ) ;
#25152 = EDGE_LOOP ( 'NONE', ( #47860, #21503, #26812, #33999, #45480 ) ) ;
#25153 = CARTESIAN_POINT ( 'NONE',  ( -24.34502386579654498, -17.56683345968398768, 66.12852568699506151 ) ) ;
#25154 = DIRECTION ( 'NONE',  ( -0.7171836970970659753, 0.6968841687240312499, -4.479616660400631173E-09 ) ) ;
#25155 = CARTESIAN_POINT ( 'NONE',  ( -19.30025855022017112, -21.55315516297060441, 58.54009773080257872 ) ) ;
#25156 = B_SPLINE_CURVE_WITH_KNOTS ( 'NONE', 1,
 ( #9165, #17255 ),
 .UNSPECIFIED., .F., .F.,
 ( 2, 2 ),
 ( 0.000000000000000000, 1.000000000000000000 ),
 .UNSPECIFIED. ) ;
#25157 = EDGE_LOOP ( 'NONE', ( #21643, #32742 ) ) ;
#25158 = DIRECTION ( 'NONE',  ( 0.2479245821708712660, 0.9687793358424811041, 0.000000000000000000 ) ) ;
#25159 = EDGE_CURVE ( 'NONE', #20248, #34217, #31622, .T. ) ;
#25160 = EDGE_CURVE ( 'NONE', #27722, #6597, #16479, .T. ) ;
#25161 = CARTESIAN_POINT ( 'NONE',  ( -23.68653687815194786, -11.57061008776568123, 66.43686604568146947 ) ) ;
#25162 = PLANE ( 'NONE',  #10042 ) ;
#25163 = FACE_OUTER_BOUND ( 'NONE', #1296, .T. ) ;
#25164 = CARTESIAN_POINT ( 'NONE',  ( -13.41559485503361948, -8.529420403834853559, 57.08472365561223683 ) ) ;
#25165 = ORIENTED_EDGE ( 'NONE', *, *, #38290, .T. ) ;
#25166 = DIRECTION ( 'NONE',  ( -1.000000000000000000, -1.669677910507523057E-21, -6.493791346278465266E-22 ) ) ;
#25167 = CARTESIAN_POINT ( 'NONE',  ( -11.68672781637937419, -10.05669048882576533, 67.68392176937598492 ) ) ;
#25168 = CARTESIAN_POINT ( 'NONE',  ( -14.78754716229542687, -8.270772359302402066, 60.31996282000579157 ) ) ;
#25169 = ADVANCED_FACE ( 'NONE', ( #22756 ), #38476, .T. ) ;
#25170 = EDGE_CURVE ( 'NONE', #24138, #47558, #45545, .T. ) ;
#25171 = CARTESIAN_POINT ( 'NONE',  ( -45.92409385541306932, -16.70920654474410938, 70.50000000000000000 ) ) ;
#25172 = CARTESIAN_POINT ( 'NONE',  ( -10.77303329795002895, -12.62668660113453178, 60.79853568451941470 ) ) ;
#25173 = CARTESIAN_POINT ( 'NONE',  ( -11.87700371968174551, -10.45801594763104170, 71.26893088143391708 ) ) ;
#25174 = ORIENTED_EDGE ( 'NONE', *, *, #31104, .T. ) ;
#25175 = ORIENTED_EDGE ( 'NONE', *, *, #38698, .F. ) ;
#25176 = VECTOR ( 'NONE', #45772, 1000.000000000000000 ) ;
#25177 = CARTESIAN_POINT ( 'NONE',  ( -21.06702863216100141, -20.84540773593991148, 65.86981821684420879 ) ) ;
#25178 = CYLINDRICAL_SURFACE ( 'NONE', #24221, 1.999999999999999556 ) ;
#25179 = VERTEX_POINT ( 'NONE', #342 ) ;
#25181 = CARTESIAN_POINT ( 'NONE',  ( -11.70868151386493672, -18.85353134555335330, 71.87613056707397163 ) ) ;
#25180 = CARTESIAN_POINT ( 'NONE',  ( -10.11824992584547545, -16.26811798947522192, 71.56255103782838489 ) ) ;
#25182 = CARTESIAN_POINT ( 'NONE',  ( -20.37299714182665866, -8.405577154986387356, 67.08104082189564110 ) ) ;
#25183 = CARTESIAN_POINT ( 'NONE',  ( -23.75797251732913296, -17.78947179557082592, 59.00378417803962350 ) ) ;
#25184 = PLANE ( 'NONE',  #45472 ) ;
#25185 = ORIENTED_EDGE ( 'NONE', *, *, #10917, .F. ) ;
#25186 = CARTESIAN_POINT ( 'NONE',  ( -24.40614610099494541, -15.84163519271677956, 62.74895499471147531 ) ) ;
#25187 = DIRECTION ( 'NONE',  ( 1.000000000000000000, -1.224646799147353207E-16, 4.267285103686821372E-17 ) ) ;
#25188 = AXIS2_PLACEMENT_3D ( 'NONE', #9754, #29182, #2596 ) ;
#25189 = CARTESIAN_POINT ( 'NONE',  ( -15.56465948913147557, -7.543361525925788236, 53.49999999999994316 ) ) ;
#25190 =( BOUNDED_CURVE ( )  B_SPLINE_CURVE ( 3, ( #32824, #29884, #44916, #29146 ),
 .UNSPECIFIED., .F., .F. ) 
 B_SPLINE_CURVE_WITH_KNOTS ( ( 4, 4 ),
 ( 0.000000000000000000, 0.4074455897393656212 ),
 .UNSPECIFIED. ) 
 CURVE ( )  GEOMETRIC_REPRESENTATION_ITEM ( )  RATIONAL_B_SPLINE_CURVE ( ( 1.000000000000000000, 0.4567392136813309689, 0.3561768502900299338, 0.6983129098260969503 ) ) 
 REPRESENTATION_ITEM ( '' )  );
#25191 = DIRECTION ( 'NONE',  ( 3.071710424422018668E-17, -6.404604876783312462E-16, -1.000000000000000000 ) ) ;
#25192 = ADVANCED_FACE ( 'NONE', ( #15571 ), #15328, .T. ) ;
#25193 = ORIENTED_EDGE ( 'NONE', *, *, #35992, .T. ) ;
#25194 = DIRECTION ( 'NONE',  ( 0.9990515194385546360, 0.04354378839186318767, -1.103613758316045351E-08 ) ) ;
#25195 = CARTESIAN_POINT ( 'NONE',  ( -16.84865286310842336, -21.83598151670433296, 68.98088545748413480 ) ) ;
#25196 = VECTOR ( 'NONE', #8301, 1000.000000000000000 ) ;
#25197 = CARTESIAN_POINT ( 'NONE',  ( -24.29765692699610113, -13.47630289685046279, 59.55195110948075410 ) ) ;
#25198 = CARTESIAN_POINT ( 'NONE',  ( -20.81244001423283407, -21.44422669384312741, 58.76758266138310915 ) ) ;
#25199 = CARTESIAN_POINT ( 'NONE',  ( -10.98892314574976226, -11.92244160250971419, 70.97372176798174337 ) ) ;
#25200 = LINE ( 'NONE', #36014, #12598 ) ;
#25201 = ORIENTED_EDGE ( 'NONE', *, *, #20168, .F. ) ;
#25202 = ORIENTED_EDGE ( 'NONE', *, *, #26062, .T. ) ;
#25203 = CARTESIAN_POINT ( 'NONE',  ( -18.98034385541303948, -9.360768649639302552, 51.01397948905922419 ) ) ;
#25204 = CARTESIAN_POINT ( 'NONE',  ( -48.42409385541304800, -25.10920654474410441, 79.99999999999998579 ) ) ;
#25205 = CARTESIAN_POINT ( 'NONE',  ( -11.73260633559210042, -10.00184260618991416, 67.61401560909513364 ) ) ;
#25206 = CARTESIAN_POINT ( 'NONE',  ( -21.73098984888145679, -8.730191469543168381, 70.31627926275058371 ) ) ;
#25207 = CARTESIAN_POINT ( 'NONE',  ( -16.09495291808068274, -22.13976250616876840, 58.54231521589509413 ) ) ;
#25208 = ORIENTED_EDGE ( 'NONE', *, *, #46453, .T. ) ;
#25209 = CIRCLE ( 'NONE', #36989, 2.000000000000000888 ) ;
#25210 = CYLINDRICAL_SURFACE ( 'NONE', #7151, 0.1500000000000029365 ) ;
#25211 = CARTESIAN_POINT ( 'NONE',  ( -20.78451513435706133, -21.00713107796517320, 62.12943504870421663 ) ) ;
#25212 = ORIENTED_EDGE ( 'NONE', *, *, #26564, .F. ) ;
#25213 = CARTESIAN_POINT ( 'NONE',  ( -20.60192465206874246, -18.25372010660273503, 49.52966884056656482 ) ) ;
#25214 = AXIS2_PLACEMENT_3D ( 'NONE', #36720, #29125, #47116 ) ;
#25215 = CARTESIAN_POINT ( 'NONE',  ( -15.47038549838128674, -21.58309193914155344, 72.19575460769013375 ) ) ;
#25216 = ORIENTED_EDGE ( 'NONE', *, *, #29778, .T. ) ;
#25217 = CARTESIAN_POINT ( 'NONE',  ( -19.10745041116545906, -21.66349580942223341, 62.13936675129127707 ) ) ;
#25218 = LINE ( 'NONE', #39507, #29892 ) ;
#25219 = LINE ( 'NONE', #17801, #40695 ) ;
#25220 = VERTEX_POINT ( 'NONE', #45400 ) ;
#25221 = CYLINDRICAL_SURFACE ( 'NONE', #39560, 1.999999999999999112 ) ;
#25222 = EDGE_CURVE ( 'NONE', #32553, #23280, #41944, .T. ) ;
#25223 = LINE ( 'NONE', #40248, #2951 ) ;
#25224 = CIRCLE ( 'NONE', #16562, 1.999999999999999556 ) ;
#25225 = CARTESIAN_POINT ( 'NONE',  ( -16.67010138129746721, -21.76854072801680928, 65.24066787124687039 ) ) ;
#25226 = CARTESIAN_POINT ( 'NONE',  ( -10.72530867274958410, -17.00760959713300835, 57.97288447305809456 ) ) ;
#25227 = VERTEX_POINT ( 'NONE', #38223 ) ;
#25228 = LINE ( 'NONE', #27941, #15595 ) ;
#25229 = DIRECTION ( 'NONE',  ( 2.866981220435666553E-17, -1.000000000000000000, -1.190614954331866791E-16 ) ) ;
#25230 = CARTESIAN_POINT ( 'NONE',  ( -24.94227079592050345, -14.76255220537544233, 53.76227901944321275 ) ) ;
#25231 = EDGE_CURVE ( 'NONE', #18094, #14812, #4507, .T. ) ;
#25232 = CARTESIAN_POINT ( 'NONE',  ( -21.68034385650551599, -6.424090610841176385, 49.80797279389978627 ) ) ;
#25233 = VECTOR ( 'NONE', #45388, 1000.000000000000000 ) ;
#25234 = EDGE_CURVE ( 'NONE', #7245, #47302, #21208, .T. ) ;
#25235 = B_SPLINE_CURVE_WITH_KNOTS ( 'NONE', 3,
 ( #17245, #2948, #32040, #13546, #14259, #43126, #1999, #9397, #36202, #2484 ),
 .UNSPECIFIED., .F., .F.,
 ( 4, 2, 2, 2, 4 ),
 ( 0.000000000000000000, 0.2500000000000000000, 0.5000000000000000000, 0.7500000000000000000, 1.000000000000000000 ),
 .UNSPECIFIED. ) ;
#25236 = FACE_OUTER_BOUND ( 'NONE', #8828, .T. ) ;
#25237 = CARTESIAN_POINT ( 'NONE',  ( -22.83929682888979329, -10.29453308790037980, 66.55654356380499337 ) ) ;
#25238 = EDGE_LOOP ( 'NONE', ( #28569, #24058, #10023, #14373, #7416 ) ) ;
#25239 = DIRECTION ( 'NONE',  ( -0.04287186434519785205, -0.9990805789562556827, 2.806673972535349411E-09 ) ) ;
#25240 = EDGE_CURVE ( 'NONE', #32808, #27374, #28382, .T. ) ;
#25241 = CARTESIAN_POINT ( 'NONE',  ( -18.57335281209669731, -21.76520412651811043, 72.57038810541313012 ) ) ;
#25242 = DIRECTION ( 'NONE',  ( -2.866981220435666553E-17, 1.000000000000000000, 1.190614954331866791E-16 ) ) ;
#25243 = ORIENTED_EDGE ( 'NONE', *, *, #9217, .F. ) ;
#25244 = CARTESIAN_POINT ( 'NONE',  ( -24.16575310113231012, -12.74704012323608104, 70.07243002239955842 ) ) ;
#25245 = VECTOR ( 'NONE', #11505, 1000.000000000000000 ) ;
#25246 = EDGE_LOOP ( 'NONE', ( #5811, #42939, #13886, #37060, #27363, #45997 ) ) ;
#25247 = ORIENTED_EDGE ( 'NONE', *, *, #36881, .F. ) ;
#25248 = ORIENTED_EDGE ( 'NONE', *, *, #34271, .T. ) ;
#25250 = CARTESIAN_POINT ( 'NONE',  ( -16.15307827456697254, -21.74383799326970390, 58.29145396122345346 ) ) ;
#25249 = AXIS2_PLACEMENT_3D ( 'NONE', #19852, #34853, #31894 ) ;
#25251 = CARTESIAN_POINT ( 'NONE',  ( -36.42409385541304800, -9.359200813967566646, 50.49621490985803263 ) ) ;
#25252 = DIRECTION ( 'NONE',  ( 3.892913445306193086E-06, 4.639959643356220421E-06, 0.9999999999816580054 ) ) ;
#25253 = LINE ( 'NONE', #7022, #35407 ) ;
#25254 = VECTOR ( 'NONE', #37108, 1000.000000000000000 ) ;
#25255 = VERTEX_POINT ( 'NONE', #28848 ) ;
#25256 = ORIENTED_EDGE ( 'NONE', *, *, #26946, .T. ) ;
#25257 = CARTESIAN_POINT ( 'NONE',  ( -17.32409385650551314, -6.426201560718813433, 50.50509628382439331 ) ) ;
#25258 = CARTESIAN_POINT ( 'NONE',  ( -20.13271805750754595, -8.299978134201072777, 70.53628287813307907 ) ) ;
#25259 = CYLINDRICAL_SURFACE ( 'NONE', #13408, 0.1500000000000040190 ) ;
#25260 =( BOUNDED_CURVE ( )  B_SPLINE_CURVE ( 3, ( #21478, #39939, #5497, #35989 ),
 .UNSPECIFIED., .F., .F. ) 
 B_SPLINE_CURVE_WITH_KNOTS ( ( 4, 4 ),
 ( 0.000000000000000000, 0.4074455897393639559 ),
 .UNSPECIFIED. ) 
 CURVE ( )  GEOMETRIC_REPRESENTATION_ITEM ( )  RATIONAL_B_SPLINE_CURVE ( ( 1.000000000000000000, 0.4567392136813363535, 0.3561768502900319322, 0.6983129098260867362 ) ) 
 REPRESENTATION_ITEM ( '' )  );
#25261 = CARTESIAN_POINT ( 'NONE',  ( -19.29284385650551670, -7.406986770994973490, 48.81910596585309747 ) ) ;
#25262 = ORIENTED_EDGE ( 'NONE', *, *, #25067, .T. ) ;
#25263 = CARTESIAN_POINT ( 'NONE',  ( -15.40811923343076906, -21.56513327689926030, 72.06047564147742435 ) ) ;
#25264 = VECTOR ( 'NONE', #22609, 999.9999999999998863 ) ;
#25266 = DIRECTION ( 'NONE',  ( 0.7658821528503445553, 0.6346126762488748518, 0.1033986416233889927 ) ) ;
#25265 = B_SPLINE_CURVE_WITH_KNOTS ( 'NONE', 1,
 ( #10809, #25829 ),
 .UNSPECIFIED., .F., .F.,
 ( 2, 2 ),
 ( 0.000000000000000000, 1.000000000000000000 ),
 .UNSPECIFIED. ) ;
#25267 = ADVANCED_FACE ( 'NONE', ( #20255 ), #43408, .T. ) ;
#25268 = ORIENTED_EDGE ( 'NONE', *, *, #8674, .F. ) ;
#25269 = DIRECTION ( 'NONE',  ( -0.7107718805962432995, -0.7034225854731134264, -7.722840056494081040E-09 ) ) ;
#25270 =( BOUNDED_SURFACE ( )  B_SPLINE_SURFACE ( 3, 1, ( 
 ( #8238, #23022 ),
 ( #38006, #19304 ),
 ( #15589, #23252 ),
 ( #47364, #1807 ),
 ( #16807, #24712 ),
 ( #39717, #31846 ),
 ( #5262, #21256 ) ),
 .UNSPECIFIED., .T., .F., .F. ) 
 B_SPLINE_SURFACE_WITH_KNOTS ( ( 4, 3, 4 ),
 ( 2, 2 ),
 ( 0.000000000000000000, 0.5000000000000000000, 1.000000000000000000 ),
 ( 0.000000000000000000, 1.000000000000000000 ),
 .UNSPECIFIED. ) 
 GEOMETRIC_REPRESENTATION_ITEM ( )  RATIONAL_B_SPLINE_SURFACE ( (
 ( 1.000000000000000000, 1.000000000000000000),
 ( 0.3333333333333335369, 0.3333333333333330373),
 ( 0.3333333333333335369, 0.3333333333333330373),
 ( 1.000000000000000000, 1.000000000000000000),
 ( 0.3333333333333333703, 0.3333333333333333703),
 ( 0.3333333333333333703, 0.3333333333333333703),
 ( 1.000000000000000000, 1.000000000000000000) ) ) 
 REPRESENTATION_ITEM ( '' )  SURFACE ( )  );
#25271 = ORIENTED_EDGE ( 'NONE', *, *, #34483, .F. ) ;
#25272 = AXIS2_PLACEMENT_3D ( 'NONE', #25856, #14492, #40617 ) ;
#25273 = CARTESIAN_POINT ( 'NONE',  ( -12.44869005970189058, -9.885249076858732664, 57.08935532200567309 ) ) ;
#25274 = CARTESIAN_POINT ( 'NONE',  ( -11.45045256087476027, -18.56827314959498310, 68.36122809857093330 ) ) ;
#25275 = CARTESIAN_POINT ( 'NONE',  ( -20.98580030992770418, -20.83533690608478040, 65.88453944791919525 ) ) ;
#25276 = ORIENTED_EDGE ( 'NONE', *, *, #24890, .F. ) ;
#25277 = CARTESIAN_POINT ( 'NONE',  ( -19.37638992839121954, -7.619477365241829503, 60.00447059577386710 ) ) ;
#25278 = CARTESIAN_POINT ( 'NONE',  ( -11.77169535943213496, -10.59578862612641714, 74.73885051658085388 ) ) ;
#25279 = FACE_OUTER_BOUND ( 'NONE', #18303, .T. ) ;
#25280 = ORIENTED_EDGE ( 'NONE', *, *, #44068, .T. ) ;
#25281 = FACE_OUTER_BOUND ( 'NONE', #41099, .T. ) ;
#25283 = AXIS2_PLACEMENT_3D ( 'NONE', #13309, #16770, #24433 ) ;
#25282 = DIRECTION ( 'NONE',  ( -3.071710424422018668E-17, 6.404604876783312462E-16, 1.000000000000000000 ) ) ;
#25285 =( BOUNDED_CURVE ( )  B_SPLINE_CURVE ( 3, ( #40638, #6916, #32767, #37172 ),
 .UNSPECIFIED., .F., .F. ) 
 B_SPLINE_CURVE_WITH_KNOTS ( ( 4, 4 ),
 ( 0.4074455897393695625, 0.5000000000000000000 ),
 .UNSPECIFIED. ) 
 CURVE ( )  GEOMETRIC_REPRESENTATION_ITEM ( )  RATIONAL_B_SPLINE_CURVE ( ( 0.6983129098261007250, 0.7760317562606826591, 0.8765941196519758671, 0.9999999999999646949 ) ) 
 REPRESENTATION_ITEM ( '' )  );
#25284 = CARTESIAN_POINT ( 'NONE',  ( -24.26435699358934883, -17.76123410301217120, 62.51715077956382771 ) ) ;
#25286 = ORIENTED_EDGE ( 'NONE', *, *, #23033, .T. ) ;
#25287 = CARTESIAN_POINT ( 'NONE',  ( -13.49409790474204840, -20.66256726344224504, 61.53118467422925164 ) ) ;
#25288 = VERTEX_POINT ( 'NONE', #43645 ) ;
#25289 = CARTESIAN_POINT ( 'NONE',  ( -13.24261801534493088, -8.643248549050911222, 60.55454889300790455 ) ) ;
#25290 = CARTESIAN_POINT ( 'NONE',  ( -13.59065431704403615, -21.19813492939682220, 68.64280514999626348 ) ) ;
#25291 = CARTESIAN_POINT ( 'NONE',  ( -13.38575581802539993, -9.030060914960570173, 60.72478133471773987 ) ) ;
#25292 = EDGE_CURVE ( 'NONE', #17265, #18661, #2265, .T. ) ;
#25293 = CARTESIAN_POINT ( 'NONE',  ( -21.23898061349145650, -21.20841973409718406, 65.77728081245959402 ) ) ;
#25294 = VERTEX_POINT ( 'NONE', #20508 ) ;
#25295 = DIRECTION ( 'NONE',  ( -6.446466763177039895E-06, 1.047023821809670710E-05, 0.9999999999244085780 ) ) ;
#25296 = AXIS2_PLACEMENT_3D ( 'NONE', #46095, #46593, #16993 ) ;
#25297 = EDGE_CURVE ( 'NONE', #11365, #7957, #24791, .T. ) ;
#25298 = CARTESIAN_POINT ( 'NONE',  ( -23.91632973644556159, -12.05317525496800357, 59.89724340139424896 ) ) ;
#25299 = CARTESIAN_POINT ( 'NONE',  ( -21.57822623285374419, -8.624884721674641597, 73.70105113553994158 ) ) ;
#25300 = ORIENTED_EDGE ( 'NONE', *, *, #27547, .F. ) ;
#25301 = CARTESIAN_POINT ( 'NONE',  ( -10.16748990304072464, -13.12235252378331651, 71.39323974795351546 ) ) ;
#25302 = EDGE_CURVE ( 'NONE', #17349, #44188, #19551, .T. ) ;
#25303 = CARTESIAN_POINT ( 'NONE',  ( -12.41791333049023116, -9.841008508234809327, 60.97406688302051947 ) ) ;
#25305 = VERTEX_POINT ( 'NONE', #9427 ) ;
#25304 = AXIS2_PLACEMENT_3D ( 'NONE', #40898, #35, #11113 ) ;
#25306 = ORIENTED_EDGE ( 'NONE', *, *, #14715, .T. ) ;
#25307 = LINE ( 'NONE', #18616, #47825 ) ;
#25308 = LINE ( 'NONE', #40319, #17840 ) ;
#25309 = CYLINDRICAL_SURFACE ( 'NONE', #3846, 0.1499999999999964695 ) ;
#25310 = EDGE_CURVE ( 'NONE', #27657, #3647, #32067, .T. ) ;
#25311 = CARTESIAN_POINT ( 'NONE',  ( -14.84266645611046442, -8.302458146920823623, 60.31996277900389458 ) ) ;
#25312 = DIRECTION ( 'NONE',  ( 1.927470528863119542E-16, 0.000000000000000000, -1.000000000000000000 ) ) ;
#25313 = CARTESIAN_POINT ( 'NONE',  ( -13.10534385759798681, -7.595227055684746986, 51.75156210489594599 ) ) ;
#25314 = ORIENTED_EDGE ( 'NONE', *, *, #3673, .T. ) ;
#25315 = ORIENTED_EDGE ( 'NONE', *, *, #46649, .F. ) ;
#25316 = CARTESIAN_POINT ( 'NONE',  ( -17.77658133828675702, -19.49442885748621990, 49.52966884056656482 ) ) ;
#25317 = VECTOR ( 'NONE', #21132, 1000.000000000000000 ) ;
#25318 = CARTESIAN_POINT ( 'NONE',  ( -19.55442184481404766, -21.52995072282663358, 65.47958309245051112 ) ) ;
#25319 = LINE ( 'NONE', #18629, #13426 ) ;
#25320 = DIRECTION ( 'NONE',  ( -5.329554271033179131E-07, -1.313503372282854535E-06, -0.9999999999989953592 ) ) ;
#25321 = CARTESIAN_POINT ( 'NONE',  ( -17.42409385541300892, -14.80920654474439502, 75.49999999999994316 ) ) ;
#25322 = CARTESIAN_POINT ( 'NONE',  ( -18.53034385650551386, -9.794322478646142471, 51.19202720610083901 ) ) ;
#25323 = ORIENTED_EDGE ( 'NONE', *, *, #48078, .F. ) ;
#25324 = CARTESIAN_POINT ( 'NONE',  ( -21.95894689775886377, -20.14334376385412284, 62.30609413755689019 ) ) ;
#25325 = CARTESIAN_POINT ( 'NONE',  ( -10.81230840161673967, -17.25685697075765646, 64.64211442681141762 ) ) ;
#25326 = CARTESIAN_POINT ( 'NONE',  ( -14.59672178607931414, -8.347720424474937673, 60.20507679337548979 ) ) ;
#25327 = CARTESIAN_POINT ( 'NONE',  ( -10.09291371782238045, -16.13494220690481384, 68.16263107114907882 ) ) ;
#25328 = EDGE_CURVE ( 'NONE', #7640, #31648, #34721, .T. ) ;
#25329 = ORIENTED_EDGE ( 'NONE', *, *, #20014, .T. ) ;
#25330 = CARTESIAN_POINT ( 'NONE',  ( -10.59800981977604195, -16.35987635455024503, 71.63853451875513656 ) ) ;
#25331 = DIRECTION ( 'NONE',  ( 1.000000000000000000, -0.000000000000000000, -2.406186529621654511E-16 ) ) ;
#25332 = CARTESIAN_POINT ( 'NONE',  ( -17.37357235347134932, -7.759347209999027051, 67.32039595933659371 ) ) ;
#25333 = CYLINDRICAL_SURFACE ( 'NONE', #7092, 0.1499999999999964695 ) ;
#25334 = ORIENTED_EDGE ( 'NONE', *, *, #25987, .F. ) ;
#25336 = EDGE_CURVE ( 'NONE', #36571, #18999, #35512, .T. ) ;
#25335 = B_SPLINE_CURVE_WITH_KNOTS ( 'NONE', 3,
 ( #3343, #29448, #36809, #14884, #10983, #37802, #22305, #3583, #6797, #30198 ),
 .UNSPECIFIED., .F., .F.,
 ( 4, 2, 2, 2, 4 ),
 ( 0.1272669073658610484, 0.2522669073463410516, 0.3772669073268209994, 0.5022669073073009471, 0.6272669072877810059 ),
 .UNSPECIFIED. ) ;
#25337 = ORIENTED_EDGE ( 'NONE', *, *, #24897, .F. ) ;
#25338 = CARTESIAN_POINT ( 'NONE',  ( -23.84039510144717511, -11.88788025021025874, 59.48235730685867395 ) ) ;
#25339 = CARTESIAN_POINT ( 'NONE',  ( -17.64628924239291763, -7.362394388585356886, 63.67340115340124385 ) ) ;
#25340 = B_SPLINE_CURVE_WITH_KNOTS ( 'NONE', 3,
 ( #25144, #21455, #3209, #17966, #14264, #6666, #32756, #47552, #36668, #13784 ),
 .UNSPECIFIED., .F., .F.,
 ( 4, 2, 2, 2, 4 ),
 ( 0.000000000000000000, 0.2500000000000000000, 0.5000000000000000000, 0.7500000000000000000, 1.000000000000000000 ),
 .UNSPECIFIED. ) ;
#25341 = VERTEX_POINT ( 'NONE', #43154 ) ;
#25342 = CARTESIAN_POINT ( 'NONE',  ( -18.35341103611197866, -21.74886582742231766, 72.39584113235251550 ) ) ;
#25343 = CARTESIAN_POINT ( 'NONE',  ( -12.50897416063251733, -20.40789074996439112, 72.06299591474957822 ) ) ;
#25344 = EDGE_CURVE ( 'NONE', #46725, #32734, #2023, .T. ) ;
#25345 = VERTEX_POINT ( 'NONE', #9674 ) ;
#25346 = DIRECTION ( 'NONE',  ( -1.000000000000000000, 0.000000000000000000, 0.000000000000000000 ) ) ;
#25347 = CARTESIAN_POINT ( 'NONE',  ( -24.86207103330155377, -14.38397445572853961, 66.30479991853488286 ) ) ;
#25348 = ORIENTED_EDGE ( 'NONE', *, *, #1987, .F. ) ;
#25349 = CARTESIAN_POINT ( 'NONE',  ( -10.95917937052863422, -17.62195967018737619, 71.58190244267143498 ) ) ;
#25350 = CARTESIAN_POINT ( 'NONE',  ( -10.95360866178292625, -18.50214713473828709, 57.96861125158908834 ) ) ;
#25351 = EDGE_CURVE ( 'NONE', #5623, #18657, #16494, .T. ) ;
#25352 = LINE ( 'NONE', #47283, #36131 ) ;
#25353 = CARTESIAN_POINT ( 'NONE',  ( -50.42609385541305755, -14.80920654474428666, 74.09999999999998010 ) ) ;
#25354 = ORIENTED_EDGE ( 'NONE', *, *, #7163, .F. ) ;
#25355 = ORIENTED_EDGE ( 'NONE', *, *, #38895, .T. ) ;
#25356 = CARTESIAN_POINT ( 'NONE',  ( -23.36875552208945095, -10.31881635475721737, 59.80214635332909978 ) ) ;
#25357 = DIRECTION ( 'NONE',  ( -0.9000732436326449593, -0.4357386327795698122, 2.072980810273451456E-08 ) ) ;
#25358 = ORIENTED_EDGE ( 'NONE', *, *, #12075, .F. ) ;
#25359 = FACE_OUTER_BOUND ( 'NONE', #7121, .T. ) ;
#25360 = B_SPLINE_CURVE_WITH_KNOTS ( 'NONE', 3,
 ( #5836, #27749, #42780, #16889, #1650, #40048, #21092, #47197, #31929, #6065 ),
 .UNSPECIFIED., .F., .F.,
 ( 4, 2, 2, 2, 4 ),
 ( 0.6272669072877643526, 0.7522669073072746349, 0.8772669073267849171, 1.002266907346295088, 1.127266907365805482 ),
 .UNSPECIFIED. ) ;
#25361 =( BOUNDED_CURVE ( )  B_SPLINE_CURVE ( 3, ( #11052, #33421, #15206, #30017 ),
 .UNSPECIFIED., .F., .F. ) 
 B_SPLINE_CURVE_WITH_KNOTS ( ( 4, 4 ),
 ( 0.000000000000000000, 0.4074455897393629566 ),
 .UNSPECIFIED. ) 
 CURVE ( )  GEOMETRIC_REPRESENTATION_ITEM ( )  RATIONAL_B_SPLINE_CURVE ( ( 1.000000000000000000, 0.4567392136813351877, 0.3561768502900315436, 0.6983129098260889567 ) ) 
 REPRESENTATION_ITEM ( '' )  );
#25362 = EDGE_CURVE ( 'NONE', #42067, #43505, #1113, .T. ) ;
#25363 = CARTESIAN_POINT ( 'NONE',  ( -16.76159385759799036, -7.228003583438117552, 51.38655588711986155 ) ) ;
#25364 = CARTESIAN_POINT ( 'NONE',  ( -24.05813527555462628, -11.41757595432783745, 63.06562998582658253 ) ) ;
#25365 = CARTESIAN_POINT ( 'NONE',  ( -12.84817825325788299, -8.930034686467767102, 67.42296837860310177 ) ) ;
#25366 = CARTESIAN_POINT ( 'NONE',  ( -23.70794718243703514, -18.81148055198525171, 69.45405303023558474 ) ) ;
#25367 = DIRECTION ( 'NONE',  ( 0.000000000000000000, 0.9999954153791273948, 0.003028072113822398263 ) ) ;
#25368 = ORIENTED_EDGE ( 'NONE', *, *, #22323, .T. ) ;
#25369 = CARTESIAN_POINT ( 'NONE',  ( -10.56265156832558105, -13.42272637098185939, 74.97817617512852451 ) ) ;
#25370 = CARTESIAN_POINT ( 'NONE',  ( -14.10113443798904065, -8.141252799482343150, 70.98603544959661349 ) ) ;
#25371 = CARTESIAN_POINT ( 'NONE',  ( -24.87417961795293664, -14.80849281899037884, 59.42795564617806292 ) ) ;
#25372 = CARTESIAN_POINT ( 'NONE',  ( -16.58958238669307406, -22.21248813724601234, 65.36417849732876562 ) ) ;
#25373 = ADVANCED_FACE ( 'NONE', ( #14284 ), #15021, .T. ) ;
#25374 = EDGE_CURVE ( 'NONE', #48128, #36043, #40100, .T. ) ;
#25375 = ORIENTED_EDGE ( 'NONE', *, *, #32338, .T. ) ;
#25376 = ORIENTED_EDGE ( 'NONE', *, *, #15675, .T. ) ;
#25377 = EDGE_CURVE ( 'NONE', #48505, #4743, #10624, .T. ) ;
#25378 = CYLINDRICAL_SURFACE ( 'NONE', #39838, 4.686499999999997002 ) ;
#25379 = CARTESIAN_POINT ( 'NONE',  ( -23.70135487130767515, -11.71146637837649074, 63.25218278684473461 ) ) ;
#25380 = CARTESIAN_POINT ( 'NONE',  ( -45.92409385541306222, -13.51240245935757578, 70.50000000000000000 ) ) ;
#25381 = DIRECTION ( 'NONE',  ( -0.9999889394985580493, -0.004703284017506803583, 7.734398264755894983E-09 ) ) ;
#25382 = VERTEX_POINT ( 'NONE', #3230 ) ;
#25383 = CARTESIAN_POINT ( 'NONE',  ( -24.46986505407297585, -14.47671061003208415, 69.74455334859420930 ) ) ;
#25384 = CARTESIAN_POINT ( 'NONE',  ( -13.68510254299556905, -20.79040957969665371, 68.75625391717530022 ) ) ;
#25385 = ORIENTED_EDGE ( 'NONE', *, *, #48261, .F. ) ;
#25386 = CARTESIAN_POINT ( 'NONE',  ( -22.43638724005049667, -20.32197157274265820, 62.34783858214098728 ) ) ;
#25387 = CARTESIAN_POINT ( 'NONE',  ( -24.87126894608573124, -14.60124070896847392, 62.75650584303257062 ) ) ;
#25388 = CARTESIAN_POINT ( 'NONE',  ( -15.74023824147349337, -8.014750687795812567, 67.33110349041905351 ) ) ;
#25389 = B_SPLINE_CURVE_WITH_KNOTS ( 'NONE', 3,
 ( #9563, #20393, #5857, #43291, #24584, #38615, #9076, #8587, #23855, #23612 ),
 .UNSPECIFIED., .F., .F.,
 ( 4, 2, 2, 2, 4 ),
 ( 0.6272669072782746102, 0.7522669073001777562, 0.8772669073220807912, 1.002266907343983826, 1.127266907365886972 ),
 .UNSPECIFIED. ) ;
#25390 = EDGE_LOOP ( 'NONE', ( #2904, #11569, #5949, #1680 ) ) ;
#25391 = VERTEX_POINT ( 'NONE', #3721 ) ;
#25392 = CARTESIAN_POINT ( 'NONE',  ( -21.34628024798174550, -12.22231469401973847, 49.52966884056655772 ) ) ;
#25393 = CARTESIAN_POINT ( 'NONE',  ( -18.44909385759799036, -8.112991634885936776, 51.74999426922421719 ) ) ;
#25394 = CARTESIAN_POINT ( 'NONE',  ( -11.53247046633659600, -18.68106308600668797, 64.74707076449911369 ) ) ;
#25395 = EDGE_LOOP ( 'NONE', ( #32015, #10720 ) ) ;
#25396 = CARTESIAN_POINT ( 'NONE',  ( -13.90804716676048258, -20.86209139562971160, 68.45625137333186672 ) ) ;
#25397 = CARTESIAN_POINT ( 'NONE',  ( -24.08517543038346531, -12.49907855475201579, 73.52753481283211556 ) ) ;
#25398 = VECTOR ( 'NONE', #24732, 1000.000000000000227 ) ;
#25399 = CARTESIAN_POINT ( 'NONE',  ( -12.25434508901797770, -20.17367074759813406, 65.05170324716399932 ) ) ;
#25400 =( BOUNDED_CURVE ( )  B_SPLINE_CURVE ( 3, ( #39044, #9263, #17108, #35592 ),
 .UNSPECIFIED., .F., .F. ) 
 B_SPLINE_CURVE_WITH_KNOTS ( ( 4, 4 ),
 ( 0.9074455897393715054, 1.000000000000000000 ),
 .UNSPECIFIED. ) 
 CURVE ( )  GEOMETRIC_REPRESENTATION_ITEM ( )  RATIONAL_B_SPLINE_CURVE ( ( 0.6983129098260993928, 0.7760317562607036423, 0.8765941196520038448, 1.000000000000000000 ) ) 
 REPRESENTATION_ITEM ( '' )  );
#25401 = CARTESIAN_POINT ( 'NONE',  ( -10.05973382411576189, -15.93640770713343535, 64.68488457034484895 ) ) ;
#25402 = CARTESIAN_POINT ( 'NONE',  ( -19.37484620200115160, -7.619050568204919216, 60.14588398245204814 ) ) ;
#25403 = CARTESIAN_POINT ( 'NONE',  ( -24.23177493074759425, -12.96287917719623017, 69.86423168924338256 ) ) ;
#25404 = VERTEX_POINT ( 'NONE', #2739 ) ;
#25405 = CYLINDRICAL_SURFACE ( 'NONE', #9772, 0.1500000000000031863 ) ;
#25406 = CARTESIAN_POINT ( 'NONE',  ( -10.76763551407085373, -17.13171859787639661, 61.45743118825841123 ) ) ;
#25407 = DIRECTION ( 'NONE',  ( 0.9687793358424819923, -0.2479245821708678243, 0.000000000000000000 ) ) ;
#25408 = DIRECTION ( 'NONE',  ( -3.413470714839332458E-33, 1.190614954331866791E-16, -1.000000000000000000 ) ) ;
#25409 = ADVANCED_FACE ( 'NONE', ( #33483 ), #22196, .T. ) ;
#25410 = CARTESIAN_POINT ( 'NONE',  ( -9.908656216309283948, -19.57032361137281384, 53.49999999999995026 ) ) ;
#25411 = CARTESIAN_POINT ( 'NONE',  ( -13.24284385650551599, -8.811426318492348031, 52.18089403414752070 ) ) ;
#25412 = ORIENTED_EDGE ( 'NONE', *, *, #13516, .F. ) ;
#25413 = ORIENTED_EDGE ( 'NONE', *, *, #20460, .T. ) ;
#25414 = CARTESIAN_POINT ( 'NONE',  ( -11.10386593012501244, -18.75361831986885974, 61.32064883311096537 ) ) ;
#25415 = CARTESIAN_POINT ( 'NONE',  ( -20.88270815654435353, -21.40782497263450068, 58.82970582236164603 ) ) ;
#25416 = EDGE_LOOP ( 'NONE', ( #35894, #29991, #47817, #6516, #37492 ) ) ;
#25418 = CARTESIAN_POINT ( 'NONE',  ( -20.52359238471669300, -8.472965537638735611, 59.84125077296574347 ) ) ;
#25417 = CARTESIAN_POINT ( 'NONE',  ( -23.62594491300536959, -11.45603751788689095, 66.70742424642772050 ) ) ;
#25419 = DIRECTION ( 'NONE',  ( -0.000000000000000000, -1.000000000000000000, 0.000000000000000000 ) ) ;
#25420 = CARTESIAN_POINT ( 'NONE',  ( -23.03538909537400770, -9.907469116741831172, 70.19833813022523827 ) ) ;
#25421 = CARTESIAN_POINT ( 'NONE',  ( -22.22371030936713510, -9.111184089457765367, 59.90666523727240644 ) ) ;
#25422 = CARTESIAN_POINT ( 'NONE',  ( -33.52409385541305653, -2.423472813913224222, 52.29999999999998295 ) ) ;
#25423 = CARTESIAN_POINT ( 'NONE',  ( -24.35389707626741185, -16.10709931453381216, 62.87856533165624029 ) ) ;
#25424 = CARTESIAN_POINT ( 'NONE',  ( -24.82675434745867449, -13.96959720065245136, 73.24458743042187336 ) ) ;
#25425 =( BOUNDED_CURVE ( )  B_SPLINE_CURVE ( 3, ( #29329, #21698, #17981, #48517 ),
 .UNSPECIFIED., .F., .F. ) 
 B_SPLINE_CURVE_WITH_KNOTS ( ( 4, 4 ),
 ( 0.000000000000000000, 0.4074455897393655657 ),
 .UNSPECIFIED. ) 
 CURVE ( )  GEOMETRIC_REPRESENTATION_ITEM ( )  RATIONAL_B_SPLINE_CURVE ( ( 1.000000000000000000, 0.4567392136813248626, 0.3561768502900276578, 0.6983129098261082746 ) ) 
 REPRESENTATION_ITEM ( '' )  );
#25426 = CARTESIAN_POINT ( 'NONE',  ( -10.42278039055306849, -14.74509148815288739, 74.98706025067703251 ) ) ;
#25427 = CARTESIAN_POINT ( 'NONE',  ( -14.87282237418130215, -7.809539361298669213, 57.02812736438108487 ) ) ;
#25428 = EDGE_LOOP ( 'NONE', ( #41354, #44181, #37961, #28717 ) ) ;
#25429 = FACE_BOUND ( 'NONE', #23218, .T. ) ;
#25430 = CARTESIAN_POINT ( 'NONE',  ( -10.56016083362581703, -13.18709213229180932, 67.62343541709479666 ) ) ;
#25431 = CARTESIAN_POINT ( 'NONE',  ( -20.92409385759799179, -9.359200813967568422, 50.49621490985803263 ) ) ;
#25432 = CARTESIAN_POINT ( 'NONE',  ( -24.61605428079846547, -12.86511719609775284, 66.41751453275240635 ) ) ;
#25433 = CARTESIAN_POINT ( 'NONE',  ( -13.86779599075735092, -20.83853035579127067, 65.09514786855950774 ) ) ;
#25434 = CARTESIAN_POINT ( 'NONE',  ( -11.50273595086851763, -11.07590776185467263, 57.20903212540526539 ) ) ;
#25435 = B_SPLINE_CURVE_WITH_KNOTS ( 'NONE', 3,
 ( #20303, #42949, #20059, #27690, #1326, #28179, #5779, #46887, #31382, #8751 ),
 .UNSPECIFIED., .F., .F.,
 ( 4, 2, 2, 2, 4 ),
 ( 0.1272669073658437844, 0.2522669073488139624, 0.3772669073317841959, 0.5022669073147544294, 0.6272669072977246074 ),
 .UNSPECIFIED. ) ;
#25437 = ORIENTED_EDGE ( 'NONE', *, *, #5945, .F. ) ;
#25436 = ADVANCED_FACE ( 'NONE', ( #18478 ), #29832, .T. ) ;
#25438 = ORIENTED_EDGE ( 'NONE', *, *, #22472, .T. ) ;
#25439 = CARTESIAN_POINT ( 'NONE',  ( -18.92409385541304090, -9.359200813967568422, 50.49621490985803263 ) ) ;
#25440 = ORIENTED_EDGE ( 'NONE', *, *, #43620, .T. ) ;
#25441 = EDGE_CURVE ( 'NONE', #25847, #20972, #20361, .T. ) ;
#25442 = EDGE_CURVE ( 'NONE', #19604, #23975, #21551, .T. ) ;
#25443 = CARTESIAN_POINT ( 'NONE',  ( -15.80316865820435446, -9.815700611529285524, 52.02966884056656482 ) ) ;
#25444 = CIRCLE ( 'NONE', #38825, 5.000000000000000000 ) ;
#25445 = DIRECTION ( 'NONE',  ( -1.404489950266683237E-08, 6.428047446179355909E-07, 0.9999999999997932765 ) ) ;
#25446 = CARTESIAN_POINT ( 'NONE',  ( -21.57946453887431204, -8.565578233975859490, 47.99999999999994316 ) ) ;
#25447 = CARTESIAN_POINT ( 'NONE',  ( -16.59344411340201475, -21.75974756046277747, 65.22564390621562325 ) ) ;
#25448 = VERTEX_POINT ( 'NONE', #26135 ) ;
#25449 = CARTESIAN_POINT ( 'NONE',  ( -17.42409385541306222, -14.80920654474411080, 75.49999999999998579 ) ) ;
#25450 = ORIENTED_EDGE ( 'NONE', *, *, #19034, .F. ) ;
#25451 = DIRECTION ( 'NONE',  ( 0.7971031148784507581, -0.6038432116460916710, 6.916509187980650173E-08 ) ) ;
#25452 = FACE_OUTER_BOUND ( 'NONE', #4297, .T. ) ;
#25453 = ORIENTED_EDGE ( 'NONE', *, *, #38434, .F. ) ;
#25454 = CARTESIAN_POINT ( 'NONE',  ( -23.16117746674104438, -18.90708040007733359, 62.63934749780565880 ) ) ;
#25455 = CARTESIAN_POINT ( 'NONE',  ( -21.42200791050363051, -21.09572771556245740, 69.09804232902482113 ) ) ;
#25456 = LINE ( 'NONE', #40958, #2179 ) ;
#25457 = EDGE_LOOP ( 'NONE', ( #42214, #7429, #20488, #25348, #47647 ) ) ;
#25458 = DIRECTION ( 'NONE',  ( -2.866981220435666553E-17, 1.000000000000000000, 1.190614954331866791E-16 ) ) ;
#25459 = ADVANCED_FACE ( 'NONE', ( #18235 ), #41147, .F. ) ;
#25460 = CARTESIAN_POINT ( 'NONE',  ( -23.95986381193147707, -17.46034710541827906, 69.82828398331871256 ) ) ;
#25461 = DIRECTION ( 'NONE',  ( 0.8949343913984054710, -0.4461977533475101065, -3.119193279067933041E-16 ) ) ;
#25462 = DIRECTION ( 'NONE',  ( 1.006957036571142899E-05, -6.253991264129192257E-06, -0.9999999999297457531 ) ) ;
#25463 = VERTEX_POINT ( 'NONE', #36460 ) ;
#25464 = CARTESIAN_POINT ( 'NONE',  ( -18.92409385541305511, -14.80920654474410547, 47.99999999999998579 ) ) ;
#25465 = CARTESIAN_POINT ( 'NONE',  ( -10.73211873618052969, -12.75535506112652584, 60.87141649276334476 ) ) ;
#25466 = CARTESIAN_POINT ( 'NONE',  ( -23.69928304873747038, -18.82488403301566038, 69.33726028187463442 ) ) ;
#25467 = CARTESIAN_POINT ( 'NONE',  ( -11.97212546196701943, -10.32690635925306211, 74.58318462221375000 ) ) ;
#25468 = CIRCLE ( 'NONE', #4254, 1.999999999999999334 ) ;
#25469 = CARTESIAN_POINT ( 'NONE',  ( -16.84865286310842336, -21.83598151670433296, 68.98088545748413480 ) ) ;
#25470 = CARTESIAN_POINT ( 'NONE',  ( -14.91432061146141663, -8.212540298998538546, 63.93411529719415398 ) ) ;
#25471 = ORIENTED_EDGE ( 'NONE', *, *, #44476, .T. ) ;
#25472 = CARTESIAN_POINT ( 'NONE',  ( -24.35040279276217845, -17.55351991699908609, 66.10390635504940349 ) ) ;
#25473 = DIRECTION ( 'NONE',  ( -0.1240347345892086200, 1.145860353393066553E-16, -0.9922778767136676281 ) ) ;
#25474 = CARTESIAN_POINT ( 'NONE',  ( -11.89178903705324863, -10.43929771899554915, 71.26893105542536944 ) ) ;
#25475 = EDGE_LOOP ( 'NONE', ( #29844, #38919, #34928, #46069 ) ) ;
#25476 = ORIENTED_EDGE ( 'NONE', *, *, #27331, .T. ) ;
#25477 = VERTEX_POINT ( 'NONE', #29575 ) ;
#25478 = ORIENTED_EDGE ( 'NONE', *, *, #24078, .F. ) ;
#25479 = CARTESIAN_POINT ( 'NONE',  ( -11.52915434062558120, -10.92788463621912420, 60.82318916367986361 ) ) ;
#25480 = DIRECTION ( 'NONE',  ( 3.071710424422018668E-17, -6.404604876783312462E-16, -1.000000000000000000 ) ) ;
#25481 = CARTESIAN_POINT ( 'NONE',  ( -12.81450749931373245, -9.474957484202729319, 74.31923006089486705 ) ) ;
#25482 = ORIENTED_EDGE ( 'NONE', *, *, #46776, .F. ) ;
#25483 = EDGE_LOOP ( 'NONE', ( #48553, #30093, #47906, #36997, #7804 ) ) ;
#25484 = CARTESIAN_POINT ( 'NONE',  ( -16.93034385650552309, -9.794322478646142471, 51.19202720610083901 ) ) ;
#25485 = EDGE_CURVE ( 'NONE', #42753, #48265, #6556, .T. ) ;
#25486 = DIRECTION ( 'NONE',  ( -3.071710424422018668E-17, 6.404604876783312462E-16, 1.000000000000000000 ) ) ;
#25487 = DIRECTION ( 'NONE',  ( 1.000000000000000000, -4.164305804376849172E-17, 1.614929280266638808E-16 ) ) ;
#25488 = CARTESIAN_POINT ( 'NONE',  ( -19.01159385650551670, -6.922745924619793101, 51.69366785382590024 ) ) ;
#25489 = AXIS2_PLACEMENT_3D ( 'NONE', #29172, #25715, #36766 ) ;
#25490 = ADVANCED_FACE ( 'NONE', ( #48282 ), #33740, .T. ) ;
#25492 = ORIENTED_EDGE ( 'NONE', *, *, #41754, .T. ) ;
#25491 = ADVANCED_FACE ( 'NONE', ( #17745 ), #44143, .T. ) ;
#25493 = FACE_OUTER_BOUND ( 'NONE', #4923, .T. ) ;
#25494 = AXIS2_PLACEMENT_3D ( 'NONE', #22147, #47520, #37129 ) ;
#25495 = EDGE_CURVE ( 'NONE', #40380, #48456, #48046, .T. ) ;
#25496 = CARTESIAN_POINT ( 'NONE',  ( -14.48548941065489970, -8.400516866317895293, 67.27447142263336843 ) ) ;
#25497 = EDGE_CURVE ( 'NONE', #12297, #10202, #23141, .T. ) ;
#25498 = CARTESIAN_POINT ( 'NONE',  ( -24.40217300928714650, -14.25566238011515274, 69.65275273531472067 ) ) ;
#25499 = VERTEX_POINT ( 'NONE', #45341 ) ;
#25500 = CARTESIAN_POINT ( 'NONE',  ( -11.21157628577468657, -11.58358644131346082, 67.61864608155907774 ) ) ;
#25501 = ORIENTED_EDGE ( 'NONE', *, *, #12502, .T. ) ;
#25502 = CARTESIAN_POINT ( 'NONE',  ( -19.59909385541296345, -8.105421454601382081, 49.25000573077626598 ) ) ;
#25503 = CARTESIAN_POINT ( 'NONE',  ( -19.45790264050342699, -21.50891717485947652, 65.57559305958521634 ) ) ;
#25504 = CARTESIAN_POINT ( 'NONE',  ( -10.50893933415051507, -13.43540278197274063, 74.96345540680638919 ) ) ;
#25505 = CARTESIAN_POINT ( 'NONE',  ( -10.39868982912479645, -12.32967425775121306, 57.50574246823239122 ) ) ;
#25506 = EDGE_CURVE ( 'NONE', #46725, #28374, #39236, .T. ) ;
#25507 = EDGE_LOOP ( 'NONE', ( #27991, #13519 ) ) ;
#25508 = LINE ( 'NONE', #14630, #6125 ) ;
#25509 = DIRECTION ( 'NONE',  ( -3.071710424422018668E-17, 6.404604876783312462E-16, 1.000000000000000000 ) ) ;
#25510 = DIRECTION ( 'NONE',  ( -0.09332174201254901658, -0.9956360040033422898, 0.000000000000000000 ) ) ;
#25511 = ORIENTED_EDGE ( 'NONE', *, *, #29794, .F. ) ;
#25512 = DIRECTION ( 'NONE',  ( 1.927470528863184130E-16, 1.434740771370715221E-29, -1.000000000000000000 ) ) ;
#25513 = DIRECTION ( 'NONE',  ( 0.9180681052388952601, -0.3964226963016432292, 0.000000000000000000 ) ) ;
#25514 = CARTESIAN_POINT ( 'NONE',  ( -18.76715758977493209, -7.481188742717107765, 70.41422074109146934 ) ) ;
#25515 = EDGE_LOOP ( 'NONE', ( #33715, #2129, #29521, #5316 ) ) ;
#25516 = CARTESIAN_POINT ( 'NONE',  ( -11.73209289625006058, -10.73465601455801099, 74.51172899894849877 ) ) ;
#25517 = VERTEX_POINT ( 'NONE', #3974 ) ;
#25518 = CARTESIAN_POINT ( 'NONE',  ( -10.33483191699034265, -17.09962811228164270, 57.73114616685904110 ) ) ;
#25519 = CARTESIAN_POINT ( 'NONE',  ( -24.66548415425539531, -13.05833320866972613, 62.93990042163805043 ) ) ;
#25520 = LINE ( 'NONE', #29461, #12421 ) ;
#25521 = CARTESIAN_POINT ( 'NONE',  ( -23.41616298382994898, -18.52428493080399008, 72.77840375779385340 ) ) ;
#25522 = ORIENTED_EDGE ( 'NONE', *, *, #47592, .F. ) ;
#25523 = LINE ( 'NONE', #28975, #18155 ) ;
#25524 = CARTESIAN_POINT ( 'NONE',  ( -42.91426037125016535, -14.90920654474413709, 59.07866787330315361 ) ) ;
#25525 = DIRECTION ( 'NONE',  ( -1.224646799147353207E-16, -1.000000000000000000, 1.935130192142698731E-16 ) ) ;
#25526 = ORIENTED_EDGE ( 'NONE', *, *, #8919, .T. ) ;
#25527 = CARTESIAN_POINT ( 'NONE',  ( -14.07539681412751165, -8.605278097683305205, 74.49954655214880006 ) ) ;
#25528 = AXIS2_PLACEMENT_3D ( 'NONE', #943, #19404, #26810 ) ;
#25529 = AXIS2_PLACEMENT_3D ( 'NONE', #39029, #1117, #31655 ) ;
#25530 = ORIENTED_EDGE ( 'NONE', *, *, #22571, .T. ) ;
#25531 = VERTEX_POINT ( 'NONE', #23174 ) ;
#25532 = CARTESIAN_POINT ( 'NONE',  ( -14.92957465851463006, -21.82926012297162899, 65.22101360901100975 ) ) ;
#25533 = CARTESIAN_POINT ( 'NONE',  ( -15.34465393633500518, -21.54586957516256263, 68.86120835375241711 ) ) ;
#25534 = CARTESIAN_POINT ( 'NONE',  ( -10.13783977983156248, -13.25541127610578762, 74.79322348855123437 ) ) ;
#25535 = CARTESIAN_POINT ( 'NONE',  ( -20.36536858953947515, -8.398766899984980938, 63.19632798853695022 ) ) ;
#25536 =( BOUNDED_CURVE ( )  B_SPLINE_CURVE ( 3, ( #36476, #40662, #25418, #6943 ),
 .UNSPECIFIED., .F., .F. ) 
 B_SPLINE_CURVE_WITH_KNOTS ( ( 4, 4 ),
 ( 0.000000000000000000, 0.4074455897393672310 ),
 .UNSPECIFIED. ) 
 CURVE ( )  GEOMETRIC_REPRESENTATION_ITEM ( )  RATIONAL_B_SPLINE_CURVE ( ( 1.000000000000000000, 0.4567392136813244186, 0.3561768502900274913, 0.6983129098261091627 ) ) 
 REPRESENTATION_ITEM ( '' )  );
#25537 = ADVANCED_FACE ( 'NONE', ( #19958 ), #4448, .T. ) ;
#25538 = CARTESIAN_POINT ( 'NONE',  ( -14.87886284476815923, -8.287862385134991072, 60.60379677410870869 ) ) ;
#25539 = CARTESIAN_POINT ( 'NONE',  ( -12.19808601445598306, -20.11893053951551735, 65.04487616575880793 ) ) ;
#25540 = CARTESIAN_POINT ( 'NONE',  ( -13.16159385759798894, -7.228003583438117552, 51.38655588711986155 ) ) ;
#25541 = ORIENTED_EDGE ( 'NONE', *, *, #10436, .T. ) ;
#25542 = ORIENTED_EDGE ( 'NONE', *, *, #18647, .F. ) ;
#25543 = DIRECTION ( 'NONE',  ( 1.000000000000000000, -4.164305804376849172E-17, 1.614929280266638808E-16 ) ) ;
#25544 = EDGE_CURVE ( 'NONE', #20471, #42275, #35288, .T. ) ;
#25545 = LINE ( 'NONE', #22108, #3161 ) ;
#25546 = CARTESIAN_POINT ( 'NONE',  ( -23.76319945593019156, -11.71557033483072985, 66.72214621596255313 ) ) ;
#25547 = DIRECTION ( 'NONE',  ( -1.000000000000000000, 4.164305804376849172E-17, -1.614929280266638808E-16 ) ) ;
#25548 = FACE_OUTER_BOUND ( 'NONE', #24130, .T. ) ;
#25549 = ORIENTED_EDGE ( 'NONE', *, *, #19899, .T. ) ;
#25550 = CARTESIAN_POINT ( 'NONE',  ( -20.16159385650551883, -9.295667164867525756, 49.30633214617472504 ) ) ;
#25551 =( BOUNDED_SURFACE ( )  B_SPLINE_SURFACE ( 3, 1, ( 
 ( #39833, #44039 ),
 ( #40321, #21129 ),
 ( #6591, #36127 ),
 ( #23689, #32908 ),
 ( #31298, #47952 ),
 ( #38686, #17885 ),
 ( #2410, #44276 ) ),
 .UNSPECIFIED., .T., .F., .F. ) 
 B_SPLINE_SURFACE_WITH_KNOTS ( ( 4, 3, 4 ),
 ( 2, 2 ),
 ( 0.000000000000000000, 0.5000000000000000000, 1.000000000000000000 ),
 ( 0.000000000000000000, 1.000000000000000000 ),
 .UNSPECIFIED. ) 
 GEOMETRIC_REPRESENTATION_ITEM ( )  RATIONAL_B_SPLINE_SURFACE ( (
 ( 1.000000000000000000, 1.000000000000000000),
 ( 0.3333333333333335369, 0.3333333333333330373),
 ( 0.3333333333333335369, 0.3333333333333330373),
 ( 1.000000000000000000, 1.000000000000000000),
 ( 0.3333333333333333703, 0.3333333333333333703),
 ( 0.3333333333333333703, 0.3333333333333333703),
 ( 1.000000000000000000, 1.000000000000000000) ) ) 
 REPRESENTATION_ITEM ( '' )  SURFACE ( )  );
#25552 = ORIENTED_EDGE ( 'NONE', *, *, #48209, .F. ) ;
#25553 = CARTESIAN_POINT ( 'NONE',  ( -22.02981006882838955, -20.08072627601145399, 62.53439177585065778 ) ) ;
#25554 = DIRECTION ( 'NONE',  ( -3.071710424422018668E-17, 6.404604876783312462E-16, 1.000000000000000000 ) ) ;
#25555 = EDGE_CURVE ( 'NONE', #21318, #23343, #24306, .T. ) ;
#25556 = CARTESIAN_POINT ( 'NONE',  ( -16.41515664040973022, -21.78667843868697318, 62.05568103759625842 ) ) ;
#25557 = CARTESIAN_POINT ( 'NONE',  ( -11.20449214220105816, -18.91032654392478207, 64.94695843806114510 ) ) ;
#25558 = EDGE_CURVE ( 'NONE', #46918, #18891, #46305, .T. ) ;
#25559 = ORIENTED_EDGE ( 'NONE', *, *, #5260, .F. ) ;
#25560 =( BOUNDED_CURVE ( )  B_SPLINE_CURVE ( 2, ( #6448, #10387, #2014, #17008, #25393, #36218, #2256, #28372, #43398 ),
 .UNSPECIFIED., .F., .F. ) 
 B_SPLINE_CURVE_WITH_KNOTS ( ( 3, 2, 2, 2, 3 ),
 ( 0.3749999999999998335, 0.3854166666666665741, 0.3958333333333332593, 0.4062500000000000000, 0.4166666666666667407 ),
 .UNSPECIFIED. ) 
 CURVE ( )  GEOMETRIC_REPRESENTATION_ITEM ( )  RATIONAL_B_SPLINE_CURVE ( ( 1.000000000000001110, 0.9238795325112855172, 1.000000000000000000, 0.9238795325112867385, 1.000000000000000000, 0.9238795325112867385, 1.000000000000000000, 0.9238795325112862944, 1.000000000000000444 ) ) 
 REPRESENTATION_ITEM ( '' )  );
#25561 = AXIS2_PLACEMENT_3D ( 'NONE', #15285, #23195, #38185 ) ;
#25562 = EDGE_CURVE ( 'NONE', #28462, #5991, #18069, .T. ) ;
#25563 = DIRECTION ( 'NONE',  ( 2.866981220435666553E-17, -1.000000000000000000, -1.190614954331866791E-16 ) ) ;
#25564 = CARTESIAN_POINT ( 'NONE',  ( -14.66741299049177094, -8.374868138257010486, 60.51099561025887397 ) ) ;
#25565 = CIRCLE ( 'NONE', #20863, 1.999999999999998668 ) ;
#25566 = EDGE_LOOP ( 'NONE', ( #20184, #7318 ) ) ;
#25567 = DIRECTION ( 'NONE',  ( 3.141253923644155253E-07, -8.288700512985352896E-07, 0.9999999999996072031 ) ) ;
#25568 = EDGE_CURVE ( 'NONE', #16133, #1136, #46060, .T. ) ;
#25569 = B_SPLINE_CURVE_WITH_KNOTS ( 'NONE', 1,
 ( #42642, #20705 ),
 .UNSPECIFIED., .F., .F.,
 ( 2, 2 ),
 ( 0.000000000000000000, 1.000000000000000000 ),
 .UNSPECIFIED. ) ;
#25570 = FACE_OUTER_BOUND ( 'NONE', #16037, .T. ) ;
#25571 = ORIENTED_EDGE ( 'NONE', *, *, #18188, .F. ) ;
#25572 = CARTESIAN_POINT ( 'NONE',  ( -20.85666738206293047, -20.91166016791921578, 65.69527100157196742 ) ) ;
#25573 = ORIENTED_EDGE ( 'NONE', *, *, #3687, .T. ) ;
#25574 = CARTESIAN_POINT ( 'NONE',  ( -16.56761320685650318, -19.87745396966068157, 49.52966884056656482 ) ) ;
#25575 = EDGE_LOOP ( 'NONE', ( #6421, #37793, #47829, #16421 ) ) ;
#25576 = DIRECTION ( 'NONE',  ( -6.385196548387842039E-06, 5.147825516598811523E-06, -0.9999999999663645722 ) ) ;
#25577 = DIRECTION ( 'NONE',  ( -3.141253907721240275E-07, 8.288700426223213302E-07, -0.9999999999996070921 ) ) ;
#25578 = ORIENTED_EDGE ( 'NONE', *, *, #5551, .T. ) ;
#25579 = CYLINDRICAL_SURFACE ( 'NONE', #7969, 0.1500000000000002998 ) ;
#25580 = CARTESIAN_POINT ( 'NONE',  ( -19.81157080418587313, -21.44583120317290081, 65.34997476282926243 ) ) ;
#25581 = DIRECTION ( 'NONE',  ( -0.9757441136919988711, -0.2189141945955433433, 0.000000000000000000 ) ) ;
#25582 = EDGE_LOOP ( 'NONE', ( #41476, #2946 ) ) ;
#25583 = CARTESIAN_POINT ( 'NONE',  ( -24.40217295060720204, -14.25566147773195524, 69.95275273531336779 ) ) ;
#25584 = DIRECTION ( 'NONE',  ( -1.206829990499677715E-05, -1.995688260022264671E-06, -0.9999999999251866223 ) ) ;
#25585 = CARTESIAN_POINT ( 'NONE',  ( -23.74619244455239553, -11.68933966055485030, 63.25218278636739910 ) ) ;
#25586 = VERTEX_POINT ( 'NONE', #30571 ) ;
#25587 = ORIENTED_EDGE ( 'NONE', *, *, #23526, .F. ) ;
#25588 = CARTESIAN_POINT ( 'NONE',  ( -22.84776207900630851, -9.701615188675109636, 73.73807001133110361 ) ) ;
#25589 = CARTESIAN_POINT ( 'NONE',  ( -11.93102662126159785, -10.47028825497329585, 70.96893105764984000 ) ) ;
#25590 = CARTESIAN_POINT ( 'NONE',  ( -17.65298207767979477, -7.812888375568328492, 60.30734138473366102 ) ) ;
#25591 = CARTESIAN_POINT ( 'NONE',  ( -16.25534385759799250, -8.623186033802570094, 49.24843789510467218 ) ) ;
#25592 = CARTESIAN_POINT ( 'NONE',  ( -24.12071508562369715, -11.54438765950021306, 63.06722961171875852 ) ) ;
#25593 = EDGE_CURVE ( 'NONE', #48265, #37822, #17087, .T. ) ;
#25594 = CARTESIAN_POINT ( 'NONE',  ( -16.78865379391102408, -21.78030513117466072, 68.69560651887046276 ) ) ;
#25595 = PLANE ( 'NONE',  #10345 ) ;
#25596 = VECTOR ( 'NONE', #37213, 1000.000000000000114 ) ;
#25597 = ORIENTED_EDGE ( 'NONE', *, *, #44375, .T. ) ;
#25598 = CARTESIAN_POINT ( 'NONE',  ( -20.94324281608204430, -8.242681057013424351, 60.09771182510558418 ) ) ;
#25599 =( REPRESENTATION_RELATIONSHIP ('NONE','NONE', #2768, #34550 ) REPRESENTATION_RELATIONSHIP_WITH_TRANSFORMATION ( #40004 )SHAPE_REPRESENTATION_RELATIONSHIP( ) );
#25600 = FACE_OUTER_BOUND ( 'NONE', #35379, .T. ) ;
#25601 = CARTESIAN_POINT ( 'NONE',  ( -11.57425704488359841, -18.65360627554439077, 65.04707076833931012 ) ) ;
#25602 = EDGE_LOOP ( 'NONE', ( #26088, #40371, #15563, #39154, #18222 ) ) ;
#25603 = EDGE_LOOP ( 'NONE', ( #26886, #22704, #838, #45719 ) ) ;
#25604 = CARTESIAN_POINT ( 'NONE',  ( -20.63429004897692920, -8.588635981428261346, 60.12659873706649449 ) ) ;
#25605 = CARTESIAN_POINT ( 'NONE',  ( -24.86242989439883289, -14.39095395922188558, 66.36788051138485400 ) ) ;
#25606 = EDGE_CURVE ( 'NONE', #34242, #42959, #31316, .T. ) ;
#25607 = CARTESIAN_POINT ( 'NONE',  ( -23.32859574730126084, -19.35227928776919626, 58.98387009178664186 ) ) ;
#25608 = CARTESIAN_POINT ( 'NONE',  ( -24.30978138445934533, -13.29580787541330444, 59.66267893655142984 ) ) ;
#25609 = EDGE_CURVE ( 'NONE', #16499, #40821, #38409, .T. ) ;
#25610 = VERTEX_POINT ( 'NONE', #26622 ) ;
#25611 = CARTESIAN_POINT ( 'NONE',  ( -11.54646099848356222, -18.70898497394131255, 61.27710574299381108 ) ) ;
#25612 = EDGE_CURVE ( 'NONE', #46946, #23016, #7925, .T. ) ;
#25613 = CARTESIAN_POINT ( 'NONE',  ( -10.96142808812597735, -11.10142881709785101, 64.33537400591416144 ) ) ;
#25614 = ORIENTED_EDGE ( 'NONE', *, *, #5531, .T. ) ;
#25615 = CARTESIAN_POINT ( 'NONE',  ( -13.69193161217391363, -21.25696551969686965, 68.65613906552292178 ) ) ;
#25616 = ADVANCED_FACE ( 'NONE', ( #30814 ), #6445, .T. ) ;
#25617 = CARTESIAN_POINT ( 'NONE',  ( -12.89377865171026905, -9.472814404202125615, 70.92213358633685516 ) ) ;
#25618 = CARTESIAN_POINT ( 'NONE',  ( -22.90738119516900539, -10.37220287249194683, 59.81023178929109463 ) ) ;
#25619 = ORIENTED_EDGE ( 'NONE', *, *, #22472, .F. ) ;
#25620 = LINE ( 'NONE', #13558, #7109 ) ;
#25621 = AXIS2_PLACEMENT_3D ( 'NONE', #23146, #34697, #19192 ) ;
#25622 = EDGE_LOOP ( 'NONE', ( #37113, #31920, #21122, #13296, #16021 ) ) ;
#25623 = CARTESIAN_POINT ( 'NONE',  ( -22.78151580134219500, -19.98625284378301004, 72.75905219260647527 ) ) ;
#25624 = CARTESIAN_POINT ( 'NONE',  ( -12.15466845058241674, -8.150045384784233349, 54.38277594638588397 ) ) ;
#25625 = ORIENTED_EDGE ( 'NONE', *, *, #31505, .F. ) ;
#25626 = DIRECTION ( 'NONE',  ( -0.4415479322351564262, -0.8912598635915878198, 0.1033986416233890898 ) ) ;
#25627 = CARTESIAN_POINT ( 'NONE',  ( -24.51865387586880729, -12.53305138704347144, 73.42880879726919829 ) ) ;
#25628 = CARTESIAN_POINT ( 'NONE',  ( -20.81159385650551386, -6.922745924619793101, 51.69366785382590024 ) ) ;
#25629 = CARTESIAN_POINT ( 'NONE',  ( -14.37872387272655850, -8.506304085067752041, 67.54509766762896561 ) ) ;
#25630 = EDGE_CURVE ( 'NONE', #28899, #39514, #21925, .T. ) ;
#25631 = CARTESIAN_POINT ( 'NONE',  ( -10.79541835452027776, -17.05898387227370705, 57.76048578130984623 ) ) ;
#25632 = CARTESIAN_POINT ( 'NONE',  ( -17.42409385541299471, -14.80920654474435771, 49.52966884056655772 ) ) ;
#25633 = ORIENTED_EDGE ( 'NONE', *, *, #46838, .F. ) ;
#25634 = CARTESIAN_POINT ( 'NONE',  ( -20.58080933007877533, -8.501275685423019368, 67.08104112728932478 ) ) ;
#25635 = EDGE_CURVE ( 'NONE', #15096, #27258, #20194, .T. ) ;
#25636 = CARTESIAN_POINT ( 'NONE',  ( -17.26599293058224305, -9.561587646847172550, 50.77966884056655772 ) ) ;
#25637 = CARTESIAN_POINT ( 'NONE',  ( -21.47456293661849713, -9.038556783377254433, 70.41660404402310292 ) ) ;
#25638 = CARTESIAN_POINT ( 'NONE',  ( -22.23733827145997566, -19.96043728507621040, 65.70421731380814379 ) ) ;
#25639 = CARTESIAN_POINT ( 'NONE',  ( -13.35712140185222019, -20.57241581739411984, 61.81646620894163391 ) ) ;
#25640 = EDGE_CURVE ( 'NONE', #10431, #5464, #39637, .T. ) ;
#25641 = CARTESIAN_POINT ( 'NONE',  ( -24.28473927714575353, -16.19956134247464519, 62.59328727871961462 ) ) ;
#25642 = EDGE_LOOP ( 'NONE', ( #1775, #28370, #9414, #10611 ) ) ;
#25643 = ORIENTED_EDGE ( 'NONE', *, *, #16213, .T. ) ;
#25644 = CARTESIAN_POINT ( 'NONE',  ( -24.49878988761138388, -12.47402815302071843, 73.36508674653782691 ) ) ;
#25645 = VERTEX_POINT ( 'NONE', #20926 ) ;
#25647 = CARTESIAN_POINT ( 'NONE',  ( -13.83659385650551776, -6.915538690918075382, 49.31353937987644542 ) ) ;
#25646 = CARTESIAN_POINT ( 'NONE',  ( -15.41171220965234134, -7.636089294961081464, 74.18711515319478167 ) ) ;
#25648 = EDGE_CURVE ( 'NONE', #28690, #25694, #30030, .T. ) ;
#25649 = CARTESIAN_POINT ( 'NONE',  ( -6.424093855413055110, -27.10920654474410796, 45.99999999999998579 ) ) ;
#25650 = CARTESIAN_POINT ( 'NONE',  ( -15.47038452772150841, -21.58309165278561537, 72.04575460769355288 ) ) ;
#25651 = DIRECTION ( 'NONE',  ( 2.866981220435666553E-17, -1.000000000000000000, -1.190614954331866791E-16 ) ) ;
#25652 = FACE_BOUND ( 'NONE', #17326, .T. ) ;
#25653 = CARTESIAN_POINT ( 'NONE',  ( -24.83000351354337099, -13.99979019377566125, 73.22247878125472198 ) ) ;
#25654 = CARTESIAN_POINT ( 'NONE',  ( -11.41951145912443266, -19.21922708312919426, 71.79411749213964811 ) ) ;
#25655 = CARTESIAN_POINT ( 'NONE',  ( -17.19811928533322387, -9.313850733363548073, 53.49999999999995026 ) ) ;
#25656 = ORIENTED_EDGE ( 'NONE', *, *, #44476, .F. ) ;
#25657 = CARTESIAN_POINT ( 'NONE',  ( -14.38502091232239621, -11.22596901536237013, 49.52966884056655772 ) ) ;
#25658 = DIRECTION ( 'NONE',  ( 0.000000000000000000, 0.000000000000000000, 1.000000000000000000 ) ) ;
#25659 = DIRECTION ( 'NONE',  ( -0.1240347345892086062, 1.145860353393066553E-16, -0.9922778767136676281 ) ) ;
#25660 = CARTESIAN_POINT ( 'NONE',  ( -10.37462438995674319, -14.89569194323783208, 74.79778901495059529 ) ) ;
#25661 = CARTESIAN_POINT ( 'NONE',  ( -24.21645823680271903, -12.90730551592505115, 63.04083907877015491 ) ) ;
#25662 = DIRECTION ( 'NONE',  ( 0.000000000000000000, -0.9999954153791273948, -0.003028072113819838245 ) ) ;
#25663 = B_SPLINE_CURVE_WITH_KNOTS ( 'NONE', 3,
 ( #29977, #45014, #33899, #26273, #37092, #33149, #48427, #14657, #41538, #7824 ),
 .UNSPECIFIED., .F., .F.,
 ( 4, 2, 2, 2, 4 ),
 ( 0.000000000000000000, 0.2500000000000000000, 0.5000000000000000000, 0.7500000000000000000, 1.000000000000000000 ),
 .UNSPECIFIED. ) ;
#25664 = FACE_OUTER_BOUND ( 'NONE', #11628, .T. ) ;
#25665 = ORIENTED_EDGE ( 'NONE', *, *, #6542, .T. ) ;
#25666 = VECTOR ( 'NONE', #19936, 1000.000000000000000 ) ;
#25667 = ORIENTED_EDGE ( 'NONE', *, *, #1432, .F. ) ;
#25668 = CIRCLE ( 'NONE', #5263, 0.5000000000000004441 ) ;
#25669 = CARTESIAN_POINT ( 'NONE',  ( -15.49284385541304232, -8.630756214087126565, 51.74842643355248129 ) ) ;
#25670 = ORIENTED_EDGE ( 'NONE', *, *, #9178, .F. ) ;
#25671 = B_SPLINE_CURVE_WITH_KNOTS ( 'NONE', 3,
 ( #27156, #16536, #31575, #20500, #42178, #41934, #8211, #23471, #4751, #38467 ),
 .UNSPECIFIED., .F., .F.,
 ( 4, 2, 2, 2, 4 ),
 ( 0.1272669073658183603, 0.2522669073463091882, 0.3772669073268000162, 0.5022669073072908441, 0.6272669072877816721 ),
 .UNSPECIFIED. ) ;
#25672 = CARTESIAN_POINT ( 'NONE',  ( -16.98261326800368209, -21.79527086262147861, 72.16543221550985265 ) ) ;
#25673 = CARTESIAN_POINT ( 'NONE',  ( -23.99919193691511410, -17.21124756729841465, 69.41339796233270931 ) ) ;
#25674 = ADVANCED_FACE ( 'NONE', ( #35929 ), #26878, .T. ) ;
#25675 = CARTESIAN_POINT ( 'NONE',  ( -15.72937801229072541, -7.965776692693047778, 70.61549658711864197 ) ) ;
#25676 = CARTESIAN_POINT ( 'NONE',  ( -10.37210014130659275, -14.68995570394611505, 75.21267707208666309 ) ) ;
#25677 = EDGE_LOOP ( 'NONE', ( #43271, #28103, #8214, #29323, #22635, #47074, #8428, #19949, #30130, #5319, #47090, #45331 ) ) ;
#25678 = ADVANCED_FACE ( 'NONE', ( #35681 ), #24635, .F. ) ;
#25679 = CARTESIAN_POINT ( 'NONE',  ( -23.13465042048557763, -10.02438105578966621, 66.68148899222990167 ) ) ;
#25680 = CARTESIAN_POINT ( 'NONE',  ( -12.44533934557844113, -9.817553771701762244, 57.09495291247809945 ) ) ;
#25681 = VERTEX_POINT ( 'NONE', #9850 ) ;
#25682 =( BOUNDED_CURVE ( )  B_SPLINE_CURVE ( 3, ( #4574, #34851, #34603, #27948 ),
 .UNSPECIFIED., .F., .F. ) 
 B_SPLINE_CURVE_WITH_KNOTS ( ( 4, 4 ),
 ( 0.5000000000000000000, 0.9074455897393659543 ),
 .UNSPECIFIED. ) 
 CURVE ( )  GEOMETRIC_REPRESENTATION_ITEM ( )  RATIONAL_B_SPLINE_CURVE ( ( 0.9999999999999836797, 0.4567392136813330783, 0.3561768502900419797, 0.6983129098260927314 ) ) 
 REPRESENTATION_ITEM ( '' )  );
#25683 = CARTESIAN_POINT ( 'NONE',  ( -18.67409385759799179, -6.859212275519751323, 50.50378509014259265 ) ) ;
#25684 = CARTESIAN_POINT ( 'NONE',  ( -23.82366785274684418, -10.99486113721019009, 73.47697904737684382 ) ) ;
#25685 = ORIENTED_EDGE ( 'NONE', *, *, #15596, .T. ) ;
#25686 = FACE_OUTER_BOUND ( 'NONE', #5523, .T. ) ;
#25687 = CARTESIAN_POINT ( 'NONE',  ( -11.04141120970326462, -11.93494789359697883, 74.55840195308121565 ) ) ;
#25688 = CARTESIAN_POINT ( 'NONE',  ( -9.979603215878100286, -14.52052451035377345, 68.04295550616701860 ) ) ;
#25689 = ORIENTED_EDGE ( 'NONE', *, *, #23614, .F. ) ;
#25690 = CYLINDRICAL_SURFACE ( 'NONE', #44323, 0.1499999999999994671 ) ;
#25691 = CARTESIAN_POINT ( 'NONE',  ( -23.36642407317085812, -18.50986088251124073, 73.04751736639515514 ) ) ;
#25692 = CARTESIAN_POINT ( 'NONE',  ( -21.75868347184070473, -16.62218431696164345, 49.52966884056655772 ) ) ;
#25693 = CARTESIAN_POINT ( 'NONE',  ( -17.42409385541299471, -14.80920654474435771, 49.52966884056655772 ) ) ;
#25694 = VERTEX_POINT ( 'NONE', #21173 ) ;
#25695 = CARTESIAN_POINT ( 'NONE',  ( -21.58848639831018090, -8.631801418357438749, 73.75128750060586924 ) ) ;
#25697 =( BOUNDED_SURFACE ( )  B_SPLINE_SURFACE ( 3, 1, ( 
 ( #644, #7810 ),
 ( #15645, #26021 ),
 ( #26755, #41038 ),
 ( #37559, #26256 ),
 ( #37313, #30700 ),
 ( #41271, #11479 ),
 ( #40784, #3863 ) ),
 .UNSPECIFIED., .T., .F., .F. ) 
 B_SPLINE_SURFACE_WITH_KNOTS ( ( 4, 3, 4 ),
 ( 2, 2 ),
 ( 0.000000000000000000, 0.5000000000000000000, 1.000000000000000000 ),
 ( 0.000000000000000000, 1.000000000000000000 ),
 .UNSPECIFIED. ) 
 GEOMETRIC_REPRESENTATION_ITEM ( )  RATIONAL_B_SPLINE_SURFACE ( (
 ( 1.000000000000000000, 1.000000000000000000),
 ( 0.3333333333333335369, 0.3333333333333330373),
 ( 0.3333333333333335369, 0.3333333333333330373),
 ( 1.000000000000000000, 1.000000000000000000),
 ( 0.3333333333333333703, 0.3333333333333333703),
 ( 0.3333333333333333703, 0.3333333333333333703),
 ( 1.000000000000000000, 1.000000000000000000) ) ) 
 REPRESENTATION_ITEM ( '' )  SURFACE ( )  );
#25696 = DIRECTION ( 'NONE',  ( -7.110378524392051906E-06, -9.728165310344191876E-06, 0.9999999999274027385 ) ) ;
#25698 = ADVANCED_FACE ( 'NONE', ( #36166 ), #12566, .T. ) ;
#25699 = VECTOR ( 'NONE', #13307, 1000.000000000000000 ) ;
#25700 = AXIS2_PLACEMENT_3D ( 'NONE', #21996, #36991, #2786 ) ;
#25701 = CARTESIAN_POINT ( 'NONE',  ( -16.61787835827217563, -21.81669226458268795, 61.75567858111494246 ) ) ;
#25702 = EDGE_CURVE ( 'NONE', #18272, #12703, #23906, .T. ) ;
#25703 = EDGE_CURVE ( 'NONE', #11292, #22956, #38507, .T. ) ;
#25704 = CARTESIAN_POINT ( 'NONE',  ( -22.80534385650551954, -8.801233750844183135, 48.81488406609782515 ) ) ;
#25705 = EDGE_CURVE ( 'NONE', #2873, #17241, #3575, .T. ) ;
#25706 = ORIENTED_EDGE ( 'NONE', *, *, #33310, .F. ) ;
#25707 = DIRECTION ( 'NONE',  ( -5.731567514496413899E-31, -1.020425574103664789E-16, -1.000000000000000000 ) ) ;
#25708 = DIRECTION ( 'NONE',  ( -3.071710424422018668E-17, 6.404604876783312462E-16, 1.000000000000000000 ) ) ;
#25709 = VERTEX_POINT ( 'NONE', #17464 ) ;
#25710 = CARTESIAN_POINT ( 'NONE',  ( -24.22092292145011072, -12.93687797069018153, 66.60246741374322710 ) ) ;
#25711 = AXIS2_PLACEMENT_3D ( 'NONE', #4871, #39554, #20614 ) ;
#25712 = CYLINDRICAL_SURFACE ( 'NONE', #32149, 1.999999999999999112 ) ;
#25713 = CARTESIAN_POINT ( 'NONE',  ( -12.74563483257940177, -17.19133189234193893, 50.77966884056655772 ) ) ;
#25714 = ORIENTED_EDGE ( 'NONE', *, *, #32363, .T. ) ;
#25715 = DIRECTION ( 'NONE',  ( -3.071710424422018668E-17, 6.404604876783312462E-16, 1.000000000000000000 ) ) ;
#25716 = ORIENTED_EDGE ( 'NONE', *, *, #36464, .T. ) ;
#25717 = ORIENTED_EDGE ( 'NONE', *, *, #39122, .F. ) ;
#25718 = VERTEX_POINT ( 'NONE', #22380 ) ;
#25719 = CARTESIAN_POINT ( 'NONE',  ( -19.26159385650551670, -9.295667164867525756, 49.30633214617472504 ) ) ;
#25720 = CARTESIAN_POINT ( 'NONE',  ( -14.40713934193096080, -8.490940502754424912, 70.84030674940029826 ) ) ;
#25721 = CARTESIAN_POINT ( 'NONE',  ( -23.34190511704397153, -19.33504077159632573, 58.92764702605110472 ) ) ;
#25722 = CARTESIAN_POINT ( 'NONE',  ( -18.11889201384288484, -21.82488578508536747, 65.34532159284481168 ) ) ;
#25723 = CARTESIAN_POINT ( 'NONE',  ( -12.91576191806997542, -9.388722997169708151, 71.13453240065665284 ) ) ;
#25724 = ORIENTED_EDGE ( 'NONE', *, *, #11299, .F. ) ;
#25725 = VERTEX_POINT ( 'NONE', #26082 ) ;
#25726 = CARTESIAN_POINT ( 'NONE',  ( -14.39909385650551776, -8.114302828567740988, 52.18300498402516041 ) ) ;
#25727 = EDGE_CURVE ( 'NONE', #15919, #15234, #18421, .T. ) ;
#25728 = CARTESIAN_POINT ( 'NONE',  ( -14.56979395989184844, -7.868632093599801536, 54.02222386812614729 ) ) ;
#25729 = CARTESIAN_POINT ( 'NONE',  ( -24.47401588851211329, -14.84236380343934592, 59.24300237059242136 ) ) ;
#25730 = CARTESIAN_POINT ( 'NONE',  ( -20.41784385650551314, -9.790100578890868377, 49.79778022625163203 ) ) ;
#25731 = CIRCLE ( 'NONE', #9993, 2.500000000000000444 ) ;
#25732 = AXIS2_PLACEMENT_3D ( 'NONE', #24070, #19645, #8818 ) ;
#25733 = EDGE_LOOP ( 'NONE', ( #43450, #39021, #12185, #3481, #21525 ) ) ;
#25734 = CARTESIAN_POINT ( 'NONE',  ( -24.36278531766821231, -15.73455962487135551, 69.83307441201348809 ) ) ;
#25735 = EDGE_CURVE ( 'NONE', #30777, #31226, #5343, .T. ) ;
#25736 = CARTESIAN_POINT ( 'NONE',  ( -13.78028125966771178, -8.764572710043150749, 74.35521961121672518 ) ) ;
#25737 = AXIS2_PLACEMENT_3D ( 'NONE', #1276, #31085, #42173 ) ;
#25738 = CARTESIAN_POINT ( 'NONE',  ( -50.42609385541305755, -14.90920654474411577, 58.90588235294116970 ) ) ;
#25739 = ORIENTED_EDGE ( 'NONE', *, *, #28644, .F. ) ;
#25740 = CARTESIAN_POINT ( 'NONE',  ( -17.02512887036163747, -21.84805734118084786, 72.45983438422057077 ) ) ;
#25741 = EDGE_LOOP ( 'NONE', ( #42501, #36926, #44477, #34404 ) ) ;
#25742 = CARTESIAN_POINT ( 'NONE',  ( -19.65534385541296203, -8.623186033802625161, 49.24843789510452297 ) ) ;
#25743 = CARTESIAN_POINT ( 'NONE',  ( -20.31445822498897513, -8.433666593767874531, 66.78104076700890346 ) ) ;
#25744 = CARTESIAN_POINT ( 'NONE',  ( -24.42383173988974221, -14.88139849484145216, 59.54300232022885808 ) ) ;
#25745 = CARTESIAN_POINT ( 'NONE',  ( -24.40658449907488148, -15.78251210865724907, 69.53307488410803217 ) ) ;
#25746 = ORIENTED_EDGE ( 'NONE', *, *, #33423, .F. ) ;
#25747 = CARTESIAN_POINT ( 'NONE',  ( -23.44246603937665441, -11.23440635791340370, 70.08313896382058772 ) ) ;
#25748 = CARTESIAN_POINT ( 'NONE',  ( -22.77624011198484411, -19.99176503748672218, 72.76683626849190034 ) ) ;
#25749 = CARTESIAN_POINT ( 'NONE',  ( -19.36749320447652067, -7.617017704847905080, 60.13809874652617538 ) ) ;
#25750 = CARTESIAN_POINT ( 'NONE',  ( -21.18398602608336745, -21.24092397535611809, 65.69958545398036165 ) ) ;
#25751 = ORIENTED_EDGE ( 'NONE', *, *, #32580, .T. ) ;
#25752 = CARTESIAN_POINT ( 'NONE',  ( -15.10382451463400955, -18.89477942154363888, 49.52966884056656482 ) ) ;
#25753 = LINE ( 'NONE', #10735, #31320 ) ;
#25754 = CARTESIAN_POINT ( 'NONE',  ( -10.70296955259081351, -11.59513340129999648, 71.27356289404251299 ) ) ;
#25755 = EDGE_LOOP ( 'NONE', ( #2606, #20311, #31534, #24766, #42523 ) ) ;
#25756 = FACE_BOUND ( 'NONE', #6963, .T. ) ;
#25757 = VERTEX_POINT ( 'NONE', #13752 ) ;
#25758 = ADVANCED_FACE ( 'NONE', ( #48468 ), #40844, .T. ) ;
#25759 = EDGE_CURVE ( 'NONE', #24420, #46610, #32948, .T. ) ;
#25760 = CARTESIAN_POINT ( 'NONE',  ( -21.23484681875272528, -20.74088929683185611, 69.33978048267414351 ) ) ;
#25761 = CARTESIAN_POINT ( 'NONE',  ( -24.64856881849836157, -12.98951230985249516, 62.95451385596734184 ) ) ;
#25762 = LINE ( 'NONE', #33366, #31305 ) ;
#25763 = VECTOR ( 'NONE', #24974, 1000.000000000000000 ) ;
#25764 = CARTESIAN_POINT ( 'NONE',  ( -15.95864454847012581, -7.504678945485328434, 63.71365074502104875 ) ) ;
#25765 = VERTEX_POINT ( 'NONE', #29284 ) ;
#25766 = DIRECTION ( 'NONE',  ( -0.9687793358424822143, 0.2479245821708672415, 0.000000000000000000 ) ) ;
#25767 = VERTEX_POINT ( 'NONE', #2687 ) ;
#25768 = CARTESIAN_POINT ( 'NONE',  ( -12.67420009981309548, -9.069561984988212089, 71.00958696908303125 ) ) ;
#25769 = CYLINDRICAL_SURFACE ( 'NONE', #7036, 0.1499999999999953038 ) ;
#25770 = EDGE_LOOP ( 'NONE', ( #42614, #29682, #10708, #12745 ) ) ;
#25771 = CARTESIAN_POINT ( 'NONE',  ( -20.54979434103954006, -8.489990112051950533, 63.61121512946457557 ) ) ;
#25772 = VECTOR ( 'NONE', #17014, 1000.000000000000000 ) ;
#25773 = ADVANCED_FACE ( 'NONE', ( #7375 ), #48271, .T. ) ;
#25774 = EDGE_CURVE ( 'NONE', #21441, #14380, #4210, .T. ) ;
#25775 = CARTESIAN_POINT ( 'NONE',  ( -13.52463770777002416, -20.62256002460651061, 58.11938029867636146 ) ) ;
#25776 = ORIENTED_EDGE ( 'NONE', *, *, #27963, .T. ) ;
#25777 = ORIENTED_EDGE ( 'NONE', *, *, #5941, .T. ) ;
#25778 = EDGE_CURVE ( 'NONE', #15450, #40523, #47909, .T. ) ;
#25779 = CARTESIAN_POINT ( 'NONE',  ( -26.42409385541305511, -15.80920654474410725, 63.99999999999998579 ) ) ;
#25780 = CARTESIAN_POINT ( 'NONE',  ( -23.22061493458723191, -18.82855841280685993, 69.59372281959836926 ) ) ;
#25781 = VECTOR ( 'NONE', #36456, 1000.000000000000000 ) ;
#25782 = CARTESIAN_POINT ( 'NONE',  ( -11.55760334190795646, -18.71930654562736507, 65.04147253430677722 ) ) ;
#25783 = CARTESIAN_POINT ( 'NONE',  ( -10.32448118053900998, -17.06708155110676728, 57.83760547180983025 ) ) ;
#25784 = PLANE ( 'NONE',  #47183 ) ;
#25785 = CARTESIAN_POINT ( 'NONE',  ( -14.30855566557790226, -8.484641631233271752, 70.74429704309763167 ) ) ;
#25786 = CARTESIAN_POINT ( 'NONE',  ( -12.88034385759799250, -9.360768649639304329, 51.01397948905922419 ) ) ;
#25787 = VECTOR ( 'NONE', #15956, 1000.000000000000000 ) ;
#25788 = EDGE_LOOP ( 'NONE', ( #10776, #22137, #14646, #45805 ) ) ;
#25789 = ORIENTED_EDGE ( 'NONE', *, *, #37540, .T. ) ;
#25790 = CARTESIAN_POINT ( 'NONE',  ( -24.43827367352892210, -15.52193379869737377, 73.28831629023289906 ) ) ;
#25791 = EDGE_CURVE ( 'NONE', #11764, #8655, #37127, .T. ) ;
#25792 = CARTESIAN_POINT ( 'NONE',  ( -43.04835856129541583, -14.90920654474411577, 58.00588235294116402 ) ) ;
#25793 = CARTESIAN_POINT ( 'NONE',  ( -21.07871280138893155, -21.30141328949765267, 62.25324875861664964 ) ) ;
#25794 = CARTESIAN_POINT ( 'NONE',  ( -19.25408589567127038, -10.49476435801947893, 52.02966884056656482 ) ) ;
#25795 = DIRECTION ( 'NONE',  ( 0.9753750245375039096, 0.2205528542287732985, 7.244220459260265297E-08 ) ) ;
#25796 = ORIENTED_EDGE ( 'NONE', *, *, #10220, .T. ) ;
#25797 = CARTESIAN_POINT ( 'NONE',  ( -19.26159385650551670, -9.295667164867525756, 49.30633214617472504 ) ) ;
#25798 = ORIENTED_EDGE ( 'NONE', *, *, #15998, .F. ) ;
#25799 = CARTESIAN_POINT ( 'NONE',  ( -22.00056395679878918, -20.10656929443474183, 62.51822596018408262 ) ) ;
#25800 = CARTESIAN_POINT ( 'NONE',  ( -14.47983227664519212, -7.965588925009814858, 63.90483403727078837 ) ) ;
#25801 = AXIS2_PLACEMENT_3D ( 'NONE', #44013, #9360, #10268 ) ;
#25802 = CARTESIAN_POINT ( 'NONE',  ( -10.88286923018596575, -17.43962093083235843, 68.11193994895104709 ) ) ;
#25803 = CIRCLE ( 'NONE', #35246, 1.500000000000001332 ) ;
#25804 = VERTEX_POINT ( 'NONE', #48226 ) ;
#25805 = CIRCLE ( 'NONE', #4585, 4.686499999999997890 ) ;
#25806 = CARTESIAN_POINT ( 'NONE',  ( -10.52647097981341773, -16.26776460278879810, 71.74190558978101251 ) ) ;
#25807 = CARTESIAN_POINT ( 'NONE',  ( -14.80624636014071172, -8.317144122717282428, 60.61996281969079803 ) ) ;
#25808 = ORIENTED_EDGE ( 'NONE', *, *, #16613, .F. ) ;
#25809 = CARTESIAN_POINT ( 'NONE',  ( -15.25374053646965855, -21.46424723517000643, 65.21482766330532854 ) ) ;
#25810 = DIRECTION ( 'NONE',  ( -0.9687793358424819923, 0.2479245821708680464, 0.000000000000000000 ) ) ;
#25811 = EDGE_LOOP ( 'NONE', ( #15581, #39972 ) ) ;
#25812 = DIRECTION ( 'NONE',  ( -0.9180681052388980357, 0.3964226963016364014, 0.000000000000000000 ) ) ;
#25813 = EDGE_LOOP ( 'NONE', ( #44799, #29069 ) ) ;
#25814 = CARTESIAN_POINT ( 'NONE',  ( -10.30936164548169565, -17.01954009666350842, 57.84907067837097827 ) ) ;
#25815 = CARTESIAN_POINT ( 'NONE',  ( -24.87306303946944652, -14.67811516855542742, 62.89109217698693755 ) ) ;
#25816 = ORIENTED_EDGE ( 'NONE', *, *, #12416, .T. ) ;
#25817 = EDGE_CURVE ( 'NONE', #14105, #47823, #33445, .T. ) ;
#25818 = CARTESIAN_POINT ( 'NONE',  ( -12.84817825325788299, -8.930034686467767102, 67.42296837860310177 ) ) ;
#25819 = CARTESIAN_POINT ( 'NONE',  ( -18.60622205832422082, -22.16490843864383109, 72.47006330605313451 ) ) ;
#25820 = ORIENTED_EDGE ( 'NONE', *, *, #39665, .F. ) ;
#25821 = CARTESIAN_POINT ( 'NONE',  ( -18.79451800406743800, -7.944217934494487210, 70.65451536062514037 ) ) ;
#25822 =( BOUNDED_CURVE ( )  B_SPLINE_CURVE ( 3, ( #22758, #37248, #30147, #34054 ),
 .UNSPECIFIED., .F., .F. ) 
 B_SPLINE_CURVE_WITH_KNOTS ( ( 4, 4 ),
 ( 0.5000000000000000000, 0.9074455897393649551 ),
 .UNSPECIFIED. ) 
 CURVE ( )  GEOMETRIC_REPRESENTATION_ITEM ( )  RATIONAL_B_SPLINE_CURVE ( ( 0.9999999999999769074, 0.4567392136813299697, 0.3561768502900456435, 0.6983129098260987266 ) ) 
 REPRESENTATION_ITEM ( '' )  );
#25823 = LINE ( 'NONE', #11059, #7064 ) ;
#25824 = CARTESIAN_POINT ( 'NONE',  ( -21.56516322056021195, -8.616078523729070682, 73.79402879848014152 ) ) ;
#25825 = EDGE_LOOP ( 'NONE', ( #41250, #31903, #632, #47447, #42875, #14633, #48177, #12300, #12079, #18394, #45706, #48446, #29912, #4533, #9393, #43162, #18414, #38486, #9117, #36914, #45143, #45140, #25998, #28508, #6722, #23582, #6891, #14881, #25099, #1202, #10232, #8363, #8672, #39753, #26695, #29961, #36084, #40776, #42923, #14857, #30942, #18768, #6553, #16173, #7761, #31741, #3151, #14652, #6422, #35446, #1593, #4859, #9922, #33066, #21107, #22670, #13595, #17890, #3513, #13855, #25995, #7996, #1973, #23951, #491, #31408, #48693, #11300, #36472, #13806, #13764, #28996, #20284, #12161, #20332, #36279, #31538, #35414, #41943, #20201, #19344, #21711, #39527, #16988, #8673, #10469, #41353, #32117, #21332, #4459, #26013, #13662, #2541, #40595, #13138, #16152, #38872, #31140, #30879, #16007, #45736, #9380, #22847, #14341, #36371, #4631, #17669, #28924, #14870, #48331, #24395, #36967, #30581, #9716, #7854, #33176, #9266, #29562, #24438, #21425, #14819, #28904, #18829, #16221, #27393, #47222, #32764, #2402, #23154, #42524, #18711, #23221, #30009, #8580, #31946, #1462, #36579, #35006, #10615, #42626, #40075, #25633, #15604, #41924, #47525, #3468, #25096, #33145, #242, #23119, #666, #12444, #690, #48361, #39038, #11311, #13549, #5138, #22523, #5043, #29381, #2954, #16132, #47266, #9407 ) ) ;
#25826 = FACE_OUTER_BOUND ( 'NONE', #22814, .T. ) ;
#25827 = B_SPLINE_CURVE_WITH_KNOTS ( 'NONE', 3,
 ( #28333, #2212, #27835, #36416, #39409, #20938, #28805, #2463, #43097, #39155 ),
 .UNSPECIFIED., .F., .F.,
 ( 4, 2, 2, 2, 4 ),
 ( 0.000000000000000000, 0.2500000000000000000, 0.5000000000000000000, 0.7500000000000000000, 1.000000000000000000 ),
 .UNSPECIFIED. ) ;
#25828 = ADVANCED_FACE ( 'NONE', ( #3416 ), #34177, .T. ) ;
#25829 = CARTESIAN_POINT ( 'NONE',  ( -11.41497376296057098, -19.21309731666858411, 71.80190493362104576 ) ) ;
#25830 = ORIENTED_EDGE ( 'NONE', *, *, #31436, .T. ) ;
#25831 = ORIENTED_EDGE ( 'NONE', *, *, #24296, .T. ) ;
#25832 = EDGE_CURVE ( 'NONE', #12513, #20130, #37673, .T. ) ;
#25833 = CARTESIAN_POINT ( 'NONE',  ( -22.84886394736722792, -9.702774549906752810, 73.59665770010028041 ) ) ;
#25834 = CYLINDRICAL_SURFACE ( 'NONE', #28150, 0.1500000000000014932 ) ;
#25836 = CARTESIAN_POINT ( 'NONE',  ( -10.42546210075913748, -12.25520342886974845, 57.44361899967025664 ) ) ;
#25835 = VECTOR ( 'NONE', #38906, 1000.000000000000000 ) ;
#25837 = CARTESIAN_POINT ( 'NONE',  ( -15.52409385759799143, -9.359200813967568422, 50.49621490985803263 ) ) ;
#25838 = EDGE_CURVE ( 'NONE', #20038, #21687, #236, .T. ) ;
#25839 = CARTESIAN_POINT ( 'NONE',  ( -23.13305522301093120, -10.65917872773856878, 63.21619042434998903 ) ) ;
#25840 = VECTOR ( 'NONE', #30110, 1000.000000000000000 ) ;
#25841 = CARTESIAN_POINT ( 'NONE',  ( -19.23866243364646422, -21.62168334911581269, 58.52507384657483414 ) ) ;
#25842 = CARTESIAN_POINT ( 'NONE',  ( -24.34442481654545176, -17.56831618823577301, 65.98711337262309939 ) ) ;
#25843 =( BOUNDED_CURVE ( )  B_SPLINE_CURVE ( 3, ( #11993, #46692, #23565, #27003 ),
 .UNSPECIFIED., .F., .F. ) 
 B_SPLINE_CURVE_WITH_KNOTS ( ( 4, 4 ),
 ( 0.5000000000000000000, 0.9074455897393653991 ),
 .UNSPECIFIED. ) 
 CURVE ( )  GEOMETRIC_REPRESENTATION_ITEM ( )  RATIONAL_B_SPLINE_CURVE ( ( 0.9999999999999921174, 0.4567392136813264170, 0.3561768502900336530, 0.6983129098261052770 ) ) 
 REPRESENTATION_ITEM ( '' )  );
#25844 = AXIS2_PLACEMENT_3D ( 'NONE', #29835, #44861, #26139 ) ;
#25845 = CIRCLE ( 'NONE', #1480, 2.404255319148937531 ) ;
#25846 = DIRECTION ( 'NONE',  ( 0.9132646967824439299, -0.4073666574609056124, 8.344532078871960245E-09 ) ) ;
#25847 = VERTEX_POINT ( 'NONE', #48722 ) ;
#25848 = CARTESIAN_POINT ( 'NONE',  ( -20.94465692579565896, -8.243430592510261334, 59.95629952546280350 ) ) ;
#25849 = FACE_OUTER_BOUND ( 'NONE', #16928, .T. ) ;
#25850 = CARTESIAN_POINT ( 'NONE',  ( -21.09639645740537617, -17.74003392703708926, 52.02966884056656482 ) ) ;
#25851 = CARTESIAN_POINT ( 'NONE',  ( -20.46316679850361808, -18.39244407412632043, 52.02966884056656482 ) ) ;
#25852 = VERTEX_POINT ( 'NONE', #710 ) ;
#25853 =( BOUNDED_CURVE ( )  B_SPLINE_CURVE ( 3, ( #42170, #42419, #8689, #19509 ),
 .UNSPECIFIED., .F., .F. ) 
 B_SPLINE_CURVE_WITH_KNOTS ( ( 4, 4 ),
 ( 0.000000000000000000, 0.4074455897393610693 ),
 .UNSPECIFIED. ) 
 CURVE ( )  GEOMETRIC_REPRESENTATION_ITEM ( )  RATIONAL_B_SPLINE_CURVE ( ( 1.000000000000000000, 0.4567392136813320791, 0.3561768502900303779, 0.6983129098260949519 ) ) 
 REPRESENTATION_ITEM ( '' )  );
#25854 = VERTEX_POINT ( 'NONE', #3659 ) ;
#25855 = CYLINDRICAL_SURFACE ( 'NONE', #31195, 1.249999999999998668 ) ;
#25856 = CARTESIAN_POINT ( 'NONE',  ( -10.42334078895570926, -15.64104556165006521, 61.18789045260545834 ) ) ;
#25857 = CARTESIAN_POINT ( 'NONE',  ( -15.40060450416582860, -21.97927049188689708, 72.16762693854772692 ) ) ;
#25858 = CARTESIAN_POINT ( 'NONE',  ( -11.85162103594838001, -10.49015045520576983, 71.25420998615621215 ) ) ;
#25859 = ORIENTED_EDGE ( 'NONE', *, *, #15875, .T. ) ;
#25860 = CARTESIAN_POINT ( 'NONE',  ( -24.49635653881819408, -12.46679777644911447, 73.35730153580948354 ) ) ;
#25861 = CARTESIAN_POINT ( 'NONE',  ( -10.85887813628090015, -11.28619579020030628, 64.26226673522833721 ) ) ;
#25862 = ORIENTED_EDGE ( 'NONE', *, *, #34274, .F. ) ;
#25863 = CARTESIAN_POINT ( 'NONE',  ( -22.01912385291013408, -9.457520419221951968, 63.49153900988868315 ) ) ;
#25864 = VECTOR ( 'NONE', #21959, 1000.000000000000114 ) ;
#25865 = CARTESIAN_POINT ( 'NONE',  ( -23.06443888862362002, -10.57364818883473667, 63.16366193195977985 ) ) ;
#25866 =( GEOMETRIC_REPRESENTATION_CONTEXT ( 3 ) GLOBAL_UNCERTAINTY_ASSIGNED_CONTEXT ( ( #38115 ) ) GLOBAL_UNIT_ASSIGNED_CONTEXT ( ( #5152, #24106, #31488 ) ) REPRESENTATION_CONTEXT ( 'NONE', 'WORKASPACE' ) );
#25867 = CARTESIAN_POINT ( 'NONE',  ( -24.75383108144848165, -16.14659837148148824, 66.24980321609697853 ) ) ;
#25868 = ADVANCED_FACE ( 'NONE', ( #41584 ), #15949, .T. ) ;
#25869 = ORIENTED_EDGE ( 'NONE', *, *, #21730, .T. ) ;
#25870 = CARTESIAN_POINT ( 'NONE',  ( -24.15708737698322395, -12.88964658164904620, 70.00072905108670795 ) ) ;
#25871 = VECTOR ( 'NONE', #20536, 1000.000000000000000 ) ;
#25872 = VECTOR ( 'NONE', #36466, 1000.000000000000114 ) ;
#25873 = EDGE_LOOP ( 'NONE', ( #23085, #40584, #20678, #3963, #44282 ) ) ;
#25874 = CARTESIAN_POINT ( 'NONE',  ( -22.47245519635065492, -19.73066437834766873, 72.65872596779033188 ) ) ;
#25875 = CARTESIAN_POINT ( 'NONE',  ( -23.62594491300536959, -11.45603751788689451, 66.70742424642772050 ) ) ;
#25876 = ORIENTED_EDGE ( 'NONE', *, *, #28302, .F. ) ;
#25877 = DIRECTION ( 'NONE',  ( 0.7248509490090241369, -0.6889057277456160922, 1.880377065355303572E-09 ) ) ;
#25878 = CARTESIAN_POINT ( 'NONE',  ( -10.29339667142563819, -12.65123896477911103, 64.52482037846105811 ) ) ;
#25879 = CARTESIAN_POINT ( 'NONE',  ( -20.86784385650551954, -6.428312510596451368, 51.20221977374900035 ) ) ;
#25880 = DIRECTION ( 'NONE',  ( -3.071710424422018668E-17, 6.404604876783312462E-16, 1.000000000000000000 ) ) ;
#25881 = AXIS2_PLACEMENT_3D ( 'NONE', #5851, #47213, #32436 ) ;
#25882 = CARTESIAN_POINT ( 'NONE',  ( -10.05964041407737497, -15.93577270795842615, 64.62958807307776965 ) ) ;
#25883 = CARTESIAN_POINT ( 'NONE',  ( -24.43362369560107794, -14.05489154181400124, 73.27271507725298250 ) ) ;
#25884 = CARTESIAN_POINT ( 'NONE',  ( -16.12334351384450670, -20.16700684834330914, 53.88362224778186516 ) ) ;
#25885 = VERTEX_POINT ( 'NONE', #19667 ) ;
#25886 = CARTESIAN_POINT ( 'NONE',  ( -46.42632161746406894, -13.24559821555319239, 70.13000000000000966 ) ) ;
#25887 = DIRECTION ( 'NONE',  ( -1.916827911674356108E-06, -6.156520247306097078E-06, 0.9999999999792114069 ) ) ;
#25888 = CARTESIAN_POINT ( 'NONE',  ( -35.42409385541304800, -8.109206544743658540, 50.50000000000030553 ) ) ;
#25889 = CARTESIAN_POINT ( 'NONE',  ( -22.22619444978876757, -20.50513558618911958, 58.94938304221643222 ) ) ;
#25890 = DIRECTION ( 'NONE',  ( -3.071710424422018668E-17, 6.404604876783312462E-16, 1.000000000000000000 ) ) ;
#25891 = CARTESIAN_POINT ( 'NONE',  ( -17.05186597850482144, -7.819110227248425637, 70.59921951062938206 ) ) ;
#25892 = ORIENTED_EDGE ( 'NONE', *, *, #7660, .F. ) ;
#25893 = VERTEX_POINT ( 'NONE', #38351 ) ;
#25894 = EDGE_CURVE ( 'NONE', #4171, #28824, #47636, .T. ) ;
#25895 = CARTESIAN_POINT ( 'NONE',  ( -23.75243126011088890, -11.69520888738364306, 66.83703234806088744 ) ) ;
#25896 = CARTESIAN_POINT ( 'NONE',  ( -24.87290000513101873, -14.67112934921935974, 62.82801050733710468 ) ) ;
#25897 = ORIENTED_EDGE ( 'NONE', *, *, #32376, .F. ) ;
#25899 = CARTESIAN_POINT ( 'NONE',  ( -13.94909385650551492, -8.104110260919579645, 48.81699501597546487 ) ) ;
#25898 = CARTESIAN_POINT ( 'NONE',  ( -23.56005053104643210, -11.33143871826892912, 66.30725794404830253 ) ) ;
#25900 = CARTESIAN_POINT ( 'NONE',  ( -11.36795091080559850, -18.31963851737709348, 58.10714594516144871 ) ) ;
#25901 = CARTESIAN_POINT ( 'NONE',  ( -14.25068793291388047, -8.513811817964199946, 71.02957628655769895 ) ) ;
#25902 = EDGE_CURVE ( 'NONE', #39406, #12959, #35324, .T. ) ;
#25903 = CARTESIAN_POINT ( 'NONE',  ( -10.54994933093899867, -13.24305344519376781, 71.49356453765415154 ) ) ;
#25904 = FACE_BOUND ( 'NONE', #20937, .T. ) ;
#25905 = PLANE ( 'NONE',  #1138 ) ;
#25906 = CARTESIAN_POINT ( 'NONE',  ( -10.03450206504577125, -13.86240527909647824, 57.59825032318321547 ) ) ;
#25907 = EDGE_CURVE ( 'NONE', #24257, #28351, #26692, .T. ) ;
#25908 = DIRECTION ( 'NONE',  ( 0.6380325334150255268, -0.7700094066334542964, 0.000000000000000000 ) ) ;
#25909 = ORIENTED_EDGE ( 'NONE', *, *, #36773, .F. ) ;
#25910 = FACE_OUTER_BOUND ( 'NONE', #21383, .T. ) ;
#25911 = CARTESIAN_POINT ( 'NONE',  ( -10.66644504159021878, -12.78954850062448578, 68.15321152835137752 ) ) ;
#25912 = AXIS2_PLACEMENT_3D ( 'NONE', #30132, #45157, #11398 ) ;
#25913 = CARTESIAN_POINT ( 'NONE',  ( -19.84060227527380249, -21.38033787448792467, 72.62034542409985249 ) ) ;
#25914 = CARTESIAN_POINT ( 'NONE',  ( -24.29765713679916317, -13.47630389642528215, 59.47341129314763464 ) ) ;
#25915 = DIRECTION ( 'NONE',  ( 1.000000000000000000, 2.866981220435666553E-17, 0.000000000000000000 ) ) ;
#25916 = EDGE_CURVE ( 'NONE', #29955, #25765, #6237, .T. ) ;
#25917 = CARTESIAN_POINT ( 'NONE',  ( -13.70502021987594077, -20.80197949353049580, 68.87113990053892110 ) ) ;
#25918 = CARTESIAN_POINT ( 'NONE',  ( -23.42915847708036381, -11.11517115755410146, 73.64721174900437006 ) ) ;
#25919 = EDGE_CURVE ( 'NONE', #37096, #16722, #18931, .T. ) ;
#25920 = AXIS2_PLACEMENT_3D ( 'NONE', #47043, #1750, #16742 ) ;
#25921 = AXIS2_PLACEMENT_3D ( 'NONE', #40602, #40377, #14475 ) ;
#25922 = VERTEX_POINT ( 'NONE', #30274 ) ;
#25923 = EDGE_LOOP ( 'NONE', ( #11836, #29285, #21932, #27269, #47572 ) ) ;
#25924 = CARTESIAN_POINT ( 'NONE',  ( -13.74909385541304374, -8.112991634885936776, 51.74999426922421719 ) ) ;
#25925 = ORIENTED_EDGE ( 'NONE', *, *, #4999, .F. ) ;
#25926 = CARTESIAN_POINT ( 'NONE',  ( 8.575906144586950219, -6.109215713985405749, 50.50605614422795497 ) ) ;
#25927 = CARTESIAN_POINT ( 'NONE',  ( -18.59285626271963210, -7.848678033734123538, 67.05638626395584367 ) ) ;
#25928 = CIRCLE ( 'NONE', #11768, 2.000000000000001776 ) ;
#25929 = B_SPLINE_CURVE_WITH_KNOTS ( 'NONE', 1,
 ( #31404, #5310 ),
 .UNSPECIFIED., .F., .F.,
 ( 2, 2 ),
 ( 0.000000000000000000, 1.000000000000000000 ),
 .UNSPECIFIED. ) ;
#25930 = DIRECTION ( 'NONE',  ( -3.071710424422018668E-17, 6.404604876783312462E-16, 1.000000000000000000 ) ) ;
#25931 = CARTESIAN_POINT ( 'NONE',  ( -16.13432406759100246, -21.74052631579560568, 58.30057715624173653 ) ) ;
#25932 = ORIENTED_EDGE ( 'NONE', *, *, #27908, .T. ) ;
#25933 = CARTESIAN_POINT ( 'NONE',  ( -24.36668221452861971, -15.71384968925034364, 73.23133671100342212 ) ) ;
#25934 = CARTESIAN_POINT ( 'NONE',  ( -33.95962776134579286, -8.109206544744111511, 50.50000000000000000 ) ) ;
#25935 = VERTEX_POINT ( 'NONE', #30520 ) ;
#25936 = EDGE_CURVE ( 'NONE', #42966, #42781, #6478, .T. ) ;
#25937 = CARTESIAN_POINT ( 'NONE',  ( -23.37999588001404661, -18.58199455739222827, 69.57899840282863124 ) ) ;
#25938 = VERTEX_POINT ( 'NONE', #24582 ) ;
#25939 = CARTESIAN_POINT ( 'NONE',  ( -10.82908108634309663, -17.30933488606310178, 68.51210539238705621 ) ) ;
#25940 = CARTESIAN_POINT ( 'NONE',  ( -15.06268261486707338, -8.219072439155830523, 57.13383403554141893 ) ) ;
#25941 = CARTESIAN_POINT ( 'NONE',  ( -9.982384861202168835, -14.45670355602896073, 67.96525964217694593 ) ) ;
#25942 = VERTEX_POINT ( 'NONE', #20391 ) ;
#25943 = CARTESIAN_POINT ( 'NONE',  ( -22.09908899289463591, -14.48102562737866705, 49.52966884056655772 ) ) ;
#25944 = CARTESIAN_POINT ( 'NONE',  ( -15.81235419205221504, -7.945607373518417837, 67.42535135806457447 ) ) ;
#25945 = CIRCLE ( 'NONE', #14867, 5.249999999999998224 ) ;
#25946 = DIRECTION ( 'NONE',  ( -1.000000000000000000, 0.000000000000000000, 9.637352644315596475E-17 ) ) ;
#25947 = CARTESIAN_POINT ( 'NONE',  ( -22.11764131551248269, -20.59576654024708731, 58.95098234965121264 ) ) ;
#25948 = ORIENTED_EDGE ( 'NONE', *, *, #38732, .F. ) ;
#25949 = DIRECTION ( 'NONE',  ( -0.8037372918934695409, 0.5949843406508663612, 7.322964617522835370E-08 ) ) ;
#25950 = CARTESIAN_POINT ( 'NONE',  ( -16.50530592306966682, -19.40475993746870387, 49.52966884056656482 ) ) ;
#25951 = EDGE_CURVE ( 'NONE', #7670, #38928, #9561, .T. ) ;
#25952 = AXIS2_PLACEMENT_3D ( 'NONE', #8598, #23627, #9578 ) ;
#25953 = CARTESIAN_POINT ( 'NONE',  ( -24.72409385541305582, -14.90920654474422058, 68.06470588235292496 ) ) ;
#25954 = CARTESIAN_POINT ( 'NONE',  ( -18.34560609025200861, -9.386954687716537293, 54.07175714974878389 ) ) ;
#25955 = CARTESIAN_POINT ( 'NONE',  ( -18.24909385650551741, -8.104110260919579645, 48.81699501597546487 ) ) ;
#25956 = EDGE_LOOP ( 'NONE', ( #38655, #9052 ) ) ;
#25957 = DIRECTION ( 'NONE',  ( -3.071710424422018668E-17, 6.404604876783312462E-16, 1.000000000000000000 ) ) ;
#25958 = CARTESIAN_POINT ( 'NONE',  ( -14.47983125967835960, -7.965589368325148634, 63.90483512601500848 ) ) ;
#25959 = ORIENTED_EDGE ( 'NONE', *, *, #20845, .T. ) ;
#25960 = CARTESIAN_POINT ( 'NONE',  ( -19.57699614054808634, -21.94144247634149281, 62.17999043330664222 ) ) ;
#25961 = VECTOR ( 'NONE', #14785, 1000.000000000000000 ) ;
#25962 = CARTESIAN_POINT ( 'NONE',  ( -15.36368464484735874, -8.119310132577721717, 74.27088789173198791 ) ) ;
#25963 = CARTESIAN_POINT ( 'NONE',  ( -11.74167521261877134, -9.991000739040469369, 67.66043377903119449 ) ) ;
#25964 = ORIENTED_EDGE ( 'NONE', *, *, #16620, .F. ) ;
#25965 = CARTESIAN_POINT ( 'NONE',  ( -10.04946558025865500, -15.86660702602552320, 64.70109908442724134 ) ) ;
#25966 = ADVANCED_FACE ( 'NONE', ( #46251 ), #26580, .T. ) ;
#25967 = CARTESIAN_POINT ( 'NONE',  ( -14.62089650835144816, -21.71189251387697894, 58.30471404203333918 ) ) ;
#25968 = ORIENTED_EDGE ( 'NONE', *, *, #38034, .F. ) ;
#25969 = ORIENTED_EDGE ( 'NONE', *, *, #5934, .T. ) ;
#25970 = CARTESIAN_POINT ( 'NONE',  ( -15.60534385650551847, -8.801233750844183135, 48.81488406609782515 ) ) ;
#25971 = EDGE_CURVE ( 'NONE', #1137, #39506, #36332, .T. ) ;
#25972 = ADVANCED_FACE ( 'NONE', ( #2146 ), #17149, .T. ) ;
#25973 = LINE ( 'NONE', #7273, #37388 ) ;
#25974 = CARTESIAN_POINT ( 'NONE',  ( -14.08295856548867597, -8.150414966537949724, 70.82983378092882276 ) ) ;
#25975 = CARTESIAN_POINT ( 'NONE',  ( -23.12302657392458016, -18.95946740514217765, 62.35406880581413702 ) ) ;
#25976 = ORIENTED_EDGE ( 'NONE', *, *, #28663, .F. ) ;
#25977 = VERTEX_POINT ( 'NONE', #38853 ) ;
#25978 = CARTESIAN_POINT ( 'NONE',  ( -15.13034385650551528, -9.794322478646142471, 51.19202720610083901 ) ) ;
#25979 = CIRCLE ( 'NONE', #40112, 1.999999999999999556 ) ;
#25980 = CARTESIAN_POINT ( 'NONE',  ( -10.83536388074712598, -17.31742051234312640, 64.92739380450886699 ) ) ;
#25981 = FACE_OUTER_BOUND ( 'NONE', #48611, .T. ) ;
#25982 = VECTOR ( 'NONE', #32306, 1000.000000000000114 ) ;
#25983 =( BOUNDED_CURVE ( )  B_SPLINE_CURVE ( 3, ( #9181, #28846, #1535, #39454 ),
 .UNSPECIFIED., .F., .F. ) 
 B_SPLINE_CURVE_WITH_KNOTS ( ( 4, 4 ),
 ( 0.9074455897393670645, 1.000000000000000000 ),
 .UNSPECIFIED. ) 
 CURVE ( )  GEOMETRIC_REPRESENTATION_ITEM ( )  RATIONAL_B_SPLINE_CURVE ( ( 0.6983129098260929535, 0.7760317562606982023, 0.8765941196520005141, 1.000000000000000000 ) ) 
 REPRESENTATION_ITEM ( '' )  );
#25985 = EDGE_CURVE ( 'NONE', #24088, #15624, #17, .T. ) ;
#25984 = CARTESIAN_POINT ( 'NONE',  ( -16.98659385650551812, -9.302874398569244363, 51.68646062012417985 ) ) ;
#25986 = AXIS2_PLACEMENT_3D ( 'NONE', #1198, #12528, #23874 ) ;
#25987 = EDGE_CURVE ( 'NONE', #40177, #3121, #14613, .T. ) ;
#25988 = ORIENTED_EDGE ( 'NONE', *, *, #6542, .F. ) ;
#25989 = EDGE_CURVE ( 'NONE', #25893, #9814, #32867, .T. ) ;
#25990 = ADVANCED_FACE ( 'NONE', ( #42570 ), #33164, .T. ) ;
#25991 = CYLINDRICAL_SURFACE ( 'NONE', #29331, 0.1500000000000060729 ) ;
#25992 = CARTESIAN_POINT ( 'NONE',  ( -22.37985683132060188, -19.82347751554591397, 69.47417989525710880 ) ) ;
#25993 = AXIS2_PLACEMENT_3D ( 'NONE', #27914, #42937, #5522 ) ;
#25994 = CYLINDRICAL_SURFACE ( 'NONE', #22585, 0.1500000000000050182 ) ;
#25995 = ORIENTED_EDGE ( 'NONE', *, *, #11260, .F. ) ;
#25996 = DIRECTION ( 'NONE',  ( 3.071710424422018668E-17, -6.404604876783312462E-16, -1.000000000000000000 ) ) ;
#25997 =( BOUNDED_CURVE ( )  B_SPLINE_CURVE ( 3, ( #22644, #41109, #7394, #3938 ),
 .UNSPECIFIED., .F., .F. ) 
 B_SPLINE_CURVE_WITH_KNOTS ( ( 4, 4 ),
 ( 0.9074455897393646220, 1.000000000000000000 ),
 .UNSPECIFIED. ) 
 CURVE ( )  GEOMETRIC_REPRESENTATION_ITEM ( )  RATIONAL_B_SPLINE_CURVE ( ( 0.6983129098260778544, 0.7760317562606851016, 0.8765941196519925205, 1.000000000000000000 ) ) 
 REPRESENTATION_ITEM ( '' )  );
#25998 = ORIENTED_EDGE ( 'NONE', *, *, #46016, .F. ) ;
#25999 = FACE_OUTER_BOUND ( 'NONE', #41072, .T. ) ;
#26000 = DIRECTION ( 'NONE',  ( 0.9687793358424821033, -0.2479245821708677133, 0.000000000000000000 ) ) ;
#26001 = CARTESIAN_POINT ( 'NONE',  ( -9.995738443926455830, -14.24059931954510816, 64.50308448303212572 ) ) ;
#26002 = CIRCLE ( 'NONE', #44121, 5.500000000000000000 ) ;
#26003 = VERTEX_POINT ( 'NONE', #14647 ) ;
#26004 = CARTESIAN_POINT ( 'NONE',  ( -33.52409385541305653, -6.359206544744109735, 48.79999999999998295 ) ) ;
#26005 = LINE ( 'NONE', #18348, #39938 ) ;
#26006 = FACE_OUTER_BOUND ( 'NONE', #48463, .T. ) ;
#26007 = DIRECTION ( 'NONE',  ( 0.5562740912439652075, 0.8309988781043535777, 7.851267780903551505E-08 ) ) ;
#26008 = ORIENTED_EDGE ( 'NONE', *, *, #31173, .T. ) ;
#26009 = CARTESIAN_POINT ( 'NONE',  ( -15.69736356130078647, -8.025520047610617880, 70.90989840317035942 ) ) ;
#26010 = CARTESIAN_POINT ( 'NONE',  ( -12.57223699000811656, -19.85511602558925048, 65.16674893742153074 ) ) ;
#26011 = VERTEX_POINT ( 'NONE', #29467 ) ;
#26012 = FACE_BOUND ( 'NONE', #32532, .T. ) ;
#26013 = ORIENTED_EDGE ( 'NONE', *, *, #4240, .F. ) ;
#26014 = FACE_OUTER_BOUND ( 'NONE', #12846, .T. ) ;
#26016 = ADVANCED_FACE ( 'NONE', ( #21116 ), #25769, .T. ) ;
#26015 = LINE ( 'NONE', #3106, #36507 ) ;
#26017 = CARTESIAN_POINT ( 'NONE',  ( -24.42002265954547724, -14.56875473297011681, 62.72798972149294627 ) ) ;
#26018 = AXIS2_PLACEMENT_3D ( 'NONE', #47151, #2327, #24751 ) ;
#26019 = CARTESIAN_POINT ( 'NONE',  ( -21.61680475328812889, -8.650891705389904374, 73.85774703147257014 ) ) ;
#26020 = VERTEX_POINT ( 'NONE', #13932 ) ;
#26021 = CARTESIAN_POINT ( 'NONE',  ( -10.14660727810982976, -16.40665786317032371, 71.56094979796495181 ) ) ;
#26022 = ORIENTED_EDGE ( 'NONE', *, *, #34637, .F. ) ;
#26023 = DIRECTION ( 'NONE',  ( 5.551115123125782702E-17, 1.232595164407830946E-32, 1.000000000000000000 ) ) ;
#26024 = LINE ( 'NONE', #41043, #39268 ) ;
#26025 = ORIENTED_EDGE ( 'NONE', *, *, #46345, .F. ) ;
#26026 = CARTESIAN_POINT ( 'NONE',  ( -45.92409385541306222, -14.90920654474410867, 71.85000000000000853 ) ) ;
#26027 = AXIS2_PLACEMENT_3D ( 'NONE', #29748, #29996, #45031 ) ;
#26028 = CARTESIAN_POINT ( 'NONE',  ( -18.32857646159318676, -22.20418385865972155, 68.93019298464047040 ) ) ;
#26029 = ADVANCED_FACE ( 'NONE', ( #47463 ), #40788, .F. ) ;
#26030 = ORIENTED_EDGE ( 'NONE', *, *, #46365, .T. ) ;
#26031 = ORIENTED_EDGE ( 'NONE', *, *, #8199, .F. ) ;
#26032 = CARTESIAN_POINT ( 'NONE',  ( -27.42409385541305156, -15.80920654474410725, 47.99999999999997868 ) ) ;
#26033 = CARTESIAN_POINT ( 'NONE',  ( -22.24952096526922318, -19.88199321984651391, 69.40247773061638270 ) ) ;
#26034 = AXIS2_PLACEMENT_3D ( 'NONE', #44050, #29486, #18390 ) ;
#26035 = CARTESIAN_POINT ( 'NONE',  ( -12.56051219783612538, -20.45271961000943861, 71.85007761110178137 ) ) ;
#26036 = CARTESIAN_POINT ( 'NONE',  ( -10.04087064144442110, -13.81269952487260078, 57.58791698818001947 ) ) ;
#26037 = CARTESIAN_POINT ( 'NONE',  ( -11.55573786329523855, -10.21941616939416342, 71.15388509157428132 ) ) ;
#26038 = DIRECTION ( 'NONE',  ( 0.9979768094191903138, 0.06357898915123821881, 0.000000000000000000 ) ) ;
#26039 = CARTESIAN_POINT ( 'NONE',  ( -47.12338083056222615, -12.91120565595569580, 70.13000000000000966 ) ) ;
#26040 = ORIENTED_EDGE ( 'NONE', *, *, #31234, .T. ) ;
#26041 = EDGE_LOOP ( 'NONE', ( #12750, #36896 ) ) ;
#26042 = CARTESIAN_POINT ( 'NONE',  ( -15.93106588071581697, -7.910958181831522218, 60.35595345230024833 ) ) ;
#26043 = AXIS2_PLACEMENT_3D ( 'NONE', #39270, #10212, #20572 ) ;
#26044 = LINE ( 'NONE', #25072, #35399 ) ;
#26045 = CARTESIAN_POINT ( 'NONE',  ( -14.95256263785226203, -21.41194290305684333, 61.93040681845756268 ) ) ;
#26046 = DIRECTION ( 'NONE',  ( -5.731567514496413899E-31, -1.020425574103664789E-16, -1.000000000000000000 ) ) ;
#26047 = ORIENTED_EDGE ( 'NONE', *, *, #29602, .T. ) ;
#26048 = CARTESIAN_POINT ( 'NONE',  ( -16.22409385650551883, -6.426201560718813433, 50.50509628382439331 ) ) ;
#26049 = ADVANCED_FACE ( 'NONE', ( #17873 ), #22084, .T. ) ;
#26050 = ORIENTED_EDGE ( 'NONE', *, *, #16635, .F. ) ;
#26051 = VECTOR ( 'NONE', #45687, 1000.000000000000000 ) ;
#26052 = EDGE_CURVE ( 'NONE', #12496, #29452, #18356, .T. ) ;
#26053 = EDGE_CURVE ( 'NONE', #31211, #12927, #47694, .T. ) ;
#26054 = FACE_OUTER_BOUND ( 'NONE', #6226, .T. ) ;
#26055 = CARTESIAN_POINT ( 'NONE',  ( -11.86614749421525339, -19.77135288044581429, 58.11337654531251218 ) ) ;
#26056 = CIRCLE ( 'NONE', #16583, 4.686499999999999666 ) ;
#26057 = CARTESIAN_POINT ( 'NONE',  ( -16.87780900865216438, -10.15465445929086030, 52.02966884056656482 ) ) ;
#26058 = ORIENTED_EDGE ( 'NONE', *, *, #42506, .F. ) ;
#26059 = CARTESIAN_POINT ( 'NONE',  ( -45.92409385541306222, -14.20920654474410760, 70.50000000000000000 ) ) ;
#26060 = AXIS2_PLACEMENT_3D ( 'NONE', #11958, #19088, #37536 ) ;
#26061 = EDGE_CURVE ( 'NONE', #6771, #8867, #11183, .T. ) ;
#26062 = EDGE_CURVE ( 'NONE', #19139, #30521, #33717, .T. ) ;
#26063 = CARTESIAN_POINT ( 'NONE',  ( -14.98927377128279304, -8.246306944878790901, 75.49999999999994316 ) ) ;
#26064 = LINE ( 'NONE', #26297, #10721 ) ;
#26065 = EDGE_LOOP ( 'NONE', ( #32182, #4628 ) ) ;
#26066 = CIRCLE ( 'NONE', #43371, 4.686499999999998778 ) ;
#26067 = CARTESIAN_POINT ( 'NONE',  ( -22.46373187589079379, -16.28044704940516496, 49.52966884056655772 ) ) ;
#26068 = CARTESIAN_POINT ( 'NONE',  ( -21.89130958583942288, -9.354787850460871468, 63.20625856529903075 ) ) ;
#26069 = ORIENTED_EDGE ( 'NONE', *, *, #9645, .T. ) ;
#26070 = CARTESIAN_POINT ( 'NONE',  ( -24.68120957711303731, -16.49402054639926263, 59.30145216245190909 ) ) ;
#26071 = VERTEX_POINT ( 'NONE', #29711 ) ;
#26072 = CARTESIAN_POINT ( 'NONE',  ( -10.16749015965427105, -13.12235144340169235, 71.39323866028058774 ) ) ;
#26073 = CARTESIAN_POINT ( 'NONE',  ( -24.30574759568347787, -16.34084296935221303, 59.42332403323545265 ) ) ;
#26074 = ORIENTED_EDGE ( 'NONE', *, *, #22792, .F. ) ;
#26075 = CARTESIAN_POINT ( 'NONE',  ( -28.42409385541305511, -6.859206544744110623, 52.99999999999997158 ) ) ;
#26076 = EDGE_CURVE ( 'NONE', #6043, #3502, #36613, .T. ) ;
#26077 = CARTESIAN_POINT ( 'NONE',  ( -16.32575768948312600, -7.844986739114469643, 60.21500614002425777 ) ) ;
#26078 = ORIENTED_EDGE ( 'NONE', *, *, #13669, .T. ) ;
#26079 = DIRECTION ( 'NONE',  ( -0.3478314405900309048, -0.9375570856950864451, 0.000000000000000000 ) ) ;
#26080 =( BOUNDED_CURVE ( )  B_SPLINE_CURVE ( 3, ( #20768, #46201, #36257, #42269 ),
 .UNSPECIFIED., .F., .F. ) 
 B_SPLINE_CURVE_WITH_KNOTS ( ( 4, 4 ),
 ( 0.000000000000000000, 0.4074455897393662318 ),
 .UNSPECIFIED. ) 
 CURVE ( )  GEOMETRIC_REPRESENTATION_ITEM ( )  RATIONAL_B_SPLINE_CURVE ( ( 1.000000000000000000, 0.4567392136813269721, 0.3561768502900284350, 0.6983129098261046108 ) ) 
 REPRESENTATION_ITEM ( '' )  );
#26081 = DIRECTION ( 'NONE',  ( -3.413470714839332458E-33, 1.190614954331866791E-16, -1.000000000000000000 ) ) ;
#26082 = CARTESIAN_POINT ( 'NONE',  ( -18.34288178775629419, -10.21365315202000446, 49.52966884056655772 ) ) ;
#26083 = ORIENTED_EDGE ( 'NONE', *, *, #11527, .T. ) ;
#26084 = CYLINDRICAL_SURFACE ( 'NONE', #39667, 1.249999999999998668 ) ;
#26085 = CARTESIAN_POINT ( 'NONE',  ( -23.29491342820895028, -19.39590518005356756, 59.06223412631987912 ) ) ;
#26086 = AXIS2_PLACEMENT_3D ( 'NONE', #44780, #6845, #45265 ) ;
#26087 = CARTESIAN_POINT ( 'NONE',  ( -24.38556453292044424, -15.94620486698431350, 62.59328380657402846 ) ) ;
#26088 = ORIENTED_EDGE ( 'NONE', *, *, #18256, .F. ) ;
#26089 = ORIENTED_EDGE ( 'NONE', *, *, #5052, .F. ) ;
#26090 = AXIS2_PLACEMENT_3D ( 'NONE', #29054, #21905, #25367 ) ;
#26091 = CYLINDRICAL_SURFACE ( 'NONE', #12563, 0.1500000000000061562 ) ;
#26092 = CYLINDRICAL_SURFACE ( 'NONE', #47708, 1.249999999999998668 ) ;
#26093 = CARTESIAN_POINT ( 'NONE',  ( -15.35534385759798859, -8.623186033802571870, 49.24843789510467218 ) ) ;
#26094 = CARTESIAN_POINT ( 'NONE',  ( -23.83724620116612058, -11.87385095858915207, 63.36706934938042934 ) ) ;
#26095 = CARTESIAN_POINT ( 'NONE',  ( -24.11138715268779364, -17.05307659639229101, 69.41339812867973080 ) ) ;
#26096 = CARTESIAN_POINT ( 'NONE',  ( -16.96792471375929523, -7.373175173468426102, 74.05994646750021104 ) ) ;
#26097 = DIRECTION ( 'NONE',  ( -3.071710424422018668E-17, 6.404604876783312462E-16, 1.000000000000000000 ) ) ;
#26098 = ORIENTED_EDGE ( 'NONE', *, *, #36754, .T. ) ;
#26099 = CARTESIAN_POINT ( 'NONE',  ( -22.89146017634119090, -10.34570183799575105, 70.15611359559922278 ) ) ;
#26100 = VECTOR ( 'NONE', #37725, 1000.000000000000114 ) ;
#26101 = CARTESIAN_POINT ( 'NONE',  ( -14.98249323814573941, -9.880861343182303358, 53.49899999999994549 ) ) ;
#26102 = CARTESIAN_POINT ( 'NONE',  ( -16.52634554021970104, -22.20493084912042292, 65.32590148269446217 ) ) ;
#26103 = ORIENTED_EDGE ( 'NONE', *, *, #16275, .F. ) ;
#26104 = ORIENTED_EDGE ( 'NONE', *, *, #6688, .F. ) ;
#26105 = EDGE_CURVE ( 'NONE', #41118, #14238, #41622, .T. ) ;
#26106 = CARTESIAN_POINT ( 'NONE',  ( -36.42409385541304800, -8.109206544743658540, 50.50000000000030553 ) ) ;
#26107 = CARTESIAN_POINT ( 'NONE',  ( -10.62264718916325279, -13.15334866428350047, 71.20828630685304006 ) ) ;
#26108 = FACE_OUTER_BOUND ( 'NONE', #14200, .T. ) ;
#26109 = CARTESIAN_POINT ( 'NONE',  ( -13.82494607736302683, -21.33227806808298865, 72.10420475123025597 ) ) ;
#26110 = ORIENTED_EDGE ( 'NONE', *, *, #42657, .F. ) ;
#26111 = LINE ( 'NONE', #7406, #36856 ) ;
#26112 = EDGE_CURVE ( 'NONE', #14380, #21441, #19372, .T. ) ;
#26113 = EDGE_CURVE ( 'NONE', #42055, #30264, #19991, .T. ) ;
#26114 = DIRECTION ( 'NONE',  ( -0.3126464228004096069, -0.3197690014840522399, 0.8944271909999157444 ) ) ;
#26115 = ORIENTED_EDGE ( 'NONE', *, *, #23970, .T. ) ;
#26116 = ADVANCED_FACE ( 'NONE', ( #26759 ), #4872, .T. ) ;
#26117 = CIRCLE ( 'NONE', #41062, 2.499999999999999556 ) ;
#26118 = DIRECTION ( 'NONE',  ( 1.000000000000000000, -0.000000000000000000, 2.081668171172170091E-15 ) ) ;
#26119 = EDGE_CURVE ( 'NONE', #8183, #11393, #182, .T. ) ;
#26120 =( BOUNDED_CURVE ( )  B_SPLINE_CURVE ( 3, ( #41786, #10758, #25780, #4127 ),
 .UNSPECIFIED., .F., .F. ) 
 B_SPLINE_CURVE_WITH_KNOTS ( ( 4, 4 ),
 ( 0.5000000000000000000, 0.9074455897393678416 ),
 .UNSPECIFIED. ) 
 CURVE ( )  GEOMETRIC_REPRESENTATION_ITEM ( )  RATIONAL_B_SPLINE_CURVE ( ( 1.000000000000018430, 0.4567392136813228642, 0.3561768502900140021, 0.6983129098261117162 ) ) 
 REPRESENTATION_ITEM ( '' )  );
#26121 = CARTESIAN_POINT ( 'NONE',  ( -21.94239013569476171, -20.22099906679998327, 58.76442899523448204 ) ) ;
#26122 = ORIENTED_EDGE ( 'NONE', *, *, #47727, .T. ) ;
#26123 = DIRECTION ( 'NONE',  ( -0.000000000000000000, -1.000000000000000000, -0.000000000000000000 ) ) ;
#26124 = ORIENTED_EDGE ( 'NONE', *, *, #6694, .F. ) ;
#26125 = DIRECTION ( 'NONE',  ( 1.140458104654002173E-06, 1.256740833599404314E-06, -0.9999999999985599297 ) ) ;
#26126 = LINE ( 'NONE', #21222, #28167 ) ;
#26127 = ORIENTED_EDGE ( 'NONE', *, *, #2032, .T. ) ;
#26128 = CARTESIAN_POINT ( 'NONE',  ( -16.36339736119901289, -21.78261100941413986, 65.31744608471964852 ) ) ;
#26129 = FACE_OUTER_BOUND ( 'NONE', #2035, .T. ) ;
#26130 = EDGE_CURVE ( 'NONE', #11361, #31233, #23532, .T. ) ;
#26131 = CARTESIAN_POINT ( 'NONE',  ( -19.85534385650552025, -7.417179338643134834, 52.18511593390279302 ) ) ;
#26132 = CARTESIAN_POINT ( 'NONE',  ( -17.68496328886486424, -21.80445416477857279, 58.70553376440283699 ) ) ;
#26133 = CARTESIAN_POINT ( 'NONE',  ( -24.86242989439883289, -14.39095395922188558, 66.36788051138485400 ) ) ;
#26134 = DIRECTION ( 'NONE',  ( -3.071710424422018668E-17, 6.404604876783312462E-16, 1.000000000000000000 ) ) ;
#26135 = CARTESIAN_POINT ( 'NONE',  ( -10.23610968374255314, -12.85046669463587143, 67.85336945107273721 ) ) ;
#26136 = ORIENTED_EDGE ( 'NONE', *, *, #19866, .F. ) ;
#26138 = CARTESIAN_POINT ( 'NONE',  ( -16.98230468507255253, -22.24614900656091621, 72.35817375816297670 ) ) ;
#26137 =( BOUNDED_SURFACE ( )  B_SPLINE_SURFACE ( 3, 1, ( 
 ( #20525, #32083 ),
 ( #6223, #12874 ),
 ( #2038, #27901 ),
 ( #42926, #43665 ),
 ( #24216, #5507 ),
 ( #1802, #28145 ),
 ( #5754, #35756 ) ),
 .UNSPECIFIED., .T., .F., .F. ) 
 B_SPLINE_SURFACE_WITH_KNOTS ( ( 4, 3, 4 ),
 ( 2, 2 ),
 ( 0.000000000000000000, 0.5000000000000000000, 1.000000000000000000 ),
 ( 0.000000000000000000, 1.000000000000000000 ),
 .UNSPECIFIED. ) 
 GEOMETRIC_REPRESENTATION_ITEM ( )  RATIONAL_B_SPLINE_SURFACE ( (
 ( 1.000000000000000000, 1.000000000000000000),
 ( 0.3333333333333335369, 0.3333333333333330373),
 ( 0.3333333333333335369, 0.3333333333333330373),
 ( 1.000000000000000000, 1.000000000000000000),
 ( 0.3333333333333333703, 0.3333333333333333703),
 ( 0.3333333333333333703, 0.3333333333333333703),
 ( 1.000000000000000000, 1.000000000000000000) ) ) 
 REPRESENTATION_ITEM ( '' )  SURFACE ( )  );
#26139 = DIRECTION ( 'NONE',  ( 0.9687793358424819923, -0.2479245821708680464, 0.000000000000000000 ) ) ;
#26140 = CARTESIAN_POINT ( 'NONE',  ( -13.18473975798692877, -20.93551490194142062, 58.23145353898504339 ) ) ;
#26141 = DIRECTION ( 'NONE',  ( -0.9524241471993249997, -0.0009228828802096092788, 0.3047743298226210373 ) ) ;
#26142 = CARTESIAN_POINT ( 'NONE',  ( -17.42409385541300892, -14.80920654474439679, 47.99999999999994316 ) ) ;
#26143 = CARTESIAN_POINT ( 'NONE',  ( -17.20139284005516700, -7.812749994621428051, 70.79035839633094440 ) ) ;
#26144 = ORIENTED_EDGE ( 'NONE', *, *, #25558, .T. ) ;
#26145 = EDGE_LOOP ( 'NONE', ( #6289, #48315, #4386, #40016, #33363 ) ) ;
#26146 = CARTESIAN_POINT ( 'NONE',  ( -23.62594491300536959, -11.45603751788689095, 66.70742424642772050 ) ) ;
#26147 = CARTESIAN_POINT ( 'NONE',  ( -21.57946453887431204, -8.565578233975859490, 53.49999999999994316 ) ) ;
#26148 = ORIENTED_EDGE ( 'NONE', *, *, #954, .T. ) ;
#26150 = CARTESIAN_POINT ( 'NONE',  ( -24.00746416177546294, -17.19188300715374140, 72.95506251513478446 ) ) ;
#26149 = CARTESIAN_POINT ( 'NONE',  ( -15.33646109947928338, -7.657507462184680591, 74.24018999459609347 ) ) ;
#26151 = DIRECTION ( 'NONE',  ( -3.071710424422018668E-17, 6.404604876783312462E-16, 1.000000000000000000 ) ) ;
#26152 = CARTESIAN_POINT ( 'NONE',  ( -11.82099749022622426, -9.899105802180386604, 64.21409645106085406 ) ) ;
#26153 = CARTESIAN_POINT ( 'NONE',  ( -24.74223048688043747, -16.20536452925702520, 62.77045531336093376 ) ) ;
#26154 = CARTESIAN_POINT ( 'NONE',  ( -24.32886716615087153, -16.23426984194678724, 62.60800820172418923 ) ) ;
#26155 = CARTESIAN_POINT ( 'NONE',  ( -19.51575165005438706, -21.95960923578041957, 62.10229500050338203 ) ) ;
#26156 = CARTESIAN_POINT ( 'NONE',  ( -22.53429316287767392, -9.952421288698296564, 73.63161091678163928 ) ) ;
#26157 =( BOUNDED_CURVE ( )  B_SPLINE_CURVE ( 3, ( #19622, #15912, #37340, #34632 ),
 .UNSPECIFIED., .F., .F. ) 
 B_SPLINE_CURVE_WITH_KNOTS ( ( 4, 4 ),
 ( 0.9074455897393781667, 1.000000000000000000 ),
 .UNSPECIFIED. ) 
 CURVE ( )  GEOMETRIC_REPRESENTATION_ITEM ( )  RATIONAL_B_SPLINE_CURVE ( ( 0.6983129098261450229, 0.7760317562607430553, 0.8765941196520280476, 1.000000000000000000 ) ) 
 REPRESENTATION_ITEM ( '' )  );
#26158 = CARTESIAN_POINT ( 'NONE',  ( -16.26195973558533581, -21.76306465430365122, 58.57113428431811997 ) ) ;
#26159 = CARTESIAN_POINT ( 'NONE',  ( -18.77402089607887348, -7.482479170000134516, 70.47729698164395984 ) ) ;
#26160 = ORIENTED_EDGE ( 'NONE', *, *, #23198, .F. ) ;
#26161 = CARTESIAN_POINT ( 'NONE',  ( -24.08907074505709645, -11.48026357735065872, 63.13713704106291402 ) ) ;
#26162 = CARTESIAN_POINT ( 'NONE',  ( -12.81450749931373423, -9.474957484202729319, 74.31923006089488126 ) ) ;
#26163 = ADVANCED_BREP_SHAPE_REPRESENTATION ( '', ( #14655, #29031 ), #29815 ) ;
#26164 = DIRECTION ( 'NONE',  ( -3.071710424422018668E-17, 6.404604876783312462E-16, 1.000000000000000000 ) ) ;
#26165 = CARTESIAN_POINT ( 'NONE',  ( -24.29423998123223782, -13.46050165329320336, 59.59097898989885067 ) ) ;
#26166 = CARTESIAN_POINT ( 'NONE',  ( -24.63461978062257174, -12.93251252767717929, 66.48902111634848211 ) ) ;
#26167 = EDGE_CURVE ( 'NONE', #21252, #29761, #23977, .T. ) ;
#26168 = CARTESIAN_POINT ( 'NONE',  ( -11.60526899143904345, -18.79015832504765626, 68.23161775275829655 ) ) ;
#26169 = FACE_OUTER_BOUND ( 'NONE', #27207, .T. ) ;
#26170 = VERTEX_POINT ( 'NONE', #48664 ) ;
#26171 = VERTEX_POINT ( 'NONE', #29964 ) ;
#26172 = CARTESIAN_POINT ( 'NONE',  ( -20.96187357126569850, -17.88286835634646721, 49.52966884056655772 ) ) ;
#26173 = VERTEX_POINT ( 'NONE', #26507 ) ;
#26174 = EDGE_CURVE ( 'NONE', #36726, #29955, #22830, .T. ) ;
#26175 = CARTESIAN_POINT ( 'NONE',  ( -16.32575768948312600, -7.844986739114469643, 60.21500614002425777 ) ) ;
#26176 = CARTESIAN_POINT ( 'NONE',  ( -10.03016176022630646, -13.89628074529801438, 57.49179087295118507 ) ) ;
#26177 = ORIENTED_EDGE ( 'NONE', *, *, #4784, .F. ) ;
#26178 = B_SPLINE_CURVE_WITH_KNOTS ( 'NONE', 1,
 ( #4179, #3930 ),
 .UNSPECIFIED., .F., .F.,
 ( 2, 2 ),
 ( 0.000000000000000000, 1.000000000000000000 ),
 .UNSPECIFIED. ) ;
#26179 = EDGE_CURVE ( 'NONE', #6465, #33214, #37824, .T. ) ;
#26180 = CARTESIAN_POINT ( 'NONE',  ( -13.47245494993759607, -21.12492725511472003, 65.10133600691351319 ) ) ;
#26181 = CARTESIAN_POINT ( 'NONE',  ( -19.61601425152793254, -21.50980239257335569, 65.61486213821591207 ) ) ;
#26182 = EDGE_CURVE ( 'NONE', #1645, #2748, #46381, .T. ) ;
#26183 = ORIENTED_EDGE ( 'NONE', *, *, #21501, .F. ) ;
#26184 = CARTESIAN_POINT ( 'NONE',  ( -22.38400322090610217, -20.36826016184844335, 62.41934579407823236 ) ) ;
#26185 = CARTESIAN_POINT ( 'NONE',  ( -23.93808066934879619, -17.37550490234871248, 69.64169580580271202 ) ) ;
#26186 = ORIENTED_EDGE ( 'NONE', *, *, #15531, .F. ) ;
#26187 = EDGE_CURVE ( 'NONE', #35729, #17425, #15395, .T. ) ;
#26188 = FACE_OUTER_BOUND ( 'NONE', #3714, .T. ) ;
#26189 = CARTESIAN_POINT ( 'NONE',  ( -19.86401518824997581, -21.42384811948916479, 69.22010401872219632 ) ) ;
#26190 = CARTESIAN_POINT ( 'NONE',  ( -22.91943239076679006, -10.38811108791941429, 59.48714571049892896 ) ) ;
#26191 = VERTEX_POINT ( 'NONE', #11735 ) ;
#26192 = CARTESIAN_POINT ( 'NONE',  ( -11.05034076241727625, -11.79557573020262318, 71.37388789199357575 ) ) ;
#26193 = DIRECTION ( 'NONE',  ( -4.115385489419834196E-17, -0.9999954153791273948, -0.003028072113822188795 ) ) ;
#26194 = EDGE_CURVE ( 'NONE', #1223, #17754, #18215, .T. ) ;
#26195 = CARTESIAN_POINT ( 'NONE',  ( -10.31364510401727053, -17.03300888149450998, 57.80265138661536639 ) ) ;
#26196 = CARTESIAN_POINT ( 'NONE',  ( -9.982716954774490503, -14.44908413001617298, 67.97304700561097945 ) ) ;
#26197 = VERTEX_POINT ( 'NONE', #38979 ) ;
#26198 = CARTESIAN_POINT ( 'NONE',  ( -9.981610056738364989, -14.47448034074775336, 68.05811324665165785 ) ) ;
#26199 = CARTESIAN_POINT ( 'NONE',  ( -9.975093145215874202, -14.93635225021824198, 74.98274299234972773 ) ) ;
#26200 = CARTESIAN_POINT ( 'NONE',  ( -16.61483489837897309, -21.81624168220134052, 61.96387868409816946 ) ) ;
#26201 = CARTESIAN_POINT ( 'NONE',  ( -21.06159385650551741, -9.295667164867525756, 49.30633214617472504 ) ) ;
#26202 = ORIENTED_EDGE ( 'NONE', *, *, #32128, .T. ) ;
#26203 = CARTESIAN_POINT ( 'NONE',  ( -17.69364751199190522, -22.25449563392884400, 58.56699864565176483 ) ) ;
#26204 = CARTESIAN_POINT ( 'NONE',  ( -45.36595154876284397, -14.19714313411803985, 70.47802965039466017 ) ) ;
#26205 = EDGE_LOOP ( 'NONE', ( #25948, #38342 ) ) ;
#26206 = CARTESIAN_POINT ( 'NONE',  ( -18.39063358449543983, -7.876195807596681142, 73.91352353256114327 ) ) ;
#26207 = CARTESIAN_POINT ( 'NONE',  ( -24.55871722839809834, -12.66422925090921225, 69.88747596251579353 ) ) ;
#26208 = FACE_OUTER_BOUND ( 'NONE', #34023, .T. ) ;
#26209 = EDGE_LOOP ( 'NONE', ( #43701, #45598, #44046, #41936, #3217 ) ) ;
#26210 = DIRECTION ( 'NONE',  ( -0.9629498065864428025, -0.2696806815386155742, -3.246020392366887627E-17 ) ) ;
#26211 = LINE ( 'NONE', #45423, #41678 ) ;
#26212 = ORIENTED_EDGE ( 'NONE', *, *, #7788, .T. ) ;
#26213 = AXIS2_PLACEMENT_3D ( 'NONE', #23777, #26482, #38530 ) ;
#26214 = CARTESIAN_POINT ( 'NONE',  ( -13.24284385650551599, -8.811426318492348031, 52.18089403414752070 ) ) ;
#26215 = CARTESIAN_POINT ( 'NONE',  ( -10.96024275427387984, -11.10349598290784989, 60.79230391164892211 ) ) ;
#26216 = DIRECTION ( 'NONE',  ( 3.071710424422018668E-17, -6.404604876783312462E-16, -1.000000000000000000 ) ) ;
#26217 = EDGE_CURVE ( 'NONE', #12496, #46961, #26024, .T. ) ;
#26218 = CARTESIAN_POINT ( 'NONE',  ( -24.85472652781555070, -14.27003188481730689, 69.79241900681766708 ) ) ;
#26219 = CARTESIAN_POINT ( 'NONE',  ( -15.50784526261009511, -8.076599967007890513, 74.37985659287807039 ) ) ;
#26220 = ORIENTED_EDGE ( 'NONE', *, *, #29490, .T. ) ;
#26221 = VERTEX_POINT ( 'NONE', #7323 ) ;
#26222 = CARTESIAN_POINT ( 'NONE',  ( -13.07679657469475032, -8.645136888763005345, 48.52585319722742696 ) ) ;
#26223 = CARTESIAN_POINT ( 'NONE',  ( -10.45134696456191392, -14.19143820756648644, 60.93323705330102058 ) ) ;
#26224 = DIRECTION ( 'NONE',  ( 0.000000000000000000, -0.9999954153791273948, -0.003028072113819838245 ) ) ;
#26225 = CARTESIAN_POINT ( 'NONE',  ( -14.39909385650551776, -8.114302828567740988, 52.18300498402516041 ) ) ;
#26226 = VERTEX_POINT ( 'NONE', #22324 ) ;
#26227 = CARTESIAN_POINT ( 'NONE',  ( -24.80769062643263467, -15.80232089486973557, 69.71802876059763321 ) ) ;
#26228 = ADVANCED_FACE ( 'NONE', ( #37563 ), #30219, .T. ) ;
#26229 = CARTESIAN_POINT ( 'NONE',  ( -18.86946249347487381, -7.959927237300316705, 67.20071732990344060 ) ) ;
#26230 = CARTESIAN_POINT ( 'NONE',  ( -24.77723895724858494, -16.00713575449774595, 66.24820309305337673 ) ) ;
#26231 = ORIENTED_EDGE ( 'NONE', *, *, #8686, .F. ) ;
#26232 = CARTESIAN_POINT ( 'NONE',  ( -12.32278866559117780, -19.67576434477648917, 61.41150688479135766 ) ) ;
#26233 = ORIENTED_EDGE ( 'NONE', *, *, #36867, .F. ) ;
#26234 = EDGE_CURVE ( 'NONE', #20100, #8067, #24089, .T. ) ;
#26235 = CARTESIAN_POINT ( 'NONE',  ( -10.38752013045322009, -14.36951432065623813, 64.67331771650336236 ) ) ;
#26236 = CARTESIAN_POINT ( 'NONE',  ( -19.60046948880987117, -21.46228020301366257, 65.76486213989072382 ) ) ;
#26237 = LINE ( 'NONE', #7536, #30765 ) ;
#26238 = CARTESIAN_POINT ( 'NONE',  ( -21.52687325878983415, -21.02790335591837589, 72.68592979288212064 ) ) ;
#26239 = AXIS2_PLACEMENT_3D ( 'NONE', #35503, #32310, #24445 ) ;
#26240 = VERTEX_POINT ( 'NONE', #24704 ) ;
#26241 = CARTESIAN_POINT ( 'NONE',  ( -17.85728874018075985, -21.84618329174708151, 61.89007996730683203 ) ) ;
#26242 = ADVANCED_FACE ( 'NONE', ( #32333 ), #9688, .T. ) ;
#26243 = CYLINDRICAL_SURFACE ( 'NONE', #4622, 0.1499999999999999667 ) ;
#26244 = DIRECTION ( 'NONE',  ( -3.071710424422018668E-17, 6.404604876783312462E-16, 1.000000000000000000 ) ) ;
#26245 = ORIENTED_EDGE ( 'NONE', *, *, #17013, .T. ) ;
#26246 = DIRECTION ( 'NONE',  ( 0.000000000000000000, 0.000000000000000000, -1.000000000000000000 ) ) ;
#26247 = CARTESIAN_POINT ( 'NONE',  ( -21.80947398209100285, -9.353160252369512762, 63.49153755919518005 ) ) ;
#26248 = CARTESIAN_POINT ( 'NONE',  ( -36.42409385541304800, -8.109206544743658540, 50.50000000000030553 ) ) ;
#26249 = FACE_BOUND ( 'NONE', #15355, .T. ) ;
#26250 = ORIENTED_EDGE ( 'NONE', *, *, #7513, .F. ) ;
#26251 = CARTESIAN_POINT ( 'NONE',  ( -13.11436666535386664, -20.88631628731643630, 58.18616748667333383 ) ) ;
#26252 = CARTESIAN_POINT ( 'NONE',  ( -13.97409385541301496, -6.859212275519754876, 50.50378509014287687 ) ) ;
#26253 = CARTESIAN_POINT ( 'NONE',  ( -19.24025795797341942, -7.996846695050864540, 60.24620885950562865 ) ) ;
#26254 = DIRECTION ( 'NONE',  ( -0.9968684284758858594, 0.07907803935364896009, -1.831731158650941667E-08 ) ) ;
#26255 = VERTEX_POINT ( 'NONE', #21245 ) ;
#26256 = CARTESIAN_POINT ( 'NONE',  ( -10.11824992584547545, -16.26811798947522192, 71.56255103782838489 ) ) ;
#26257 = VERTEX_POINT ( 'NONE', #46628 ) ;
#26258 = CARTESIAN_POINT ( 'NONE',  ( -12.67990993908946429, -9.064901105426571348, 70.97112579386727305 ) ) ;
#26259 = CARTESIAN_POINT ( 'NONE',  ( -36.42409385541304800, -8.109206544743658540, 50.50000000000030553 ) ) ;
#26261 = ADVANCED_FACE ( 'NONE', ( #47358 ), #40197, .T. ) ;
#26260 = CARTESIAN_POINT ( 'NONE',  ( -14.41428275390769365, -7.994163218335415877, 63.97474169571218283 ) ) ;
#26262 = EDGE_LOOP ( 'NONE', ( #2994, #6176 ) ) ;
#26263 = CARTESIAN_POINT ( 'NONE',  ( -16.16379449968008331, -22.15191876840708929, 58.47080954035841671 ) ) ;
#26264 = EDGE_CURVE ( 'NONE', #26764, #30116, #5974, .T. ) ;
#26265 = CARTESIAN_POINT ( 'NONE',  ( -10.95381480682210373, -17.48044017699314523, 68.09721944380058289 ) ) ;
#26266 = VERTEX_POINT ( 'NONE', #2037 ) ;
#26267 = ADVANCED_FACE ( 'NONE', ( #20523 ), #24933, .T. ) ;
#26268 = EDGE_LOOP ( 'NONE', ( #13983, #29091, #41604, #3872 ) ) ;
#26269 = VERTEX_POINT ( 'NONE', #36000 ) ;
#26270 = CARTESIAN_POINT ( 'NONE',  ( -15.25801600794807555, -21.93814553200309092, 72.23230793488828283 ) ) ;
#26271 = DIRECTION ( 'NONE',  ( 1.027096116490394736E-05, 2.598167872976484874E-06, 0.9999999999438784481 ) ) ;
#26272 = CARTESIAN_POINT ( 'NONE',  ( -19.31443854130040449, -22.01544605587237768, 58.63233246516547581 ) ) ;
#26273 = CARTESIAN_POINT ( 'NONE',  ( -10.59838470211619565, -13.25112858161469021, 74.74987944841035414 ) ) ;
#26274 =( BOUNDED_SURFACE ( )  B_SPLINE_SURFACE ( 3, 1, ( 
 ( #9727, #17804 ),
 ( #24747, #36289 ),
 ( #2571, #40712 ),
 ( #32604, #6987 ),
 ( #39749, #33063 ),
 ( #25460, #13861 ),
 ( #40470, #6748 ) ),
 .UNSPECIFIED., .T., .F., .F. ) 
 B_SPLINE_SURFACE_WITH_KNOTS ( ( 4, 3, 4 ),
 ( 2, 2 ),
 ( 0.000000000000000000, 0.5000000000000000000, 1.000000000000000000 ),
 ( 0.000000000000000000, 1.000000000000000000 ),
 .UNSPECIFIED. ) 
 GEOMETRIC_REPRESENTATION_ITEM ( )  RATIONAL_B_SPLINE_SURFACE ( (
 ( 1.000000000000000000, 1.000000000000000000),
 ( 0.3333333333333335369, 0.3333333333333330373),
 ( 0.3333333333333335369, 0.3333333333333330373),
 ( 1.000000000000000000, 1.000000000000000000),
 ( 0.3333333333333333703, 0.3333333333333333703),
 ( 0.3333333333333333703, 0.3333333333333333703),
 ( 1.000000000000000000, 1.000000000000000000) ) ) 
 REPRESENTATION_ITEM ( '' )  SURFACE ( )  );
#26275 = CARTESIAN_POINT ( 'NONE',  ( -24.13143191548659416, -12.80630458298108110, 66.41132680564976454 ) ) ;
#26276 = CARTESIAN_POINT ( 'NONE',  ( -17.26958401828953171, -19.65204229739824626, 52.02966884056656482 ) ) ;
#26277 = CARTESIAN_POINT ( 'NONE',  ( -20.21784385541269558, -6.860780111193637509, 51.02154966934593006 ) ) ;
#26278 = ORIENTED_EDGE ( 'NONE', *, *, #9613, .F. ) ;
#26279 = ORIENTED_EDGE ( 'NONE', *, *, #23820, .F. ) ;
#26280 = VECTOR ( 'NONE', #32089, 1000.000000000000000 ) ;
#26281 = CARTESIAN_POINT ( 'NONE',  ( -12.18170072908086965, -10.17053062278287889, 64.32914326641392222 ) ) ;
#26282 = AXIS2_PLACEMENT_3D ( 'NONE', #42003, #4104, #19103 ) ;
#26283 = CARTESIAN_POINT ( 'NONE',  ( -10.97897535230521449, -21.25982559335476552, 54.49999999999995026 ) ) ;
#26284 = CARTESIAN_POINT ( 'NONE',  ( -21.87050360319829778, -9.402213735156793817, 63.20770402078916561 ) ) ;
#26285 = CARTESIAN_POINT ( 'NONE',  ( -18.55203529891204539, -7.444959873133314865, 74.01781259684146619 ) ) ;
#26286 = EDGE_LOOP ( 'NONE', ( #38397, #13412, #25109, #27759 ) ) ;
#26287 = CARTESIAN_POINT ( 'NONE',  ( -14.08659385650551776, -9.302874398569244363, 51.68646062012417985 ) ) ;
#26288 =( BOUNDED_CURVE ( )  B_SPLINE_CURVE ( 3, ( #34943, #43068, #27322, #20175 ),
 .UNSPECIFIED., .F., .F. ) 
 B_SPLINE_CURVE_WITH_KNOTS ( ( 4, 4 ),
 ( 0.9074455897393710613, 1.000000000000000000 ),
 .UNSPECIFIED. ) 
 CURVE ( )  GEOMETRIC_REPRESENTATION_ITEM ( )  RATIONAL_B_SPLINE_CURVE ( ( 0.6983129098261089407, 0.7760317562607119690, 0.8765941196520089518, 1.000000000000000000 ) ) 
 REPRESENTATION_ITEM ( '' )  );
#26289 = EDGE_LOOP ( 'NONE', ( #47373, #33629 ) ) ;
#26290 = CARTESIAN_POINT ( 'NONE',  ( -19.94733193681641481, -19.41309290135173526, 50.77966884056656482 ) ) ;
#26291 = CARTESIAN_POINT ( 'NONE',  ( -12.72364920584387349, -9.064356868646193277, 49.69365772853683438 ) ) ;
#26292 = CARTESIAN_POINT ( 'NONE',  ( -10.02995829593802668, -13.89786868041111667, 57.63320316755233819 ) ) ;
#26293 = ORIENTED_EDGE ( 'NONE', *, *, #6660, .F. ) ;
#26294 = CARTESIAN_POINT ( 'NONE',  ( -17.42409385541305511, -14.80920654474410725, 52.21286476528345588 ) ) ;
#26295 = EDGE_CURVE ( 'NONE', #29883, #10137, #6470, .T. ) ;
#26296 = CARTESIAN_POINT ( 'NONE',  ( -24.17913852840423417, -12.79079990135933897, 69.77802802196565324 ) ) ;
#26297 = CARTESIAN_POINT ( 'NONE',  ( -24.72409385541305582, -14.80920654474421205, 67.95882352941174531 ) ) ;
#26298 = VERTEX_POINT ( 'NONE', #46861 ) ;
#26299 = DIRECTION ( 'NONE',  ( -5.468526094916624094E-08, -8.832527036150760808E-06, 0.9999999999609917589 ) ) ;
#26300 = CARTESIAN_POINT ( 'NONE',  ( -10.13399043377362929, -16.34501826020601811, 71.56937588126346839 ) ) ;
#26301 = CARTESIAN_POINT ( 'NONE',  ( -24.37121093718953446, -17.50201705633955740, 66.05701994492248730 ) ) ;
#26302 = VERTEX_POINT ( 'NONE', #16800 ) ;
#26303 = CARTESIAN_POINT ( 'NONE',  ( -11.18894271684748887, -11.62402355859291170, 71.27787913046262247 ) ) ;
#26304 = ORIENTED_EDGE ( 'NONE', *, *, #22106, .F. ) ;
#26305 = AXIS2_PLACEMENT_3D ( 'NONE', #18887, #36842, #48429 ) ;
#26306 = CARTESIAN_POINT ( 'NONE',  ( -10.30929367908409766, -17.01932638214790927, 57.82727192363577018 ) ) ;
#26307 = CARTESIAN_POINT ( 'NONE',  ( -17.50221816081645798, -7.047512361584055363, 53.27966884056655061 ) ) ;
#26308 = EDGE_LOOP ( 'NONE', ( #14934, #31283, #29430, #45184 ) ) ;
#26309 = FACE_OUTER_BOUND ( 'NONE', #23302, .T. ) ;
#26310 = VECTOR ( 'NONE', #40540, 1000.000000000000114 ) ;
#26311 = CARTESIAN_POINT ( 'NONE',  ( -18.55725912610375516, -22.17253639328876602, 72.38536699639935534 ) ) ;
#26312 = ORIENTED_EDGE ( 'NONE', *, *, #42506, .T. ) ;
#26313 = CARTESIAN_POINT ( 'NONE',  ( -22.09944621541271914, -9.008888719317940996, 63.39164957891247099 ) ) ;
#26314 = CARTESIAN_POINT ( 'NONE',  ( -22.30100230481251344, -19.83081991958632884, 65.77709836140900279 ) ) ;
#26315 = CARTESIAN_POINT ( 'NONE',  ( -11.99471263755300576, -9.707784190782769329, 60.65943832103737776 ) ) ;
#26316 = ORIENTED_EDGE ( 'NONE', *, *, #28234, .F. ) ;
#26317 = CARTESIAN_POINT ( 'NONE',  ( -17.36015840614627592, -7.359395087992972151, 67.20535029649403214 ) ) ;
#26318 = EDGE_CURVE ( 'NONE', #41394, #33214, #47014, .T. ) ;
#26319 = CARTESIAN_POINT ( 'NONE',  ( -21.79482124383139308, -8.775876708292097206, 70.30945321915166346 ) ) ;
#26320 = PLANE ( 'NONE',  #6696 ) ;
#26321 = ADVANCED_FACE ( 'NONE', ( #2280 ), #23417, .T. ) ;
#26322 = ADVANCED_FACE ( 'NONE', ( #28144 ), #14891, .T. ) ;
#26323 = ORIENTED_EDGE ( 'NONE', *, *, #5799, .T. ) ;
#26324 = ORIENTED_EDGE ( 'NONE', *, *, #26179, .F. ) ;
#26325 = CARTESIAN_POINT ( 'NONE',  ( -22.37985709289073455, -19.82347726015160205, 69.17417989525732480 ) ) ;
#26326 = CARTESIAN_POINT ( 'NONE',  ( -10.16749015965427105, -13.12235144340169235, 71.39323866028058774 ) ) ;
#26327 = DIRECTION ( 'NONE',  ( 2.866981220435666553E-17, -1.000000000000000000, -1.190614954331866791E-16 ) ) ;
#26328 = CARTESIAN_POINT ( 'NONE',  ( -10.39215600595210631, -14.30487551902977827, 64.38803863383273551 ) ) ;
#26329 = CARTESIAN_POINT ( 'NONE',  ( -15.46784385759799285, -9.357632978295830739, 49.97845033065684106 ) ) ;
#26330 = CARTESIAN_POINT ( 'NONE',  ( -12.40380833417894912, -19.68739609921301792, 61.39678633575574906 ) ) ;
#26331 = CARTESIAN_POINT ( 'NONE',  ( -12.80135276601915528, -20.13603490024450693, 68.22168825917964341 ) ) ;
#26332 = CARTESIAN_POINT ( 'NONE',  ( -14.62409385759799108, -9.359200813967568422, 50.49621490985803263 ) ) ;
#26333 = FACE_OUTER_BOUND ( 'NONE', #13976, .T. ) ;
#26334 = ORIENTED_EDGE ( 'NONE', *, *, #38434, .T. ) ;
#26335 = CARTESIAN_POINT ( 'NONE',  ( -15.88655729437939534, -7.980152340574909076, 67.44007279406643818 ) ) ;
#26336 = FACE_OUTER_BOUND ( 'NONE', #38288, .T. ) ;
#26337 = CARTESIAN_POINT ( 'NONE',  ( -10.53536195276627829, -13.30851587854854579, 74.69289754060230280 ) ) ;
#26338 = ORIENTED_EDGE ( 'NONE', *, *, #27799, .F. ) ;
#26339 = VECTOR ( 'NONE', #29662, 1000.000000000000114 ) ;
#26340 = ORIENTED_EDGE ( 'NONE', *, *, #18573, .F. ) ;
#26341 = EDGE_CURVE ( 'NONE', #17056, #31648, #27049, .T. ) ;
#26342 = DIRECTION ( 'NONE',  ( 0.000000000000000000, 0.9999954153791273948, 0.003028072113820366902 ) ) ;
#26343 = AXIS2_PLACEMENT_3D ( 'NONE', #37816, #4111, #42253 ) ;
#26344 =( LENGTH_UNIT ( ) NAMED_UNIT ( * ) SI_UNIT ( .MILLI., .METRE. ) );
#26345 = CARTESIAN_POINT ( 'NONE',  ( -21.57940561823839332, -9.104090476609597360, 63.34720799502051847 ) ) ;
#26346 = CARTESIAN_POINT ( 'NONE',  ( -10.18733296281416045, -13.03881024611776418, 71.34795252663174381 ) ) ;
#26347 = VERTEX_POINT ( 'NONE', #18248 ) ;
#26348 = LINE ( 'NONE', #41618, #48650 ) ;
#26349 = DIRECTION ( 'NONE',  ( -3.071710424422018668E-17, 6.404604876783312462E-16, 1.000000000000000000 ) ) ;
#26350 = EDGE_CURVE ( 'NONE', #9970, #30992, #35052, .T. ) ;
#26351 = ORIENTED_EDGE ( 'NONE', *, *, #35650, .F. ) ;
#26352 = CARTESIAN_POINT ( 'NONE',  ( -21.84079810191280657, -9.314188493807273872, 63.49153755726583626 ) ) ;
#26353 = ADVANCED_FACE ( 'NONE', ( #18493 ), #29350, .T. ) ;
#26354 =( BOUNDED_CURVE ( )  B_SPLINE_CURVE ( 3, ( #21378, #2877, #36365, #10759 ),
 .UNSPECIFIED., .F., .F. ) 
 B_SPLINE_CURVE_WITH_KNOTS ( ( 4, 4 ),
 ( 0.9074455897393595150, 1.000000000000000000 ),
 .UNSPECIFIED. ) 
 CURVE ( )  GEOMETRIC_REPRESENTATION_ITEM ( )  RATIONAL_B_SPLINE_CURVE ( ( 0.6983129098260925094, 0.7760317562606977582, 0.8765941196520002920, 1.000000000000000000 ) ) 
 REPRESENTATION_ITEM ( '' )  );
#26355 = DIRECTION ( 'NONE',  ( -0.8743548079231422410, -0.4852872034802500067, 5.778319183281968808E-08 ) ) ;
#26356 = CARTESIAN_POINT ( 'NONE',  ( -10.85423594767881283, -17.22645656662391289, 64.64355980017001002 ) ) ;
#26357 = ORIENTED_EDGE ( 'NONE', *, *, #31434, .T. ) ;
#26358 = CARTESIAN_POINT ( 'NONE',  ( -19.98727432552137984, -8.241621372411282564, 74.02096606371280529 ) ) ;
#26359 = ORIENTED_EDGE ( 'NONE', *, *, #6611, .F. ) ;
#26360 = CARTESIAN_POINT ( 'NONE',  ( -10.44378636108426583, -17.41310671260886167, 64.78885870823729931 ) ) ;
#26361 = CARTESIAN_POINT ( 'NONE',  ( -12.35277332135121675, -20.26681466537264242, 68.45162004874669037 ) ) ;
#26362 = ORIENTED_EDGE ( 'NONE', *, *, #15766, .F. ) ;
#26363 = LINE ( 'NONE', #45591, #27791 ) ;
#26364 = CARTESIAN_POINT ( 'NONE',  ( -20.10740643985815268, -21.75925148913131579, 72.51204570001823413 ) ) ;
#26365 = CARTESIAN_POINT ( 'NONE',  ( -21.65534385650552096, -7.417179338643134834, 52.18511593390279302 ) ) ;
#26366 = FACE_OUTER_BOUND ( 'NONE', #31635, .T. ) ;
#26367 = CARTESIAN_POINT ( 'NONE',  ( -10.79553443930103285, -17.05933049762642639, 57.91433868669456331 ) ) ;
#26368 = CARTESIAN_POINT ( 'NONE',  ( -10.51874523558227636, -17.60584231662749843, 68.23688550535284492 ) ) ;
#26369 = CARTESIAN_POINT ( 'NONE',  ( -13.42765988558316792, -8.521637316299758069, 57.10934427942139280 ) ) ;
#26370 = VERTEX_POINT ( 'NONE', #2995 ) ;
#26371 = DIRECTION ( 'NONE',  ( 1.000000000000000000, -6.517531090241554163E-16, 3.534154189880001717E-15 ) ) ;
#26372 = CARTESIAN_POINT ( 'NONE',  ( -24.72409385541305582, -14.90920654474420104, 66.95294117647057419 ) ) ;
#26373 = FACE_OUTER_BOUND ( 'NONE', #1121, .T. ) ;
#26374 = LINE ( 'NONE', #11599, #25014 ) ;
#26375 = CARTESIAN_POINT ( 'NONE',  ( -18.67683868338968978, -7.922091914708606630, 70.67067976651917149 ) ) ;
#26376 = CARTESIAN_POINT ( 'NONE',  ( -23.77312771997254615, -18.70709664074277612, 72.87872845841107505 ) ) ;
#26377 = ADVANCED_FACE ( 'NONE', ( #40427 ), #44874, .T. ) ;
#26378 = EDGE_CURVE ( 'NONE', #11687, #36713, #17607, .T. ) ;
#26379 = ORIENTED_EDGE ( 'NONE', *, *, #33522, .T. ) ;
#26380 = EDGE_LOOP ( 'NONE', ( #7856, #14120, #4677, #45681, #772 ) ) ;
#26381 = CARTESIAN_POINT ( 'NONE',  ( -16.83291232462568132, -21.78581065439753317, 72.27616290343694061 ) ) ;
#26382 = CARTESIAN_POINT ( 'NONE',  ( -18.36828968083242231, -10.20659317963781021, 49.52966884056655772 ) ) ;
#26383 = ORIENTED_EDGE ( 'NONE', *, *, #37359, .T. ) ;
#26384 = CARTESIAN_POINT ( 'NONE',  ( -13.49459827716768423, -24.71111635512870208, 54.60745305979834541 ) ) ;
#26385 = CARTESIAN_POINT ( 'NONE',  ( -24.04646079654614255, -17.23801300935436132, 65.94357277538750850 ) ) ;
#26386 = CARTESIAN_POINT ( 'NONE',  ( -21.84079810191280657, -9.314188493807273872, 63.49153755726583626 ) ) ;
#26387 = CARTESIAN_POINT ( 'NONE',  ( -10.45984680026578495, -15.51639866492744169, 57.85327457721793110 ) ) ;
#26388 = CARTESIAN_POINT ( 'NONE',  ( -21.60384785555947929, -20.97637623824866182, 72.64633634696070885 ) ) ;
#26389 = CARTESIAN_POINT ( 'NONE',  ( -18.79049830835916524, -7.892586073225762000, 70.38540174208183942 ) ) ;
#26390 = DIRECTION ( 'NONE',  ( 0.000000000000000000, 0.000000000000000000, -1.000000000000000000 ) ) ;
#26391 = EDGE_CURVE ( 'NONE', #10333, #31013, #44771, .T. ) ;
#26392 = EDGE_CURVE ( 'NONE', #47754, #37645, #32789, .T. ) ;
#26393 = LINE ( 'NONE', #48550, #11023 ) ;
#26394 = CARTESIAN_POINT ( 'NONE',  ( -22.51726279860821478, -19.68384809141796765, 72.64400547081167758 ) ) ;
#26395 = CARTESIAN_POINT ( 'NONE',  ( -24.12697024258913103, -11.55706310638292500, 63.11364774580268033 ) ) ;
#26396 = CARTESIAN_POINT ( 'NONE',  ( -13.08575159502176177, -11.85263988192353324, 49.52966884056655772 ) ) ;
#26397 = EDGE_CURVE ( 'NONE', #897, #20341, #16197, .T. ) ;
#26398 = B_SPLINE_CURVE_WITH_KNOTS ( 'NONE', 3,
 ( #34010, #45126, #30350, #11611, #4238, #26643, #41658, #22963, #42393, #46329 ),
 .UNSPECIFIED., .F., .F.,
 ( 4, 2, 2, 2, 4 ),
 ( 0.6272669072782640631, 0.7522669073001383433, 0.8772669073220125124, 1.002266907343886793, 1.127266907365761073 ),
 .UNSPECIFIED. ) ;
#26399 = CARTESIAN_POINT ( 'NONE',  ( -15.58315248484016102, -8.055165849531416455, 74.36369132414399985 ) ) ;
#26400 = ADVANCED_FACE ( 'NONE', ( #47818 ), #24723, .T. ) ;
#26401 = CARTESIAN_POINT ( 'NONE',  ( -17.74207408025691279, -7.814823900549897395, 63.66130038185828255 ) ) ;
#26402 = CARTESIAN_POINT ( 'NONE',  ( -21.45534385541298406, -8.623186033802610950, 49.24843789510456560 ) ) ;
#26403 = PLANE ( 'NONE',  #3996 ) ;
#26404 = CARTESIAN_POINT ( 'NONE',  ( -18.32364513544568752, -21.80460793730824420, 65.23043427352648393 ) ) ;
#26405 = EDGE_LOOP ( 'NONE', ( #41155, #47169, #21801, #17897 ) ) ;
#26406 = EDGE_LOOP ( 'NONE', ( #5618, #9491, #46179, #18492, #25412 ) ) ;
#26407 = CARTESIAN_POINT ( 'NONE',  ( -15.54909385541304268, -8.112991634885936776, 51.74999426922421719 ) ) ;
#26408 = ORIENTED_EDGE ( 'NONE', *, *, #31951, .F. ) ;
#26409 = EDGE_CURVE ( 'NONE', #6140, #7043, #11469, .T. ) ;
#26410 = CARTESIAN_POINT ( 'NONE',  ( -23.55055098682252890, -19.04828202743015098, 66.01727754597818887 ) ) ;
#26411 = LINE ( 'NONE', #41422, #8789 ) ;
#26412 =( BOUNDED_CURVE ( )  B_SPLINE_CURVE ( 3, ( #27435, #1321, #8978, #12894 ),
 .UNSPECIFIED., .F., .F. ) 
 B_SPLINE_CURVE_WITH_KNOTS ( ( 4, 4 ),
 ( 0.5000000000000000000, 0.9074455897393632897 ),
 .UNSPECIFIED. ) 
 CURVE ( )  GEOMETRIC_REPRESENTATION_ITEM ( )  RATIONAL_B_SPLINE_CURVE ( ( 1.000000000000027534, 0.4567392136813411829, 0.3561768502900142797, 0.6983129098260767442 ) ) 
 REPRESENTATION_ITEM ( '' )  );
#26413 = AXIS2_PLACEMENT_3D ( 'NONE', #6483, #21506, #45622 ) ;
#26414 = CARTESIAN_POINT ( 'NONE',  ( -13.55534385759798965, -8.623186033802571870, 49.24843789510467218 ) ) ;
#26415 = CARTESIAN_POINT ( 'NONE',  ( -16.07945710171498988, -22.13702619746868905, 58.44732121985853723 ) ) ;
#26416 = ORIENTED_EDGE ( 'NONE', *, *, #2591, .F. ) ;
#26417 = CARTESIAN_POINT ( 'NONE',  ( -21.13745558015973103, -11.09794736473739718, 52.02966884056656482 ) ) ;
#26418 = CARTESIAN_POINT ( 'NONE',  ( -19.77436091090941517, -21.87886160397694368, 65.64981624214608757 ) ) ;
#26419 = ORIENTED_EDGE ( 'NONE', *, *, #16384, .T. ) ;
#26420 = CARTESIAN_POINT ( 'NONE',  ( -46.92409385541305511, -15.80920654474410725, 60.24999999999999289 ) ) ;
#26421 =( BOUNDED_CURVE ( )  B_SPLINE_CURVE ( 3, ( #16916, #30993, #39091, #20873 ),
 .UNSPECIFIED., .F., .F. ) 
 B_SPLINE_CURVE_WITH_KNOTS ( ( 4, 4 ),
 ( 0.9074455897393656212, 1.000000000000000000 ),
 .UNSPECIFIED. ) 
 CURVE ( )  GEOMETRIC_REPRESENTATION_ITEM ( )  RATIONAL_B_SPLINE_CURVE ( ( 0.6983129098260816292, 0.7760317562606884323, 0.8765941196519945189, 1.000000000000000000 ) ) 
 REPRESENTATION_ITEM ( '' )  );
#26422 = PLANE ( 'NONE',  #25139 ) ;
#26423 = ORIENTED_EDGE ( 'NONE', *, *, #9992, .F. ) ;
#26424 = CARTESIAN_POINT ( 'NONE',  ( -11.10707449861472007, -10.85970573603012035, 57.40177339602415429 ) ) ;
#26425 = DIRECTION ( 'NONE',  ( -3.071710424422018668E-17, 6.404604876783312462E-16, 1.000000000000000000 ) ) ;
#26426 = CARTESIAN_POINT ( 'NONE',  ( -23.34481640033246208, -18.63641755246779752, 69.59371984262205046 ) ) ;
#26427 = ORIENTED_EDGE ( 'NONE', *, *, #8810, .F. ) ;
#26428 = CARTESIAN_POINT ( 'NONE',  ( -10.60148393199744632, -13.03252788045845811, 68.03272542065271011 ) ) ;
#26429 = DIRECTION ( 'NONE',  ( 0.9968684284758859704, -0.07907803935364898784, 1.831731161803828914E-08 ) ) ;
#26430 = EDGE_CURVE ( 'NONE', #32426, #12395, #4652, .T. ) ;
#26431 = CARTESIAN_POINT ( 'NONE',  ( -10.52215041504658188, -13.37196039468858011, 74.97817647370040106 ) ) ;
#26432 = CARTESIAN_POINT ( 'NONE',  ( -22.10033346171958257, -20.08913226167895871, 58.64954131300479645 ) ) ;
#26433 = ORIENTED_EDGE ( 'NONE', *, *, #37212, .T. ) ;
#26434 = CARTESIAN_POINT ( 'NONE',  ( -10.64577699202231287, -11.71757285455929853, 74.67344842241411129 ) ) ;
#26435 = DIRECTION ( 'NONE',  ( -3.071710424422018668E-17, 6.404604876783312462E-16, 1.000000000000000000 ) ) ;
#26436 = CARTESIAN_POINT ( 'NONE',  ( -10.73201024307833862, -12.75570352104612581, 61.02526939955659202 ) ) ;
#26437 =( BOUNDED_CURVE ( )  B_SPLINE_CURVE ( 3, ( #48367, #7020, #368, #40738 ),
 .UNSPECIFIED., .F., .F. ) 
 B_SPLINE_CURVE_WITH_KNOTS ( ( 4, 4 ),
 ( 0.9074455897393690629, 1.000000000000000000 ),
 .UNSPECIFIED. ) 
 CURVE ( )  GEOMETRIC_REPRESENTATION_ITEM ( )  RATIONAL_B_SPLINE_CURVE ( ( 0.6983129098261016132, 0.7760317562607056407, 0.8765941196520050660, 1.000000000000000000 ) ) 
 REPRESENTATION_ITEM ( '' )  );
#26438 = CARTESIAN_POINT ( 'NONE',  ( -18.06756654779004734, -21.77956830110077391, 61.98421986606183509 ) ) ;
#26439 = CARTESIAN_POINT ( 'NONE',  ( -23.89200480383413350, -11.11192299349349533, 70.07706151945906470 ) ) ;
#26440 = CARTESIAN_POINT ( 'NONE',  ( -21.11784385650551954, -9.790100578890868377, 49.79778022625163203 ) ) ;
#26441 = ADVANCED_FACE ( 'NONE', ( #9832 ), #36148, .F. ) ;
#26442 = VERTEX_POINT ( 'NONE', #9352 ) ;
#26443 = CARTESIAN_POINT ( 'NONE',  ( -14.47836531470152188, -7.966228403338186936, 64.04624744032878425 ) ) ;
#26444 = VERTEX_POINT ( 'NONE', #17190 ) ;
#26445 = LINE ( 'NONE', #30156, #46526 ) ;
#26446 = CARTESIAN_POINT ( 'NONE',  ( -15.36434817278061615, -8.119105809824066711, 74.18871620572336667 ) ) ;
#26447 = DIRECTION ( 'NONE',  ( 0.000000000000000000, 0.000000000000000000, 1.000000000000000000 ) ) ;
#26448 = ORIENTED_EDGE ( 'NONE', *, *, #20210, .F. ) ;
#26449 = CARTESIAN_POINT ( 'NONE',  ( -23.55072138245576596, -11.31379833372481691, 66.63034415663315713 ) ) ;
#26450 = AXIS2_PLACEMENT_3D ( 'NONE', #4209, #19218, #34220 ) ;
#26451 = CARTESIAN_POINT ( 'NONE',  ( -10.49796979654650642, -16.16706115165171198, 64.66338504953419886 ) ) ;
#26452 = AXIS2_PLACEMENT_3D ( 'NONE', #47715, #13955, #33397 ) ;
#26453 = DIRECTION ( 'NONE',  ( 1.000000000000000000, 2.866981220435666553E-17, 0.000000000000000000 ) ) ;
#26454 = ORIENTED_EDGE ( 'NONE', *, *, #32523, .T. ) ;
#26455 = CARTESIAN_POINT ( 'NONE',  ( -14.70534385650551989, -8.801233750844183135, 48.81488406609782515 ) ) ;
#26456 = EDGE_CURVE ( 'NONE', #4981, #39185, #42319, .T. ) ;
#26457 = B_SPLINE_CURVE_WITH_KNOTS ( 'NONE', 3,
 ( #12239, #31437, #15680, #22860, #19634, #12007, #37855, #8551, #34642, #26787 ),
 .UNSPECIFIED., .F., .F.,
 ( 4, 2, 2, 2, 4 ),
 ( 0.000000000000000000, 0.2500000000000000000, 0.5000000000000000000, 0.7500000000000000000, 1.000000000000000000 ),
 .UNSPECIFIED. ) ;
#26458 = EDGE_CURVE ( 'NONE', #27657, #33767, #47259, .T. ) ;
#26459 = CARTESIAN_POINT ( 'NONE',  ( -11.39127492490111315, -11.16067319722467666, 60.69357916181100876 ) ) ;
#26460 = CARTESIAN_POINT ( 'NONE',  ( -24.79586717699802279, -15.88714297609664072, 69.69454031355697055 ) ) ;
#26461 = CARTESIAN_POINT ( 'NONE',  ( -13.24261801534493088, -8.643248549050911222, 60.55454889300790455 ) ) ;
#26462 = CARTESIAN_POINT ( 'NONE',  ( -43.03806127622754474, -14.90920654474412643, 58.08826063348414692 ) ) ;
#26463 = VERTEX_POINT ( 'NONE', #21403 ) ;
#26464 = EDGE_LOOP ( 'NONE', ( #23211, #9519, #25141, #42022, #2675 ) ) ;
#26465 = CARTESIAN_POINT ( 'NONE',  ( -16.59284385650551741, -7.406986770994973490, 48.81910596585309747 ) ) ;
#26466 = CARTESIAN_POINT ( 'NONE',  ( -20.44655245503490448, -7.999037100505644204, 70.43755594487680582 ) ) ;
#26467 = SURFACE_SIDE_STYLE ('',( #11946 ) ) ;
#26468 = ADVANCED_FACE ( 'NONE', ( #31991 ), #25090, .F. ) ;
#26469 = CARTESIAN_POINT ( 'NONE',  ( -15.69284385650551172, -7.406986770994973490, 48.81910596585309747 ) ) ;
#26470 = CARTESIAN_POINT ( 'NONE',  ( -16.29054414310137489, -7.847273438603864726, 63.76191313215372247 ) ) ;
#26471 = CARTESIAN_POINT ( 'NONE',  ( -10.19958527806322302, -12.98708191879287455, 67.85176988805619658 ) ) ;
#26472 = CARTESIAN_POINT ( 'NONE',  ( -18.83448644433554620, -7.952703815611509519, 66.91574162229849776 ) ) ;
#26473 = CARTESIAN_POINT ( 'NONE',  ( -13.07710726710083193, -16.59225537930583982, 49.52966884056655772 ) ) ;
#26474 = EDGE_LOOP ( 'NONE', ( #48338, #1805, #32403, #42333, #2965 ) ) ;
#26475 = CARTESIAN_POINT ( 'NONE',  ( -22.99430600995192719, -19.05128598164557729, 62.46480054767778967 ) ) ;
#26476 = CIRCLE ( 'NONE', #41417, 1.999999999999999556 ) ;
#26477 = AXIS2_PLACEMENT_3D ( 'NONE', #32749, #3441, #21680 ) ;
#26478 = ORIENTED_EDGE ( 'NONE', *, *, #14927, .F. ) ;
#26479 = CARTESIAN_POINT ( 'NONE',  ( -13.07007069224803786, -8.763865476245500830, 64.16592477169881192 ) ) ;
#26480 = CYLINDRICAL_SURFACE ( 'NONE', #13962, 5.249999999999998224 ) ;
#26481 = CARTESIAN_POINT ( 'NONE',  ( -12.52014422847536856, -9.200672045504624919, 74.49639875428626112 ) ) ;
#26482 = DIRECTION ( 'NONE',  ( 0.9501515917649786536, 0.3117883138709296453, -1.594035198779740729E-08 ) ) ;
#26483 = ORIENTED_EDGE ( 'NONE', *, *, #38094, .F. ) ;
#26484 = FACE_OUTER_BOUND ( 'NONE', #875, .T. ) ;
#26485 = CARTESIAN_POINT ( 'NONE',  ( -22.77668345155328566, -19.99130182265360745, 72.82213277323756984 ) ) ;
#26486 = AXIS2_PLACEMENT_3D ( 'NONE', #19325, #25996, #29683 ) ;
#26487 = EDGE_CURVE ( 'NONE', #12228, #42385, #2435, .T. ) ;
#26488 = DIRECTION ( 'NONE',  ( 1.000000000000000000, -0.000000000000000000, -2.406186529621654511E-16 ) ) ;
#26489 = DIRECTION ( 'NONE',  ( 1.504942871710700414E-06, -3.061075848816703091E-06, 0.9999999999941824314 ) ) ;
#26490 = EDGE_LOOP ( 'NONE', ( #41554, #3478 ) ) ;
#26491 = CARTESIAN_POINT ( 'NONE',  ( -23.08487763607990928, -19.01185175973044039, 62.36879011380454330 ) ) ;
#26492 = CARTESIAN_POINT ( 'NONE',  ( -18.60622096112062707, -22.16490860957766529, 72.47006221837980888 ) ) ;
#26493 = CARTESIAN_POINT ( 'NONE',  ( -12.54253407177667512, -19.82621502378690082, 65.16674886820000268 ) ) ;
#26494 = FACE_BOUND ( 'NONE', #43124, .T. ) ;
#26495 = APPLICATION_PROTOCOL_DEFINITION ( 'draft international standard', 'automotive_design', 1998, #5489 ) ;
#26496 = B_SPLINE_CURVE_WITH_KNOTS ( 'NONE', 3,
 ( #38624, #5869, #20886, #35410, #28021, #27545, #4909, #35881, #9325, #19920 ),
 .UNSPECIFIED., .F., .F.,
 ( 4, 2, 2, 2, 4 ),
 ( 0.000000000000000000, 0.2500000000000000000, 0.5000000000000000000, 0.7500000000000000000, 1.000000000000000000 ),
 .UNSPECIFIED. ) ;
#26497 = ORIENTED_EDGE ( 'NONE', *, *, #10569, .T. ) ;
#26498 = CARTESIAN_POINT ( 'NONE',  ( -13.18474066807476675, -20.93551553819402855, 58.23145462665691241 ) ) ;
#26499 = CARTESIAN_POINT ( 'NONE',  ( -10.55840457303676061, -16.17443647754080871, 71.74750434597797266 ) ) ;
#26500 = CARTESIAN_POINT ( 'NONE',  ( -23.58616457878146377, -18.99640866789479432, 66.00884704819274873 ) ) ;
#26501 = LINE ( 'NONE', #33368, #14851 ) ;
#26502 = VERTEX_POINT ( 'NONE', #28304 ) ;
#26503 = DIRECTION ( 'NONE',  ( 0.7437128929774846631, -0.6684991644116392573, 1.736198598216997869E-08 ) ) ;
#26504 = ORIENTED_EDGE ( 'NONE', *, *, #23587, .T. ) ;
#26505 = CARTESIAN_POINT ( 'NONE',  ( -20.83700022493355775, -19.12221826660256951, 54.07175714974878389 ) ) ;
#26506 = CARTESIAN_POINT ( 'NONE',  ( -17.22281099395510751, -7.361840332823870625, 70.60540513140719554 ) ) ;
#26507 = CARTESIAN_POINT ( 'NONE',  ( -22.11926001268504294, -9.024814352312150234, 63.30658345311071855 ) ) ;
#26508 = ORIENTED_EDGE ( 'NONE', *, *, #4205, .F. ) ;
#26509 = PLANE ( 'NONE',  #34555 ) ;
#26510 = ORIENTED_EDGE ( 'NONE', *, *, #41370, .F. ) ;
#26511 = ORIENTED_EDGE ( 'NONE', *, *, #45847, .F. ) ;
#26512 = VERTEX_POINT ( 'NONE', #32702 ) ;
#26513 = DIRECTION ( 'NONE',  ( 0.000000000000000000, -1.000000000000000000, 0.000000000000000000 ) ) ;
#26514 = EDGE_CURVE ( 'NONE', #21258, #37232, #46993, .T. ) ;
#26515 = CARTESIAN_POINT ( 'NONE',  ( -20.18610667881221232, -8.319513185189903126, 66.66615430743608783 ) ) ;
#26516 = CARTESIAN_POINT ( 'NONE',  ( -24.72409385541305582, -14.90920654474411577, 58.90588235294116970 ) ) ;
#26517 = EDGE_CURVE ( 'NONE', #25885, #10223, #28160, .T. ) ;
#26518 = DIRECTION ( 'NONE',  ( 0.9529680021988314875, -0.3030709269876716849, -3.918663087574881996E-08 ) ) ;
#26519 = CARTESIAN_POINT ( 'NONE',  ( -23.56138462120852495, -11.33988936615837950, 70.04210750373424332 ) ) ;
#26520 = CARTESIAN_POINT ( 'NONE',  ( -11.42962470904260464, -10.38539412368214521, 74.62380407152070916 ) ) ;
#26521 = VECTOR ( 'NONE', #44506, 999.9999999999998863 ) ;
#26522 = VECTOR ( 'NONE', #35763, 1000.000000000000000 ) ;
#26523 = ORIENTED_EDGE ( 'NONE', *, *, #3472, .T. ) ;
#26524 = VERTEX_POINT ( 'NONE', #9601 ) ;
#26525 = EDGE_CURVE ( 'NONE', #29639, #1741, #17206, .T. ) ;
#26526 = CARTESIAN_POINT ( 'NONE',  ( -17.63866143434000833, -7.362211242860705163, 63.66561706598076853 ) ) ;
#26527 = CARTESIAN_POINT ( 'NONE',  ( -14.73375560093340120, -21.75656996136207866, 61.75105004614717785 ) ) ;
#26528 = CARTESIAN_POINT ( 'NONE',  ( -20.54979434103954006, -8.489990112051950533, 63.61121512946457557 ) ) ;
#26529 = VERTEX_POINT ( 'NONE', #23393 ) ;
#26530 = EDGE_CURVE ( 'NONE', #35456, #14012, #46713, .T. ) ;
#26531 = B_SPLINE_CURVE_WITH_KNOTS ( 'NONE', 3,
 ( #22890, #19174, #22382, #34676, #37883, #15215, #4172, #34179, #22629, #30276 ),
 .UNSPECIFIED., .F., .F.,
 ( 4, 2, 2, 2, 4 ),
 ( 0.000000000000000000, 0.2500000000000000000, 0.5000000000000000000, 0.7500000000000000000, 1.000000000000000000 ),
 .UNSPECIFIED. ) ;
#26532 = CARTESIAN_POINT ( 'NONE',  ( -17.51784385650551812, -9.790100578890868377, 49.79778022625163203 ) ) ;
#26533 = ORIENTED_EDGE ( 'NONE', *, *, #7075, .T. ) ;
#26534 = CARTESIAN_POINT ( 'NONE',  ( -14.66844689667836299, -21.73163918518723037, 61.82255689998408599 ) ) ;
#26535 = CARTESIAN_POINT ( 'NONE',  ( -10.95917937052863422, -17.62195967018737619, 71.58190244267143498 ) ) ;
#26536 = CARTESIAN_POINT ( 'NONE',  ( -10.02995829593802668, -13.89786868041111667, 57.63320316755233819 ) ) ;
#26537 = ORIENTED_EDGE ( 'NONE', *, *, #19217, .F. ) ;
#26538 = CARTESIAN_POINT ( 'NONE',  ( -22.48964968825576705, -9.905448439006629968, 73.76689030015370463 ) ) ;
#26539 = EDGE_CURVE ( 'NONE', #46952, #10750, #27453, .T. ) ;
#26540 = CARTESIAN_POINT ( 'NONE',  ( -14.68116061496366065, -8.368928989582258282, 60.54669703003625614 ) ) ;
#26541 = VERTEX_POINT ( 'NONE', #15740 ) ;
#26542 = CARTESIAN_POINT ( 'NONE',  ( -22.69351926024366861, -21.46836770470456202, 54.38277594638588397 ) ) ;
#26543 =( BOUNDED_CURVE ( )  B_SPLINE_CURVE ( 1, ( #30464, #30707 ),
 .UNSPECIFIED., .F., .F. ) 
 B_SPLINE_CURVE_WITH_KNOTS ( ( 2, 2 ),
 ( 0.000000000000000000, 1.000000000000000000 ),
 .UNSPECIFIED. ) 
 CURVE ( )  GEOMETRIC_REPRESENTATION_ITEM ( )  RATIONAL_B_SPLINE_CURVE ( ( 0.9847278705211290895, 0.9847278705211290895 ) ) 
 REPRESENTATION_ITEM ( '' )  );
#26544 = EDGE_CURVE ( 'NONE', #31360, #38039, #13016, .T. ) ;
#26545 = DIRECTION ( 'NONE',  ( 0.3739781583979218671, 0.9274375111247651349, 6.296758467538776703E-09 ) ) ;
#26546 = CARTESIAN_POINT ( 'NONE',  ( -16.29760673242258306, -22.17363489859456038, 61.87072740723333197 ) ) ;
#26547 = ORIENTED_EDGE ( 'NONE', *, *, #33188, .T. ) ;
#26548 = DIRECTION ( 'NONE',  ( -1.235321096432344812E-06, -4.801898932798036189E-07, -0.9999999999991217026 ) ) ;
#26549 = AXIS2_PLACEMENT_3D ( 'NONE', #2527, #3483, #36957 ) ;
#26550 = ORIENTED_EDGE ( 'NONE', *, *, #47350, .F. ) ;
#26551 = FACE_OUTER_BOUND ( 'NONE', #83, .T. ) ;
#26552 = FACE_OUTER_BOUND ( 'NONE', #25642, .T. ) ;
#26553 = EDGE_LOOP ( 'NONE', ( #7750, #40045, #47205, #2679, #25128 ) ) ;
#26554 = CARTESIAN_POINT ( 'NONE',  ( -12.84691039585993444, -8.931012183600500975, 67.56438067310742213 ) ) ;
#26555 = CARTESIAN_POINT ( 'NONE',  ( -23.80139567369806741, -11.92276173358724201, 59.48235729430358987 ) ) ;
#26556 = CARTESIAN_POINT ( 'NONE',  ( -20.17268378225416825, -8.371407738384645469, 70.25100341248858626 ) ) ;
#26557 = EDGE_LOOP ( 'NONE', ( #3944, #24212, #13534, #29439, #4818 ) ) ;
#26558 = CARTESIAN_POINT ( 'NONE',  ( -11.27147141364421401, -11.36706973555563494, 64.14882062048422995 ) ) ;
#26559 = CIRCLE ( 'NONE', #10836, 4.686499999999999666 ) ;
#26560 = CARTESIAN_POINT ( 'NONE',  ( -16.30881670716104992, -7.898512009833411618, 60.20028524975941764 ) ) ;
#26561 =( BOUNDED_SURFACE ( )  B_SPLINE_SURFACE ( 3, 1, ( 
 ( #11833, #1217 ),
 ( #19452, #8374 ),
 ( #31031, #4204 ),
 ( #4682, #1458 ),
 ( #41874, #23399 ),
 ( #19705, #8148 ),
 ( #747, #16470 ) ),
 .UNSPECIFIED., .T., .F., .F. ) 
 B_SPLINE_SURFACE_WITH_KNOTS ( ( 4, 3, 4 ),
 ( 2, 2 ),
 ( 0.000000000000000000, 0.5000000000000000000, 1.000000000000000000 ),
 ( 0.000000000000000000, 1.000000000000000000 ),
 .UNSPECIFIED. ) 
 GEOMETRIC_REPRESENTATION_ITEM ( )  RATIONAL_B_SPLINE_SURFACE ( (
 ( 1.000000000000000000, 1.000000000000000000),
 ( 0.3333333333333335369, 0.3333333333333330373),
 ( 0.3333333333333335369, 0.3333333333333330373),
 ( 1.000000000000000000, 1.000000000000000000),
 ( 0.3333333333333333703, 0.3333333333333333703),
 ( 0.3333333333333333703, 0.3333333333333333703),
 ( 1.000000000000000000, 1.000000000000000000) ) ) 
 REPRESENTATION_ITEM ( '' )  SURFACE ( )  );
#26562 = CARTESIAN_POINT ( 'NONE',  ( -10.90274307526027542, -17.35673385334968089, 68.16892125527850510 ) ) ;
#26563 = VERTEX_POINT ( 'NONE', #39377 ) ;
#26564 = EDGE_CURVE ( 'NONE', #6974, #15234, #12543, .T. ) ;
#26566 = CARTESIAN_POINT ( 'NONE',  ( -14.42683414290149813, -8.428067600363897682, 67.25975083869262505 ) ) ;
#26565 =( BOUNDED_CURVE ( )  B_SPLINE_CURVE ( 3, ( #12737, #15930, #27511, #38332 ),
 .UNSPECIFIED., .F., .F. ) 
 B_SPLINE_CURVE_WITH_KNOTS ( ( 4, 4 ),
 ( 0.9074455897393608472, 1.000000000000000000 ),
 .UNSPECIFIED. ) 
 CURVE ( )  GEOMETRIC_REPRESENTATION_ITEM ( )  RATIONAL_B_SPLINE_CURVE ( ( 0.6983129098260804080, 0.7760317562606873221, 0.8765941196519938527, 1.000000000000000000 ) ) 
 REPRESENTATION_ITEM ( '' )  );
#26567 = AXIS2_PLACEMENT_3D ( 'NONE', #20994, #35523, #46625 ) ;
#26568 = B_SPLINE_CURVE_WITH_KNOTS ( 'NONE', 3,
 ( #17789, #21746, #36731, #39982, #44186, #28889, #18520, #44904, #43937, #2556 ),
 .UNSPECIFIED., .F., .F.,
 ( 4, 2, 2, 2, 4 ),
 ( 0.1272669073658494465, 0.2522669073463357781, 0.3772669073268221096, 0.5022669073073084967, 0.6272669072877947727 ),
 .UNSPECIFIED. ) ;
#26569 = CARTESIAN_POINT ( 'NONE',  ( -21.73099075187129614, -8.730192115828774746, 70.31627817507801126 ) ) ;
#26570 = ORIENTED_EDGE ( 'NONE', *, *, #17243, .T. ) ;
#26571 = VERTEX_POINT ( 'NONE', #38646 ) ;
#26572 = CARTESIAN_POINT ( 'NONE',  ( -21.65477468606848532, -9.232349032746775208, 66.96149992608901869 ) ) ;
#26573 = CARTESIAN_POINT ( 'NONE',  ( -10.73412848974934874, -11.53077067998621175, 71.20365450754333381 ) ) ;
#26574 = DIRECTION ( 'NONE',  ( -0.4501286257827956661, -0.8929637284072021730, 1.500157795982635103E-08 ) ) ;
#26575 = CARTESIAN_POINT ( 'NONE',  ( -10.39542940759278267, -14.25923383539692146, 64.39363650855324295 ) ) ;
#26576 = CARTESIAN_POINT ( 'NONE',  ( -21.56784385650551528, -6.428312510596450480, 51.20221977374900035 ) ) ;
#26577 = CARTESIAN_POINT ( 'NONE',  ( -20.25220558506708102, -7.916061535415647832, 70.36445088532752834 ) ) ;
#26578 = CARTESIAN_POINT ( 'NONE',  ( -12.35395094432871410, -20.26789845123980527, 68.59303345011528563 ) ) ;
#26579 = CARTESIAN_POINT ( 'NONE',  ( -17.01596769717176372, -7.370308014455987156, 74.07522855441366971 ) ) ;
#26580 =( BOUNDED_SURFACE ( )  B_SPLINE_SURFACE ( 3, 1, ( 
 ( #5375, #16914 ),
 ( #35396, #13462 ),
 ( #27772, #39089 ),
 ( #1419, #42798 ),
 ( #35149, #20869 ),
 ( #1674, #16434 ),
 ( #34912, #35868 ) ),
 .UNSPECIFIED., .T., .F., .F. ) 
 B_SPLINE_SURFACE_WITH_KNOTS ( ( 4, 3, 4 ),
 ( 2, 2 ),
 ( 0.000000000000000000, 0.5000000000000000000, 1.000000000000000000 ),
 ( 0.000000000000000000, 1.000000000000000000 ),
 .UNSPECIFIED. ) 
 GEOMETRIC_REPRESENTATION_ITEM ( )  RATIONAL_B_SPLINE_SURFACE ( (
 ( 1.000000000000000000, 1.000000000000000000),
 ( 0.3333333333333335369, 0.3333333333333330373),
 ( 0.3333333333333335369, 0.3333333333333330373),
 ( 1.000000000000000000, 1.000000000000000000),
 ( 0.3333333333333333703, 0.3333333333333333703),
 ( 0.3333333333333333703, 0.3333333333333333703),
 ( 1.000000000000000000, 1.000000000000000000) ) ) 
 REPRESENTATION_ITEM ( '' )  SURFACE ( )  );
#26581 = CARTESIAN_POINT ( 'NONE',  ( -12.41315173547891781, -9.850077678253004621, 57.38935532239157311 ) ) ;
#26582 = ORIENTED_EDGE ( 'NONE', *, *, #24085, .T. ) ;
#26583 = ADVANCED_FACE ( 'NONE', ( #9106 ), #4933, .T. ) ;
#26584 = CARTESIAN_POINT ( 'NONE',  ( -11.51937024597566328, -18.66112914712196158, 64.74707106785028543 ) ) ;
#26585 = EDGE_CURVE ( 'NONE', #17102, #8229, #47179, .T. ) ;
#26586 = CIRCLE ( 'NONE', #33615, 1.999999999999994893 ) ;
#26587 = CARTESIAN_POINT ( 'NONE',  ( -19.40149108948937240, -21.57997799771671765, 65.55666331783336886 ) ) ;
#26588 = CARTESIAN_POINT ( 'NONE',  ( -13.53206926677945887, -8.990420089060579656, 60.45566976265779147 ) ) ;
#26589 = VECTOR ( 'NONE', #12146, 1000.000000000000000 ) ;
#26590 = VERTEX_POINT ( 'NONE', #24120 ) ;
#26591 = CIRCLE ( 'NONE', #48582, 3.999999999999996447 ) ;
#26592 = ORIENTED_EDGE ( 'NONE', *, *, #17267, .F. ) ;
#26593 = CARTESIAN_POINT ( 'NONE',  ( -17.42558057905623059, -9.559206755253619292, 50.77966884056655772 ) ) ;
#26594 = CARTESIAN_POINT ( 'NONE',  ( -15.40122101639776808, -21.97944830692560458, 72.22292343801429126 ) ) ;
#26595 = CARTESIAN_POINT ( 'NONE',  ( -15.15534385541304729, -8.623186033802571870, 49.24843789510467928 ) ) ;
#26596 = VECTOR ( 'NONE', #29095, 1000.000000000000000 ) ;
#26597 = EDGE_CURVE ( 'NONE', #24724, #1836, #39127, .T. ) ;
#26598 = ORIENTED_EDGE ( 'NONE', *, *, #786, .F. ) ;
#26599 = EDGE_CURVE ( 'NONE', #26956, #10314, #26288, .T. ) ;
#26600 = CARTESIAN_POINT ( 'NONE',  ( -14.36817892824948650, -8.455618309860652104, 67.54503025475185041 ) ) ;
#26601 = ADVANCED_FACE ( 'NONE', ( #28043 ), #45813, .T. ) ;
#26602 = ADVANCED_FACE ( 'NONE', ( #38889 ), #4569, .T. ) ;
#26603 = EDGE_CURVE ( 'NONE', #39108, #24138, #29858, .T. ) ;
#26604 = ORIENTED_EDGE ( 'NONE', *, *, #48243, .T. ) ;
#26605 = CARTESIAN_POINT ( 'NONE',  ( -9.976686065099853451, -14.58608982656816622, 71.51437949254577120 ) ) ;
#26606 = CARTESIAN_POINT ( 'NONE',  ( -10.37382936219775154, -14.83089353207902228, 74.81251018390588570 ) ) ;
#26607 = CARTESIAN_POINT ( 'NONE',  ( -23.04402284766838349, -19.06632961612601918, 59.16938527523783620 ) ) ;
#26608 = ORIENTED_EDGE ( 'NONE', *, *, #33042, .F. ) ;
#26609 = CARTESIAN_POINT ( 'NONE',  ( -12.25434429315920859, -20.17366997322574562, 65.05170215947674706 ) ) ;
#26610 = VERTEX_POINT ( 'NONE', #46770 ) ;
#26611 = CARTESIAN_POINT ( 'NONE',  ( -23.77935182056019414, -10.92131427075145211, 73.52226634401078798 ) ) ;
#26612 = CYLINDRICAL_SURFACE ( 'NONE', #15552, 0.1499999999999991063 ) ;
#26613 = ORIENTED_EDGE ( 'NONE', *, *, #13065, .F. ) ;
#26614 = CARTESIAN_POINT ( 'NONE',  ( -16.36034204477525478, -21.78224588847237086, 65.52564618146095654 ) ) ;
#26615 = PLANE ( 'NONE',  #38338 ) ;
#26616 = CARTESIAN_POINT ( 'NONE',  ( -19.18034385650551599, -6.424090610841176385, 49.80797279389978627 ) ) ;
#26617 = AXIS2_PLACEMENT_3D ( 'NONE', #13147, #39273, #12918 ) ;
#26618 = CARTESIAN_POINT ( 'NONE',  ( -24.47066272824306665, -14.57993217219608972, 62.99824437345091610 ) ) ;
#26619 = CIRCLE ( 'NONE', #24273, 4.686499999999999666 ) ;
#26620 = CARTESIAN_POINT ( 'NONE',  ( -23.00454255336054743, -10.50046069577333441, 59.88731295783226471 ) ) ;
#26621 = CARTESIAN_POINT ( 'NONE',  ( -10.52131307627743340, -17.61206215953548337, 68.22005024680343865 ) ) ;
#26622 = CARTESIAN_POINT ( 'NONE',  ( -20.84119928492008000, -20.97572016636869918, 62.41471400470057773 ) ) ;
#26623 = ORIENTED_EDGE ( 'NONE', *, *, #25012, .T. ) ;
#26624 = CARTESIAN_POINT ( 'NONE',  ( -22.13034385541265792, -6.857644439845596906, 49.98602051094377430 ) ) ;
#26625 = AXIS2_PLACEMENT_3D ( 'NONE', #16856, #27232, #8521 ) ;
#26626 = AXIS2_PLACEMENT_3D ( 'NONE', #7552, #172, #15148 ) ;
#26627 = CARTESIAN_POINT ( 'NONE',  ( -13.12744695462171407, -20.89546087334666069, 58.30296024829184631 ) ) ;
#26628 = CARTESIAN_POINT ( 'NONE',  ( -22.38400322090610217, -20.36826016184844335, 62.41934579407823236 ) ) ;
#26629 = DIRECTION ( 'NONE',  ( -0.9529680021988313765, 0.3030709269876716849, 3.918663088761644638E-08 ) ) ;
#26630 = CARTESIAN_POINT ( 'NONE',  ( -24.22177629109872399, -13.13842424187848934, 63.13264177643409880 ) ) ;
#26631 = EDGE_CURVE ( 'NONE', #6712, #1863, #1455, .T. ) ;
#26632 = VERTEX_POINT ( 'NONE', #6851 ) ;
#26633 = ORIENTED_EDGE ( 'NONE', *, *, #31345, .F. ) ;
#26634 = FACE_OUTER_BOUND ( 'NONE', #2403, .T. ) ;
#26635 = CARTESIAN_POINT ( 'NONE',  ( -14.97837282748989729, -8.193824179639600302, 60.73484884663594130 ) ) ;
#26636 = ORIENTED_EDGE ( 'NONE', *, *, #40110, .T. ) ;
#26637 = CARTESIAN_POINT ( 'NONE',  ( -24.83263378688676326, -15.59489965655864374, 73.18799144572807336 ) ) ;
#26638 = DIRECTION ( 'NONE',  ( 0.000000000000000000, 0.9999954153791273948, 0.003028072113819836077 ) ) ;
#26639 = AXIS2_PLACEMENT_3D ( 'NONE', #42434, #8703, #23731 ) ;
#26640 = CARTESIAN_POINT ( 'NONE',  ( -10.26935876326470876, -12.73200256517937312, 64.42869467744635870 ) ) ;
#26641 = CARTESIAN_POINT ( 'NONE',  ( -24.73118759497682362, -16.26147063645814583, 62.69354438008230090 ) ) ;
#26642 = CARTESIAN_POINT ( 'NONE',  ( -21.60997298628545593, -20.97227605400240336, 72.68479748740878676 ) ) ;
#26643 = CARTESIAN_POINT ( 'NONE',  ( -23.58130562506259764, -19.00348601836356721, 65.93051099385326097 ) ) ;
#26644 = CARTESIAN_POINT ( 'NONE',  ( -27.42409385541305511, -25.10920654474410441, 78.99999999999998579 ) ) ;
#26645 = CARTESIAN_POINT ( 'NONE',  ( -11.58430515049292886, -10.18324995017449908, 71.16904308454122940 ) ) ;
#26646 = B_SPLINE_CURVE_WITH_KNOTS ( 'NONE', 1,
 ( #967, #23629 ),
 .UNSPECIFIED., .F., .F.,
 ( 2, 2 ),
 ( 0.000000000000000000, 1.000000000000000000 ),
 .UNSPECIFIED. ) ;
#26647 = CARTESIAN_POINT ( 'NONE',  ( -10.54994933093899867, -13.24305344519376781, 71.49356453765415154 ) ) ;
#26648 = DIRECTION ( 'NONE',  ( -0.000000000000000000, -1.000000000000000000, 0.000000000000000000 ) ) ;
#26649 = CARTESIAN_POINT ( 'NONE',  ( -24.20371252810814866, -12.87440185077122834, 66.58774614429587757 ) ) ;
#26650 = CARTESIAN_POINT ( 'NONE',  ( -23.28952267755650851, -10.88343168269180339, 73.51760210707182353 ) ) ;
#26651 = ORIENTED_EDGE ( 'NONE', *, *, #47059, .F. ) ;
#26652 = EDGE_LOOP ( 'NONE', ( #33595, #23898, #11200, #4201 ) ) ;
#26653 = CARTESIAN_POINT ( 'NONE',  ( -15.60534385541304836, -7.595227055684746986, 51.75156210489594599 ) ) ;
#26654 = ORIENTED_EDGE ( 'NONE', *, *, #1067, .F. ) ;
#26655 = CARTESIAN_POINT ( 'NONE',  ( -23.03034385541303308, -6.857644439848129991, 49.98602051094116661 ) ) ;
#26656 = FACE_OUTER_BOUND ( 'NONE', #37830, .T. ) ;
#26657 =( BOUNDED_CURVE ( )  B_SPLINE_CURVE ( 3, ( #1233, #30218, #41274, #2457 ),
 .UNSPECIFIED., .F., .F. ) 
 B_SPLINE_CURVE_WITH_KNOTS ( ( 4, 4 ),
 ( 0.000000000000000000, 0.4074455897393574055 ),
 .UNSPECIFIED. ) 
 CURVE ( )  GEOMETRIC_REPRESENTATION_ITEM ( )  RATIONAL_B_SPLINE_CURVE ( ( 1.000000000000000000, 0.4567392136813416270, 0.3561768502900338751, 0.6983129098260767442 ) ) 
 REPRESENTATION_ITEM ( '' )  );
#26658 = AXIS2_PLACEMENT_3D ( 'NONE', #1197, #27790, #9586 ) ;
#26659 = B_SPLINE_CURVE_WITH_KNOTS ( 'NONE', 3,
 ( #41866, #27079, #19700, #31503, #42833, #31023, #1711, #46540, #34710, #12298 ),
 .UNSPECIFIED., .F., .F.,
 ( 4, 2, 2, 2, 4 ),
 ( 0.000000000000000000, 0.2500000000000000000, 0.5000000000000000000, 0.7500000000000000000, 1.000000000000000000 ),
 .UNSPECIFIED. ) ;
#26660 = VECTOR ( 'NONE', #18012, 1000.000000000000000 ) ;
#26661 = CARTESIAN_POINT ( 'NONE',  ( -24.34138250757122179, -16.17068267630804357, 62.89328676667766160 ) ) ;
#26662 = EDGE_CURVE ( 'NONE', #17465, #1836, #21402, .T. ) ;
#26663 = EDGE_CURVE ( 'NONE', #5991, #39328, #8051, .T. ) ;
#26664 = CARTESIAN_POINT ( 'NONE',  ( -16.09337498760136853, -22.13948385882417824, 58.40090183616962349 ) ) ;
#26665 = EDGE_LOOP ( 'NONE', ( #28834, #47551 ) ) ;
#26666 = CARTESIAN_POINT ( 'NONE',  ( -13.89388974506275787, -21.36980381032900667, 72.11102993026078423 ) ) ;
#26667 = AXIS2_PLACEMENT_3D ( 'NONE', #19900, #27768, #34906 ) ;
#26668 = CARTESIAN_POINT ( 'NONE',  ( -17.63866254341385442, -7.362211269489866261, 63.66561597723832477 ) ) ;
#26669 = ORIENTED_EDGE ( 'NONE', *, *, #17708, .F. ) ;
#26670 = CARTESIAN_POINT ( 'NONE',  ( -22.36580195822040906, -20.38434351641670972, 62.43427942229939731 ) ) ;
#26671 = CARTESIAN_POINT ( 'NONE',  ( -23.77487038158592014, -11.74745262826995429, 62.96690348473899235 ) ) ;
#26672 = ORIENTED_EDGE ( 'NONE', *, *, #16951, .T. ) ;
#26673 = EDGE_CURVE ( 'NONE', #17004, #22618, #40342, .T. ) ;
#26674 = EDGE_CURVE ( 'NONE', #18062, #13744, #29066, .T. ) ;
#26675 = CARTESIAN_POINT ( 'NONE',  ( -14.37682202087475680, -19.38786730597468022, 53.49899999999994549 ) ) ;
#26676 = CARTESIAN_POINT ( 'NONE',  ( -15.11475081961186540, -8.199755259496424031, 56.92170200118545154 ) ) ;
#26677 = CARTESIAN_POINT ( 'NONE',  ( -17.22281210278579167, -7.361840297529252730, 70.60540404266352255 ) ) ;
#26678 = ORIENTED_EDGE ( 'NONE', *, *, #11670, .F. ) ;
#26679 = FACE_OUTER_BOUND ( 'NONE', #39465, .T. ) ;
#26680 = CARTESIAN_POINT ( 'NONE',  ( -50.42609385541305755, -14.80920654474419074, 65.04705882352939739 ) ) ;
#26681 = CARTESIAN_POINT ( 'NONE',  ( -15.40811923343077083, -21.56513327689926030, 72.06047564147742435 ) ) ;
#26682 = CARTESIAN_POINT ( 'NONE',  ( -10.52483499103918874, -17.62059296423454313, 68.35367848399930324 ) ) ;
#26683 = EDGE_LOOP ( 'NONE', ( #36357, #33959, #207, #14147, #47098 ) ) ;
#26684 = CARTESIAN_POINT ( 'NONE',  ( -17.77409385759798965, -6.859212275519751323, 50.50378509014259265 ) ) ;
#26685 = CARTESIAN_POINT ( 'NONE',  ( -13.65828898514496359, -20.76952646431350757, 65.00101022825411690 ) ) ;
#26686 = CARTESIAN_POINT ( 'NONE',  ( -10.39670887254123954, -15.41691257807914184, 61.12969206769774644 ) ) ;
#26687 = CARTESIAN_POINT ( 'NONE',  ( -16.34301583228449317, -10.23680828416977739, 49.52966884056655772 ) ) ;
#26688 = CARTESIAN_POINT ( 'NONE',  ( -11.08897232857050597, -11.71577735905851902, 71.08860879097652230 ) ) ;
#26689 = CARTESIAN_POINT ( 'NONE',  ( -18.13659385650551670, -6.915538690918074494, 49.31353937987644542 ) ) ;
#26690 = ADVANCED_FACE ( 'NONE', ( #10068 ), #41679, .T. ) ;
#26691 = VERTEX_POINT ( 'NONE', #2186 ) ;
#26692 = CIRCLE ( 'NONE', #15669, 5.249999999999998224 ) ;
#26693 = CARTESIAN_POINT ( 'NONE',  ( -17.70078711893434331, -22.25418926393874486, 58.58366112844367279 ) ) ;
#26694 = CARTESIAN_POINT ( 'NONE',  ( -24.26830686446636776, -16.27808571390248105, 59.40867021969434347 ) ) ;
#26695 = ORIENTED_EDGE ( 'NONE', *, *, #28225, .F. ) ;
#26696 = CARTESIAN_POINT ( 'NONE',  ( -19.49109506855409180, -21.54969648977046148, 62.28031529404344013 ) ) ;
#26697 = VERTEX_POINT ( 'NONE', #16944 ) ;
#26698 = CARTESIAN_POINT ( 'NONE',  ( -42.81012326717776517, -14.90920654474412643, 59.91176470588234793 ) ) ;
#26699 = VECTOR ( 'NONE', #7943, 1000.000000000000000 ) ;
#26700 = DIRECTION ( 'NONE',  ( -3.071710424422018668E-17, 6.404604876783312462E-16, 1.000000000000000000 ) ) ;
#26701 = CARTESIAN_POINT ( 'NONE',  ( -20.81921389985186721, -21.44071754855728784, 58.75979745677555854 ) ) ;
#26702 = ORIENTED_EDGE ( 'NONE', *, *, #16466, .F. ) ;
#26703 = CARTESIAN_POINT ( 'NONE',  ( -16.50534385650551883, -8.801233750844183135, 48.81488406609782515 ) ) ;
#26704 = B_SPLINE_CURVE_WITH_KNOTS ( 'NONE', 1,
 ( #24064, #38829 ),
 .UNSPECIFIED., .F., .F.,
 ( 2, 2 ),
 ( 0.000000000000000000, 1.000000000000000000 ),
 .UNSPECIFIED. ) ;
#26705 = AXIS2_PLACEMENT_3D ( 'NONE', #42136, #30582, #526 ) ;
#26706 = DIRECTION ( 'NONE',  ( -3.071710424422018668E-17, 6.404604876783312462E-16, 1.000000000000000000 ) ) ;
#26707 = CARTESIAN_POINT ( 'NONE',  ( -18.60622205832422082, -22.16490843864383109, 72.47006330605313451 ) ) ;
#26708 = B_SPLINE_CURVE_WITH_KNOTS ( 'NONE', 3,
 ( #14532, #10880, #7205, #22211, #33501, #29848, #44877, #12336, #38427, #1244 ),
 .UNSPECIFIED., .F., .F.,
 ( 4, 2, 2, 2, 4 ),
 ( 0.6272669072878269692, 0.7522669073073300350, 0.8772669073268331008, 1.002266907346336167, 1.127266907365839232 ),
 .UNSPECIFIED. ) ;
#26709 =( BOUNDED_SURFACE ( )  B_SPLINE_SURFACE ( 3, 1, ( 
 ( #14994, #30058 ),
 ( #26345, #41358 ),
 ( #8138, #15481 ),
 ( #30547, #45567 ),
 ( #16705, #38884 ),
 ( #46536, #19695 ),
 ( #20169, #16461 ) ),
 .UNSPECIFIED., .T., .F., .F. ) 
 B_SPLINE_SURFACE_WITH_KNOTS ( ( 4, 3, 4 ),
 ( 2, 2 ),
 ( 0.000000000000000000, 0.5000000000000000000, 1.000000000000000000 ),
 ( 0.000000000000000000, 1.000000000000000000 ),
 .UNSPECIFIED. ) 
 GEOMETRIC_REPRESENTATION_ITEM ( )  RATIONAL_B_SPLINE_SURFACE ( (
 ( 1.000000000000000000, 1.000000000000000000),
 ( 0.3333333333333335369, 0.3333333333333330373),
 ( 0.3333333333333335369, 0.3333333333333330373),
 ( 1.000000000000000000, 1.000000000000000000),
 ( 0.3333333333333333703, 0.3333333333333333703),
 ( 0.3333333333333333703, 0.3333333333333333703),
 ( 1.000000000000000000, 1.000000000000000000) ) ) 
 REPRESENTATION_ITEM ( '' )  SURFACE ( )  );
#26710 = CARTESIAN_POINT ( 'NONE',  ( -15.62100938680255524, -7.580606089661849012, 70.72494556531428600 ) ) ;
#26711 = LINE ( 'NONE', #22522, #63 ) ;
#26712 = ORIENTED_EDGE ( 'NONE', *, *, #48332, .F. ) ;
#26713 = ORIENTED_EDGE ( 'NONE', *, *, #4645, .F. ) ;
#26714 = CARTESIAN_POINT ( 'NONE',  ( -16.19909385650551670, -8.114302828567740988, 52.18300498402516041 ) ) ;
#26715 = DIRECTION ( 'NONE',  ( -0.000000000000000000, -1.000000000000000000, -0.000000000000000000 ) ) ;
#26716 = CARTESIAN_POINT ( 'NONE',  ( -10.44644826855572006, -14.24945678126164061, 61.14494592119106642 ) ) ;
#26717 = LINE ( 'NONE', #33842, #48086 ) ;
#26718 = CARTESIAN_POINT ( 'NONE',  ( -15.01784385650551457, -9.790100578890868377, 49.79778022625163203 ) ) ;
#26719 = B_SPLINE_CURVE_WITH_KNOTS ( 'NONE', 1,
 ( #31652, #9494 ),
 .UNSPECIFIED., .F., .F.,
 ( 2, 2 ),
 ( 0.000000000000000000, 1.000000000000000000 ),
 .UNSPECIFIED. ) ;
#26720 =( BOUNDED_CURVE ( )  B_SPLINE_CURVE ( 3, ( #26685, #27166, #8221, #46121 ),
 .UNSPECIFIED., .F., .F. ) 
 B_SPLINE_CURVE_WITH_KNOTS ( ( 4, 4 ),
 ( 0.5000000000000000000, 0.9074455897393781667 ),
 .UNSPECIFIED. ) 
 CURVE ( )  GEOMETRIC_REPRESENTATION_ITEM ( )  RATIONAL_B_SPLINE_CURVE ( ( 0.9999999999999985567, 0.4567392136813051007, 0.3561768502900212741, 0.6983129098261455781 ) ) 
 REPRESENTATION_ITEM ( '' )  );
#26721 = DIRECTION ( 'NONE',  ( -1.000000000000000000, -2.866981220435666553E-17, 0.000000000000000000 ) ) ;
#26722 = EDGE_CURVE ( 'NONE', #28688, #47772, #7613, .T. ) ;
#26723 = CARTESIAN_POINT ( 'NONE',  ( -10.66644504159021878, -12.78954850062448578, 68.15321152835137752 ) ) ;
#26724 = AXIS2_PLACEMENT_3D ( 'NONE', #43568, #41311, #44785 ) ;
#26725 = CARTESIAN_POINT ( 'NONE',  ( -24.72409385541305582, -14.80920654474412679, 59.01176470588234224 ) ) ;
#26726 = FACE_OUTER_BOUND ( 'NONE', #14591, .T. ) ;
#26727 = ORIENTED_EDGE ( 'NONE', *, *, #45921, .T. ) ;
#26728 = CARTESIAN_POINT ( 'NONE',  ( -24.47744085606393583, -14.87036544990968423, 62.80476446885626984 ) ) ;
#26729 = CIRCLE ( 'NONE', #3131, 5.249999999999998224 ) ;
#26730 = EDGE_LOOP ( 'NONE', ( #23058, #11995, #1471, #45 ) ) ;
#26731 = ADVANCED_FACE ( 'NONE', ( #17676 ), #6126, .T. ) ;
#26732 = CARTESIAN_POINT ( 'NONE',  ( -21.73633048181673999, -9.221757950931626979, 59.87738363463013513 ) ) ;
#26733 = CARTESIAN_POINT ( 'NONE',  ( -24.90891992605694227, -15.28604896337863472, 54.27966884056655061 ) ) ;
#26734 = DIRECTION ( 'NONE',  ( 0.2393415023380396356, -0.9709354485539014590, 6.438601123316498798E-08 ) ) ;
#26735 = CARTESIAN_POINT ( 'NONE',  ( -13.24069677618990504, -9.134368938356168144, 64.20386707414483851 ) ) ;
#26736 = EDGE_CURVE ( 'NONE', #40267, #31211, #32476, .T. ) ;
#26737 = ORIENTED_EDGE ( 'NONE', *, *, #23518, .F. ) ;
#26738 = CARTESIAN_POINT ( 'NONE',  ( -10.70532053225239366, -12.67267096592666675, 61.08381491717225487 ) ) ;
#26739 = CARTESIAN_POINT ( 'NONE',  ( -12.38445583493520630, -13.33796604008351494, 49.52966884056655772 ) ) ;
#26740 = EDGE_CURVE ( 'NONE', #46626, #40821, #29265, .T. ) ;
#26741 = CARTESIAN_POINT ( 'NONE',  ( -12.23220172533775241, -19.57856247689574403, 57.92682373937842044 ) ) ;
#26742 = CARTESIAN_POINT ( 'NONE',  ( -24.48534228222961673, -17.18449783053895530, 72.98997734255360115 ) ) ;
#26743 = ORIENTED_EDGE ( 'NONE', *, *, #6033, .F. ) ;
#26744 = PLANE ( 'NONE',  #37781 ) ;
#26745 = DIRECTION ( 'NONE',  ( 0.000000000000000000, 0.000000000000000000, 1.000000000000000000 ) ) ;
#26746 = CARTESIAN_POINT ( 'NONE',  ( -23.41616298382994898, -18.52428493080399363, 72.77840375779385340 ) ) ;
#26747 = FACE_BOUND ( 'NONE', #37357, .T. ) ;
#26748 = EDGE_LOOP ( 'NONE', ( #1332, #25796, #40060, #24928 ) ) ;
#26749 = DIRECTION ( 'NONE',  ( 0.1261685609230672744, 0.9920088176193796459, 5.058037262945178220E-08 ) ) ;
#26750 = EDGE_CURVE ( 'NONE', #9308, #41453, #28303, .T. ) ;
#26751 = VECTOR ( 'NONE', #6028, 1000.000000000000000 ) ;
#26752 = FACE_OUTER_BOUND ( 'NONE', #34584, .T. ) ;
#26753 = CARTESIAN_POINT ( 'NONE',  ( -40.64308517176574753, -27.10920654474410796, 77.24806946917840378 ) ) ;
#26754 = ORIENTED_EDGE ( 'NONE', *, *, #20068, .T. ) ;
#26755 = CARTESIAN_POINT ( 'NONE',  ( -10.55855397105558779, -16.42450592920206276, 71.33261492083846633 ) ) ;
#26756 = VERTEX_POINT ( 'NONE', #47003 ) ;
#26757 = CYLINDRICAL_SURFACE ( 'NONE', #28965, 0.1499999999999956923 ) ;
#26758 = CARTESIAN_POINT ( 'NONE',  ( -22.97806169198474535, -10.54588128516193102, 63.26113122312534642 ) ) ;
#26759 = FACE_OUTER_BOUND ( 'NONE', #29576, .T. ) ;
#26760 = ORIENTED_EDGE ( 'NONE', *, *, #20338, .T. ) ;
#26761 = CARTESIAN_POINT ( 'NONE',  ( -11.64235026963700292, -18.84330375823651949, 68.21689631561287115 ) ) ;
#26762 = ORIENTED_EDGE ( 'NONE', *, *, #5545, .T. ) ;
#26763 = ORIENTED_EDGE ( 'NONE', *, *, #33848, .F. ) ;
#26764 = VERTEX_POINT ( 'NONE', #43329 ) ;
#26765 = CARTESIAN_POINT ( 'NONE',  ( -14.99706723701585354, -21.85287888328288375, 65.29092001793476641 ) ) ;
#26767 = CARTESIAN_POINT ( 'NONE',  ( -20.44433886619616914, -7.998055119120133227, 66.89448804686142580 ) ) ;
#26766 = TOROIDAL_SURFACE ( 'NONE', #40907, 1.499999999999998224, 0.5000000000000000000 ) ;
#26768 = CARTESIAN_POINT ( 'NONE',  ( -21.90510274986183603, -8.857417179619462289, 66.76811671267451231 ) ) ;
#26769 = CARTESIAN_POINT ( 'NONE',  ( -17.11594671439511828, -7.315539529225058679, 53.49999999999994316 ) ) ;
#26770 = CARTESIAN_POINT ( 'NONE',  ( -18.55662820153069248, -10.26160847489872197, 52.02966884056656482 ) ) ;
#26771 = CARTESIAN_POINT ( 'NONE',  ( -12.40538917401127961, -20.31523793222865493, 68.52152763170285255 ) ) ;
#26772 = CARTESIAN_POINT ( 'NONE',  ( -22.83095763869631512, -19.93459457198476770, 72.82895875648904394 ) ) ;
#26773 = AXIS2_PLACEMENT_3D ( 'NONE', #42462, #41972, #8971 ) ;
#26774 = ORIENTED_EDGE ( 'NONE', *, *, #6281, .T. ) ;
#26775 = ORIENTED_EDGE ( 'NONE', *, *, #46941, .T. ) ;
#26776 =( BOUNDED_SURFACE ( )  B_SPLINE_SURFACE ( 3, 1, ( 
 ( #45043, #25153 ),
 ( #6447, #26301 ),
 ( #30008, #36217 ),
 ( #10134, #29081 ),
 ( #30503, #11524 ),
 ( #11289, #14034 ),
 ( #15435, #21462 ) ),
 .UNSPECIFIED., .T., .F., .F. ) 
 B_SPLINE_SURFACE_WITH_KNOTS ( ( 4, 3, 4 ),
 ( 2, 2 ),
 ( 0.000000000000000000, 0.5000000000000000000, 1.000000000000000000 ),
 ( 0.000000000000000000, 1.000000000000000000 ),
 .UNSPECIFIED. ) 
 GEOMETRIC_REPRESENTATION_ITEM ( )  RATIONAL_B_SPLINE_SURFACE ( (
 ( 1.000000000000000000, 1.000000000000000000),
 ( 0.3333333333333335369, 0.3333333333333330373),
 ( 0.3333333333333335369, 0.3333333333333330373),
 ( 1.000000000000000000, 1.000000000000000000),
 ( 0.3333333333333333703, 0.3333333333333333703),
 ( 0.3333333333333333703, 0.3333333333333333703),
 ( 1.000000000000000000, 1.000000000000000000) ) ) 
 REPRESENTATION_ITEM ( '' )  SURFACE ( )  );
#26777 = CARTESIAN_POINT ( 'NONE',  ( -12.13372751330810928, -16.36162385676421493, 53.88362224778185805 ) ) ;
#26778 = CARTESIAN_POINT ( 'NONE',  ( -10.52991759648590531, -16.02177972226642311, 68.27767831073917648 ) ) ;
#26779 = VECTOR ( 'NONE', #5356, 1000.000000000000000 ) ;
#26780 = LINE ( 'NONE', #5097, #31531 ) ;
#26781 = VERTEX_POINT ( 'NONE', #9600 ) ;
#26782 = ADVANCED_FACE ( 'NONE', ( #17189 ), #47258, .T. ) ;
#26783 = B_SPLINE_CURVE_WITH_KNOTS ( 'NONE', 3,
 ( #8099, #45045, #41572, #45995, #20624, #31451, #46234, #23594, #38595, #4882 ),
 .UNSPECIFIED., .F., .F.,
 ( 4, 2, 2, 2, 4 ),
 ( 0.1272669073658330152, 0.2522669073463136846, 0.3772669073267943540, 0.5022669073072749679, 0.6272669072877556928 ),
 .UNSPECIFIED. ) ;
#26784 = CARTESIAN_POINT ( 'NONE',  ( -17.29284385650551670, -7.406986770994973490, 48.81910596585309747 ) ) ;
#26785 = VERTEX_POINT ( 'NONE', #44531 ) ;
#26786 = CARTESIAN_POINT ( 'NONE',  ( -10.62512194321859127, -12.94411275245784410, 67.74392152479347828 ) ) ;
#26787 = CARTESIAN_POINT ( 'NONE',  ( -15.29809733969474195, -21.47854975192407778, 68.87592918283094434 ) ) ;
#26788 = CARTESIAN_POINT ( 'NONE',  ( -15.22349691269893057, -21.45476926339652479, 68.59209542689700356 ) ) ;
#26789 = EDGE_LOOP ( 'NONE', ( #8383, #40122, #7469, #40055, #23453 ) ) ;
#26790 = DIRECTION ( 'NONE',  ( 0.9687793358424821033, -0.2479245821708677133, 0.000000000000000000 ) ) ;
#26791 = CARTESIAN_POINT ( 'NONE',  ( -10.60264614768167846, -13.01441009583156472, 64.47655987029209257 ) ) ;
#26792 = CARTESIAN_POINT ( 'NONE',  ( -22.84088606172599967, -19.92422106693271999, 72.80433942285431215 ) ) ;
#26793 = B_SPLINE_CURVE_WITH_KNOTS ( 'NONE', 3,
 ( #469, #23121, #235, #26314, #41331, #45290, #33675, #15448, #11538, #7620 ),
 .UNSPECIFIED., .F., .F.,
 ( 4, 2, 2, 2, 4 ),
 ( 0.000000000000000000, 0.2500000000000000000, 0.5000000000000000000, 0.7500000000000000000, 1.000000000000000000 ),
 .UNSPECIFIED. ) ;
#26794 = EDGE_CURVE ( 'NONE', #44919, #38482, #16395, .T. ) ;
#26795 = AXIS2_PLACEMENT_3D ( 'NONE', #15883, #30928, #23783 ) ;
#26796 = ORIENTED_EDGE ( 'NONE', *, *, #3898, .F. ) ;
#26797 = CARTESIAN_POINT ( 'NONE',  ( -50.42609385541305755, -14.80920654474411613, 58.90588235294116970 ) ) ;
#26798 = EDGE_CURVE ( 'NONE', #47056, #48460, #34576, .T. ) ;
#26799 = DIRECTION ( 'NONE',  ( 0.6408936281290997794, 0.7676297007174212039, 4.260501105223829885E-08 ) ) ;
#26800 = VERTEX_POINT ( 'NONE', #26063 ) ;
#26801 = DIRECTION ( 'NONE',  ( 3.071710424422018668E-17, -6.404604876783312462E-16, -1.000000000000000000 ) ) ;
#26802 = AXIS2_PLACEMENT_3D ( 'NONE', #7288, #33849, #40752 ) ;
#26803 = ORIENTED_EDGE ( 'NONE', *, *, #7232, .F. ) ;
#26804 = FACE_OUTER_BOUND ( 'NONE', #43901, .T. ) ;
#26805 = PRODUCT_DEFINITION_SHAPE ( 'NONE', 'NONE',  #16839 ) ;
#26806 = CARTESIAN_POINT ( 'NONE',  ( -12.36794914932409561, -19.72224030764921565, 61.39678633597973345 ) ) ;
#26807 = EDGE_CURVE ( 'NONE', #34499, #7578, #31899, .T. ) ;
#26808 = VERTEX_POINT ( 'NONE', #34582 ) ;
#26809 = DIRECTION ( 'NONE',  ( -0.3668819201507741989, 0.9245033139891488672, 0.1033986416233889649 ) ) ;
#26810 = DIRECTION ( 'NONE',  ( -1.261798974855884165E-05, 2.391811520720373553E-06, -0.9999999999175327448 ) ) ;
#26811 = CARTESIAN_POINT ( 'NONE',  ( -21.99213670719075253, -20.17946569659695299, 59.04970794435396897 ) ) ;
#26812 = ORIENTED_EDGE ( 'NONE', *, *, #6866, .T. ) ;
#26813 = AXIS2_PLACEMENT_3D ( 'NONE', #27496, #34633, #15913 ) ;
#26814 = UNCERTAINTY_MEASURE_WITH_UNIT (LENGTH_MEASURE( 1.000000000000000082E-05 ), #11559, 'distance_accuracy_value', 'NONE');
#26815 = EDGE_CURVE ( 'NONE', #12408, #35856, #19682, .T. ) ;
#26816 = CARTESIAN_POINT ( 'NONE',  ( -19.67760665824181388, -21.48965406232008490, 65.75014118398131302 ) ) ;
#26817 = DIRECTION ( 'NONE',  ( 0.3374354101627464186, 0.9413486835218386473, 1.423378189492272593E-08 ) ) ;
#26818 = B_SPLINE_CURVE_WITH_KNOTS ( 'NONE', 3,
 ( #34552, #31354, #8721, #46384, #15585, #34302, #34803, #38003, #4060, #23493 ),
 .UNSPECIFIED., .F., .F.,
 ( 4, 2, 2, 2, 4 ),
 ( 0.000000000000000000, 0.2500000000000000000, 0.5000000000000000000, 0.7500000000000000000, 1.000000000000000000 ),
 .UNSPECIFIED. ) ;
#26819 = ORIENTED_EDGE ( 'NONE', *, *, #34675, .T. ) ;
#26820 = CARTESIAN_POINT ( 'NONE',  ( -12.05451961919647630, -9.643808529799599683, 57.20280282899455671 ) ) ;
#26821 = CARTESIAN_POINT ( 'NONE',  ( -21.01124108229941001, -20.87838065962769463, 65.88453944495783787 ) ) ;
#26823 = VERTEX_POINT ( 'NONE', #22125 ) ;
#26822 = CIRCLE ( 'NONE', #40939, 2.000000000000000000 ) ;
#26824 = ORIENTED_EDGE ( 'NONE', *, *, #11648, .F. ) ;
#26825 = CARTESIAN_POINT ( 'NONE',  ( -24.84978522997450767, -14.20774122709759801, 69.75251648635047275 ) ) ;
#26826 = DIRECTION ( 'NONE',  ( -1.000000000000000000, 2.276824562219560297E-16, 0.000000000000000000 ) ) ;
#26827 = CARTESIAN_POINT ( 'NONE',  ( -21.76006473383504414, -8.751000872772104699, 70.28132536106762984 ) ) ;
#26828 = CARTESIAN_POINT ( 'NONE',  ( -20.89284385650552167, -7.406986770994973490, 48.81910596585309747 ) ) ;
#26829 = LINE ( 'NONE', #30530, #4686 ) ;
#26830 = CARTESIAN_POINT ( 'NONE',  ( -12.12077823425219414, -9.576857651715958042, 57.28924319034693013 ) ) ;
#26831 = CARTESIAN_POINT ( 'NONE',  ( -23.98503169607928953, -17.39005800936845603, 66.22885190747201989 ) ) ;
#26832 = CARTESIAN_POINT ( 'NONE',  ( -9.975093145215874202, -14.93635225021824198, 74.98274299234972773 ) ) ;
#26833 = ORIENTED_EDGE ( 'NONE', *, *, #14134, .F. ) ;
#26834 = AXIS2_PLACEMENT_3D ( 'NONE', #20896, #31977, #35891 ) ;
#26835 =( NAMED_UNIT ( * ) PLANE_ANGLE_UNIT ( ) SI_UNIT ( $, .RADIAN. ) );
#26836 = CIRCLE ( 'NONE', #5606, 7.500000000000001776 ) ;
#26837 = DIRECTION ( 'NONE',  ( -1.143861050413982909E-05, 2.837703136207094791E-06, -0.9999999999305527743 ) ) ;
#26838 = CARTESIAN_POINT ( 'NONE',  ( -18.52460027084869765, -7.842592186127370191, 70.25579138408188840 ) ) ;
#26839 = EDGE_CURVE ( 'NONE', #41762, #11480, #48702, .T. ) ;
#26840 = AXIS2_PLACEMENT_3D ( 'NONE', #16599, #34831, #34585 ) ;
#26841 = ORIENTED_EDGE ( 'NONE', *, *, #29431, .T. ) ;
#26842 = ORIENTED_EDGE ( 'NONE', *, *, #14617, .F. ) ;
#26843 = CARTESIAN_POINT ( 'NONE',  ( -36.42409385541304800, -6.859212275519750435, 50.50378509014258555 ) ) ;
#26844 = CARTESIAN_POINT ( 'NONE',  ( -10.70532053225239544, -12.67267096592666498, 61.08381491717225487 ) ) ;
#26845 = CARTESIAN_POINT ( 'NONE',  ( -11.69223540468882838, -10.05010615616768810, 67.60558564255768488 ) ) ;
#26846 = FACE_OUTER_BOUND ( 'NONE', #44523, .T. ) ;
#26847 = CIRCLE ( 'NONE', #40232, 2.404255319148937531 ) ;
#26848 =( BOUNDED_CURVE ( )  B_SPLINE_CURVE ( 3, ( #2866, #44026, #36830, #47692 ),
 .UNSPECIFIED., .F., .F. ) 
 B_SPLINE_CURVE_WITH_KNOTS ( ( 4, 4 ),
 ( 0.9074455897393659543, 1.000000000000000000 ),
 .UNSPECIFIED. ) 
 CURVE ( )  GEOMETRIC_REPRESENTATION_ITEM ( )  RATIONAL_B_SPLINE_CURVE ( ( 0.6983129098260867362, 0.7760317562606927622, 0.8765941196519971834, 1.000000000000000000 ) ) 
 REPRESENTATION_ITEM ( '' )  );
#26849 = ORIENTED_EDGE ( 'NONE', *, *, #37359, .F. ) ;
#26850 = EDGE_CURVE ( 'NONE', #36512, #30726, #9622, .T. ) ;
#26851 = CARTESIAN_POINT ( 'NONE',  ( -13.05823701642829882, -9.336965241264831405, 71.13308820894700091 ) ) ;
#26852 = DIRECTION ( 'NONE',  ( 2.201155577252676169E-06, 7.355553122608190330E-06, 0.9999999999705252440 ) ) ;
#26853 = AXIS2_PLACEMENT_3D ( 'NONE', #32425, #47446, #28724 ) ;
#26854 = ORIENTED_EDGE ( 'NONE', *, *, #32635, .T. ) ;
#26855 = ADVANCED_FACE ( 'NONE', ( #29753 ), #30000, .T. ) ;
#26856 = CARTESIAN_POINT ( 'NONE',  ( -10.96921284960095377, -11.97350354382807680, 74.84368195529052059 ) ) ;
#26857 = CARTESIAN_POINT ( 'NONE',  ( -22.09360125616737136, -20.02631309226648781, 65.89348735000095303 ) ) ;
#26858 =( BOUNDED_CURVE ( )  B_SPLINE_CURVE ( 3, ( #13763, #46571, #28573, #47034 ),
 .UNSPECIFIED., .F., .F. ) 
 B_SPLINE_CURVE_WITH_KNOTS ( ( 4, 4 ),
 ( 0.5000000000000000000, 0.9074455897393687298 ),
 .UNSPECIFIED. ) 
 CURVE ( )  GEOMETRIC_REPRESENTATION_ITEM ( )  RATIONAL_B_SPLINE_CURVE ( ( 1.000000000000017542, 0.4567392136813246406, 0.3561768502900152789, 0.6983129098261083856 ) ) 
 REPRESENTATION_ITEM ( '' )  );
#26859 = ORIENTED_EDGE ( 'NONE', *, *, #43624, .T. ) ;
#26860 =( BOUNDED_CURVE ( )  B_SPLINE_CURVE ( 3, ( #28307, #25332, #5893, #6616 ),
 .UNSPECIFIED., .F., .F. ) 
 B_SPLINE_CURVE_WITH_KNOTS ( ( 4, 4 ),
 ( 0.9074455897393722825, 1.000000000000000000 ),
 .UNSPECIFIED. ) 
 CURVE ( )  GEOMETRIC_REPRESENTATION_ITEM ( )  RATIONAL_B_SPLINE_CURVE ( ( 0.6983129098261113832, 0.7760317562607140784, 0.8765941196520102840, 1.000000000000000000 ) ) 
 REPRESENTATION_ITEM ( '' )  );
#26861 = CARTESIAN_POINT ( 'NONE',  ( -19.94917705995926482, -8.226604131702123013, 74.00624557436877637 ) ) ;
#26862 = ORIENTED_EDGE ( 'NONE', *, *, #10650, .T. ) ;
#26863 = CARTESIAN_POINT ( 'NONE',  ( -26.22630854578367021, -13.51651355179587632, 53.49999999999995026 ) ) ;
#26864 = EDGE_CURVE ( 'NONE', #28015, #47684, #28461, .T. ) ;
#26866 = CARTESIAN_POINT ( 'NONE',  ( -13.10965166868813903, -12.97921450448603409, 49.52966884056655772 ) ) ;
#26865 = AXIS2_PLACEMENT_3D ( 'NONE', #8253, #23269, #3823 ) ;
#26867 = VERTEX_POINT ( 'NONE', #37111 ) ;
#26868 = DIRECTION ( 'NONE',  ( -3.071710424422018668E-17, 6.404604876783312462E-16, 1.000000000000000000 ) ) ;
#26869 = CARTESIAN_POINT ( 'NONE',  ( -24.32493921937862424, -13.34866582089179055, 63.13264457041533007 ) ) ;
#26870 = CARTESIAN_POINT ( 'NONE',  ( -15.74909385650551386, -8.104110260919579645, 48.81699501597546487 ) ) ;
#26871 = CONICAL_SURFACE ( 'NONE', #20581, 0.5560000000000009379, 0.06981317007976595157 ) ;
#26872 = CARTESIAN_POINT ( 'NONE',  ( -17.86643179882426935, -7.822757671798997947, 60.09677386199297899 ) ) ;
#26873 = EDGE_CURVE ( 'NONE', #5898, #48128, #14593, .T. ) ;
#26874 = CARTESIAN_POINT ( 'NONE',  ( -22.22370946352282672, -9.111183370010303761, 59.90666632495347699 ) ) ;
#26875 = CARTESIAN_POINT ( 'NONE',  ( -14.98297878932515381, -10.79466886532025605, 52.02966884056656482 ) ) ;
#26876 = ORIENTED_EDGE ( 'NONE', *, *, #45699, .T. ) ;
#26877 = CARTESIAN_POINT ( 'NONE',  ( -24.47293982775255472, -15.07115001610720562, 59.54300207942560519 ) ) ;
#26878 =( BOUNDED_SURFACE ( )  B_SPLINE_SURFACE ( 3, 1, ( 
 ( #12801, #46790 ),
 ( #5907, #46310 ),
 ( #2203, #5681 ),
 ( #47278, #13518 ),
 ( #20691, #5432 ),
 ( #27826, #43348 ),
 ( #9619, #42855 ) ),
 .UNSPECIFIED., .T., .F., .F. ) 
 B_SPLINE_SURFACE_WITH_KNOTS ( ( 4, 3, 4 ),
 ( 2, 2 ),
 ( 0.000000000000000000, 0.5000000000000000000, 1.000000000000000000 ),
 ( 0.000000000000000000, 1.000000000000000000 ),
 .UNSPECIFIED. ) 
 GEOMETRIC_REPRESENTATION_ITEM ( )  RATIONAL_B_SPLINE_SURFACE ( (
 ( 1.000000000000000000, 1.000000000000000000),
 ( 0.3333333333333335369, 0.3333333333333330373),
 ( 0.3333333333333335369, 0.3333333333333330373),
 ( 1.000000000000000000, 1.000000000000000000),
 ( 0.3333333333333333703, 0.3333333333333333703),
 ( 0.3333333333333333703, 0.3333333333333333703),
 ( 1.000000000000000000, 1.000000000000000000) ) ) 
 REPRESENTATION_ITEM ( '' )  SURFACE ( )  );
#26879 = CARTESIAN_POINT ( 'NONE',  ( -18.98976565384166193, -12.86018837663894843, 53.27966884056655061 ) ) ;
#26880 = DIRECTION ( 'NONE',  ( 0.9687793358424819923, -0.2479245821708676023, 0.000000000000000000 ) ) ;
#26881 = DIRECTION ( 'NONE',  ( -0.7670373483544791204, -0.6416024518573234525, 2.496223344567222868E-08 ) ) ;
#26882 = CARTESIAN_POINT ( 'NONE',  ( -23.78632397794047648, -18.68536885113667623, 72.96379443305436041 ) ) ;
#26883 = VERTEX_POINT ( 'NONE', #42479 ) ;
#26884 = ORIENTED_EDGE ( 'NONE', *, *, #41307, .T. ) ;
#26885 = CARTESIAN_POINT ( 'NONE',  ( -10.81219955438992741, -11.37622629119364603, 67.76864606346147468 ) ) ;
#26886 = ORIENTED_EDGE ( 'NONE', *, *, #33095, .F. ) ;
#26887 = CIRCLE ( 'NONE', #11945, 5.249999999999998224 ) ;
#26888 = CARTESIAN_POINT ( 'NONE',  ( -16.35985130318476166, -22.18285048229636303, 61.86229803363791291 ) ) ;
#26889 = CARTESIAN_POINT ( 'NONE',  ( -22.72409385759798894, -9.359200813967568422, 50.49621490985803263 ) ) ;
#26890 = FACE_OUTER_BOUND ( 'NONE', #41571, .T. ) ;
#26891 = EDGE_CURVE ( 'NONE', #25305, #21669, #43561, .T. ) ;
#26892 = CARTESIAN_POINT ( 'NONE',  ( -11.35824856342118316, -11.21643317443627197, 60.97885780702566905 ) ) ;
#26893 = CARTESIAN_POINT ( 'NONE',  ( -22.10120296142702045, -17.19398125327358073, 52.02966884056656482 ) ) ;
#26894 = EDGE_CURVE ( 'NONE', #47558, #16040, #25945, .T. ) ;
#26895 = DIRECTION ( 'NONE',  ( 0.7700094066334515208, 0.6380325334150288574, 0.000000000000000000 ) ) ;
#26896 = ORIENTED_EDGE ( 'NONE', *, *, #4999, .T. ) ;
#26897 = PLANE ( 'NONE',  #31227 ) ;
#26898 = EDGE_CURVE ( 'NONE', #4886, #13644, #42222, .T. ) ;
#26899 = DIRECTION ( 'NONE',  ( 0.000000000000000000, 0.000000000000000000, 1.000000000000000000 ) ) ;
#26900 = CARTESIAN_POINT ( 'NONE',  ( -13.77834422207524412, -20.78674875190709415, 68.64552295153497141 ) ) ;
#26901 = CARTESIAN_POINT ( 'NONE',  ( -19.77500964849970799, -21.45962299806434359, 72.70478730350133389 ) ) ;
#26902 = CARTESIAN_POINT ( 'NONE',  ( -17.91414045948978639, -21.84516348726148394, 65.76020891215902964 ) ) ;
#26903 = VERTEX_POINT ( 'NONE', #14682 ) ;
#26904 = VERTEX_POINT ( 'NONE', #46163 ) ;
#26905 = VECTOR ( 'NONE', #20113, 1000.000000000000000 ) ;
#26906 = ORIENTED_EDGE ( 'NONE', *, *, #8371, .T. ) ;
#26907 = CARTESIAN_POINT ( 'NONE',  ( -11.41947236009895228, -18.50911967460687535, 65.16195962094886340 ) ) ;
#26908 = AXIS2_PLACEMENT_3D ( 'NONE', #43120, #39425, #46814 ) ;
#26909 = CARTESIAN_POINT ( 'NONE',  ( -16.54784415797146480, -21.75414618367045350, 61.94671215975959910 ) ) ;
#26910 = CARTESIAN_POINT ( 'NONE',  ( -13.66784385759799036, -9.357632978295827186, 49.97845033065683396 ) ) ;
#26911 = CARTESIAN_POINT ( 'NONE',  ( -17.45593231491017505, -7.751306502474292870, 60.23627933525208533 ) ) ;
#26912 = ORIENTED_EDGE ( 'NONE', *, *, #432, .F. ) ;
#26913 = CARTESIAN_POINT ( 'NONE',  ( -17.79108452803360763, -21.84994637594637368, 58.69081321602850920 ) ) ;
#26914 = CARTESIAN_POINT ( 'NONE',  ( -21.89130958583942288, -9.354787850460871468, 63.20625856529903075 ) ) ;
#26915 = ORIENTED_EDGE ( 'NONE', *, *, #44137, .F. ) ;
#26916 = CARTESIAN_POINT ( 'NONE',  ( -19.20714268997449281, -19.15619313305651161, 49.52966884056656482 ) ) ;
#26917 = CARTESIAN_POINT ( 'NONE',  ( -12.20309422964675150, -20.12380354524033521, 64.98179449731530610 ) ) ;
#26918 = EDGE_LOOP ( 'NONE', ( #2152, #40088, #48256, #37362, #1159 ) ) ;
#26919 = LINE ( 'NONE', #7730, #25233 ) ;
#26920 = CARTESIAN_POINT ( 'NONE',  ( -22.18815592092731137, -20.53689392896745503, 58.86468654123366662 ) ) ;
#26921 = ADVANCED_FACE ( 'NONE', ( #36868 ), #3152, .T. ) ;
#26922 = CARTESIAN_POINT ( 'NONE',  ( -12.84615363328625648, -20.17103110633857455, 72.09181604382622766 ) ) ;
#26923 = ORIENTED_EDGE ( 'NONE', *, *, #36523, .F. ) ;
#26924 = CARTESIAN_POINT ( 'NONE',  ( -19.64493829067500030, -21.44926303942544266, 69.12409502726751498 ) ) ;
#26925 = CARTESIAN_POINT ( 'NONE',  ( -23.03238438629518114, -19.08140394072652768, 59.17850838485211540 ) ) ;
#26926 = CARTESIAN_POINT ( 'NONE',  ( -11.55573786329523855, -10.21941616939416342, 71.15388509157428132 ) ) ;
#26927 = DIRECTION ( 'NONE',  ( 1.000000000000000000, 0.000000000000000000, 0.000000000000000000 ) ) ;
#26928 = EDGE_LOOP ( 'NONE', ( #23379, #17006, #2308, #1041, #3353 ) ) ;
#26929 = DIRECTION ( 'NONE',  ( -1.474291233076046698E-06, -1.298191854940810726E-06, 0.9999999999980706544 ) ) ;
#26930 = CARTESIAN_POINT ( 'NONE',  ( -43.17409385541305511, -14.80920654474410547, 56.99999999999998579 ) ) ;
#26931 = CARTESIAN_POINT ( 'NONE',  ( -13.76038152179329543, -18.92930211169645105, 53.69233794759168887 ) ) ;
#26932 = CARTESIAN_POINT ( 'NONE',  ( -12.50766595982653584, -19.86205097402751463, 65.01674886870775083 ) ) ;
#26933 = CYLINDRICAL_SURFACE ( 'NONE', #33844, 1.999999999999999112 ) ;
#26934 = CARTESIAN_POINT ( 'NONE',  ( -19.71159385650551599, -6.922745924619793101, 51.69366785382590024 ) ) ;
#26935 = VERTEX_POINT ( 'NONE', #29498 ) ;
#26936 = CARTESIAN_POINT ( 'NONE',  ( -26.42409385541305511, -6.859206544744110623, 47.99999999999997868 ) ) ;
#26937 = CARTESIAN_POINT ( 'NONE',  ( -11.03230881600246427, -10.98182333549695322, 60.79390388117851529 ) ) ;
#26938 = ORIENTED_EDGE ( 'NONE', *, *, #23450, .F. ) ;
#26939 = CARTESIAN_POINT ( 'NONE',  ( -22.94085508618206859, -9.802298960702817254, 70.19673832247809742 ) ) ;
#26940 = CARTESIAN_POINT ( 'NONE',  ( -10.76785811675246940, -12.48515291162924434, 57.61385273545094066 ) ) ;
#26941 = ORIENTED_EDGE ( 'NONE', *, *, #19226, .T. ) ;
#26942 = CARTESIAN_POINT ( 'NONE',  ( -10.37599212182869124, -14.63324797960940593, 71.34254748307667171 ) ) ;
#26943 = EDGE_CURVE ( 'NONE', #7654, #45579, #17521, .T. ) ;
#26944 = CARTESIAN_POINT ( 'NONE',  ( -24.42401385028228589, -14.76496886756241622, 59.25802720181223293 ) ) ;
#26945 = CARTESIAN_POINT ( 'NONE',  ( -24.03316043928017720, -11.37042366253971259, 66.58361025287214829 ) ) ;
#26946 = EDGE_CURVE ( 'NONE', #12909, #43562, #2870, .T. ) ;
#26947 = EDGE_CURVE ( 'NONE', #27374, #1012, #45147, .T. ) ;
#26948 = ORIENTED_EDGE ( 'NONE', *, *, #42546, .T. ) ;
#26949 = CARTESIAN_POINT ( 'NONE',  ( -14.98659385650551457, -9.302874398569244363, 51.68646062012417985 ) ) ;
#26950 =( BOUNDED_CURVE ( )  B_SPLINE_CURVE ( 3, ( #2849, #6563, #10007, #32653 ),
 .UNSPECIFIED., .F., .F. ) 
 B_SPLINE_CURVE_WITH_KNOTS ( ( 4, 4 ),
 ( 0.9074455897393647330, 1.000000000000000000 ),
 .UNSPECIFIED. ) 
 CURVE ( )  GEOMETRIC_REPRESENTATION_ITEM ( )  RATIONAL_B_SPLINE_CURVE ( ( 0.6983129098260990597, 0.7760317562607034203, 0.8765941196520037337, 1.000000000000000000 ) ) 
 REPRESENTATION_ITEM ( '' )  );
#26951 = CARTESIAN_POINT ( 'NONE',  ( -12.89750100592999971, -8.892007198426925996, 67.48668646829932527 ) ) ;
#26952 = LINE ( 'NONE', #848, #24553 ) ;
#26953 = CARTESIAN_POINT ( 'NONE',  ( -23.26206559395185991, -18.76176001737956511, 66.11829607788916974 ) ) ;
#26954 = CARTESIAN_POINT ( 'NONE',  ( -23.12773592331248551, -18.86744558261350946, 62.36909269548800694 ) ) ;
#26955 = VERTEX_POINT ( 'NONE', #12903 ) ;
#26956 = VERTEX_POINT ( 'NONE', #17322 ) ;
#26957 = CARTESIAN_POINT ( 'NONE',  ( -22.52409385541304232, -9.359200813967568422, 50.49621490985803263 ) ) ;
#26958 = CARTESIAN_POINT ( 'NONE',  ( -24.14679772577363437, -12.68507108172156705, 70.05770892828130059 ) ) ;
#26959 =( NAMED_UNIT ( * ) SI_UNIT ( $, .STERADIAN. ) SOLID_ANGLE_UNIT ( ) );
#26960 = DIRECTION ( 'NONE',  ( 0.9687793358424821033, -0.2479245821708679909, 0.000000000000000000 ) ) ;
#26961 = EDGE_CURVE ( 'NONE', #30371, #22574, #41661, .T. ) ;
#26962 = FACE_OUTER_BOUND ( 'NONE', #22784, .T. ) ;
#26963 = CARTESIAN_POINT ( 'NONE',  ( -20.12437885760196110, -7.865711196993452781, 73.76450701231766516 ) ) ;
#26964 = CARTESIAN_POINT ( 'NONE',  ( -17.79490377976783932, -14.65920654474411045, 48.99999999999997868 ) ) ;
#26965 = ORIENTED_EDGE ( 'NONE', *, *, #34543, .T. ) ;
#26966 = CARTESIAN_POINT ( 'NONE',  ( -10.82867520472564848, -11.34449427682889677, 67.73369198428547122 ) ) ;
#26967 = ORIENTED_EDGE ( 'NONE', *, *, #32406, .T. ) ;
#26968 = CARTESIAN_POINT ( 'NONE',  ( -12.56078782956467421, -9.165549844850980676, 74.51934210929164237 ) ) ;
#26969 = DIRECTION ( 'NONE',  ( -3.071710424422018668E-17, 6.404604876783312462E-16, 1.000000000000000000 ) ) ;
#26970 = CARTESIAN_POINT ( 'NONE',  ( -24.41597802456916710, -17.38151951243146698, 69.52001501703639974 ) ) ;
#26971 = DIRECTION ( 'NONE',  ( -5.731567514496413899E-31, -1.020425574103664789E-16, -1.000000000000000000 ) ) ;
#26972 = EDGE_LOOP ( 'NONE', ( #27787, #28137, #7251, #42234, #27981 ) ) ;
#26973 = CARTESIAN_POINT ( 'NONE',  ( -13.08575159502176177, -11.85263988192353324, 52.02966884056656482 ) ) ;
#26974 = CARTESIAN_POINT ( 'NONE',  ( -6.424093855413055110, -25.10920654474410441, 79.99999999999998579 ) ) ;
#26975 = CARTESIAN_POINT ( 'NONE',  ( -13.54823245630065998, -20.69819609872914157, 61.81646323537677290 ) ) ;
#26976 = CARTESIAN_POINT ( 'NONE',  ( -20.86878983561329548, -8.203218349707368517, 60.00158597527717319 ) ) ;
#26977 = ORIENTED_EDGE ( 'NONE', *, *, #43931, .T. ) ;
#26978 = CARTESIAN_POINT ( 'NONE',  ( -18.60463909989377385, -22.16515503909319307, 72.32864992405023941 ) ) ;
#26979 = DIRECTION ( 'NONE',  ( -1.209056809376604527E-06, -5.657077721962264774E-07, -0.9999999999991091570 ) ) ;
#26980 = DIRECTION ( 'NONE',  ( -0.9757441136919988711, -0.2189141945955436208, 0.000000000000000000 ) ) ;
#26981 = DIRECTION ( 'NONE',  ( -0.9087012777736582780, 0.4174469879787381932, 4.853707507795134418E-09 ) ) ;
#26982 = PRODUCT_CONTEXT ( 'NONE', #34083, 'mechanical' ) ;
#26983 = FACE_OUTER_BOUND ( 'NONE', #37686, .T. ) ;
#26984 = LINE ( 'NONE', #42009, #44428 ) ;
#26985 = LINE ( 'NONE', #5744, #37574 ) ;
#26986 = LINE ( 'NONE', #35086, #9381 ) ;
#26987 = EDGE_LOOP ( 'NONE', ( #37511, #35038, #7198, #42306 ) ) ;
#26988 = LINE ( 'NONE', #19598, #30810 ) ;
#26989 = VERTEX_POINT ( 'NONE', #32119 ) ;
#26990 = CARTESIAN_POINT ( 'NONE',  ( -11.79630000206883977, -19.05592701419838519, 71.97213747039440079 ) ) ;
#26991 = CARTESIAN_POINT ( 'NONE',  ( -20.78451513435706133, -21.00713107796517320, 62.12943504870421663 ) ) ;
#26992 =( BOUNDED_CURVE ( )  B_SPLINE_CURVE ( 3, ( #48234, #14241, #33200, #40853 ),
 .UNSPECIFIED., .F., .F. ) 
 B_SPLINE_CURVE_WITH_KNOTS ( ( 4, 4 ),
 ( 0.000000000000000000, 0.4074455897393673975 ),
 .UNSPECIFIED. ) 
 CURVE ( )  GEOMETRIC_REPRESENTATION_ITEM ( )  RATIONAL_B_SPLINE_CURVE ( ( 1.000000000000000000, 0.4567392136813311909, 0.3561768502900300448, 0.6983129098260966172 ) ) 
 REPRESENTATION_ITEM ( '' )  );
#26993 = ORIENTED_EDGE ( 'NONE', *, *, #37704, .F. ) ;
#26994 = FACE_BOUND ( 'NONE', #13559, .T. ) ;
#26995 = ORIENTED_EDGE ( 'NONE', *, *, #30174, .F. ) ;
#26996 = ADVANCED_FACE ( 'NONE', ( #43206 ), #24010, .T. ) ;
#26997 = ORIENTED_EDGE ( 'NONE', *, *, #46210, .F. ) ;
#26998 = ORIENTED_EDGE ( 'NONE', *, *, #11267, .T. ) ;
#26999 = FACE_OUTER_BOUND ( 'NONE', #27469, .T. ) ;
#27000 = CARTESIAN_POINT ( 'NONE',  ( -21.91688961498890720, -8.866358848214497712, 66.76126358204035682 ) ) ;
#27001 = CARTESIAN_POINT ( 'NONE',  ( -16.50613596612109646, -22.20251566029174128, 65.48210330380625521 ) ) ;
#27002 = CARTESIAN_POINT ( 'NONE',  ( -13.01353307917097268, -8.804980454159759162, 64.09441913135431435 ) ) ;
#27003 = CARTESIAN_POINT ( 'NONE',  ( -13.60238289842206072, -8.884932333444998775, 57.26967755503795843 ) ) ;
#27004 = CARTESIAN_POINT ( 'NONE',  ( -19.93659385541302953, -8.995762431863228770, 51.38120296130586695 ) ) ;
#27005 =( BOUNDED_CURVE ( )  B_SPLINE_CURVE ( 3, ( #35367, #21334, #36325, #24552 ),
 .UNSPECIFIED., .F., .F. ) 
 B_SPLINE_CURVE_WITH_KNOTS ( ( 4, 4 ),
 ( 0.000000000000000000, 0.4074455897393594594 ),
 .UNSPECIFIED. ) 
 CURVE ( )  GEOMETRIC_REPRESENTATION_ITEM ( )  RATIONAL_B_SPLINE_CURVE ( ( 1.000000000000000000, 0.4567392136813387404, 0.3561768502900328204, 0.6983129098260824064 ) ) 
 REPRESENTATION_ITEM ( '' )  );
#27006 = ORIENTED_EDGE ( 'NONE', *, *, #23814, .F. ) ;
#27007 = ORIENTED_EDGE ( 'NONE', *, *, #1495, .F. ) ;
#27008 = EDGE_CURVE ( 'NONE', #4981, #39185, #31674, .T. ) ;
#27009 = EDGE_CURVE ( 'NONE', #29759, #35234, #13622, .T. ) ;
#27010 = CARTESIAN_POINT ( 'NONE',  ( -16.16063142123006813, -7.467037929575190525, 60.38523757159160965 ) ) ;
#27011 = EDGE_CURVE ( 'NONE', #46585, #17249, #28664, .T. ) ;
#27012 = CARTESIAN_POINT ( 'NONE',  ( -11.83709238739359648, -9.880916174117215789, 64.22903110108937597 ) ) ;
#27013 = FACE_OUTER_BOUND ( 'NONE', #27594, .T. ) ;
#27014 = CARTESIAN_POINT ( 'NONE',  ( -19.67368922737015424, -21.43794379858934107, 65.47988644745025510 ) ) ;
#27015 = EDGE_CURVE ( 'NONE', #7024, #47122, #28430, .T. ) ;
#27016 = EDGE_LOOP ( 'NONE', ( #30072, #25716, #7160, #10337, #4875, #10129, #42077, #42762, #24150, #15080, #22848, #44756, #30622, #38296, #14088, #41686, #32068, #4074, #38703, #42255, #26078, #41192, #21059, #41081, #26623, #10677, #35887, #47483, #38330, #31388, #46826, #23915, #22893, #16538, #46198, #48002, #13654, #31175, #8630, #665, #30954, #22041, #13079, #44538, #21830, #16440, #32524, #25587, #31332, #5224, #26912, #35916, #13106, #5370, #4891, #35485, #20641, #35192, #30004, #39147, #40743, #38016, #28041, #47947, #10898, #16157, #44840, #17922, #9314, #3312, #12557, #13544 ) ) ;
#27017 = CARTESIAN_POINT ( 'NONE',  ( -17.12409385650551741, -6.426201560718813433, 50.50509628382439331 ) ) ;
#27018 = ORIENTED_EDGE ( 'NONE', *, *, #48131, .T. ) ;
#27019 = CARTESIAN_POINT ( 'NONE',  ( -16.20683845212634111, -21.70255763714999020, 58.58585572420326315 ) ) ;
#27020 = EDGE_CURVE ( 'NONE', #40074, #35620, #44035, .T. ) ;
#27021 = LINE ( 'NONE', #4867, #6436 ) ;
#27022 = VECTOR ( 'NONE', #25626, 1000.000000000000227 ) ;
#27023 = CARTESIAN_POINT ( 'NONE',  ( -17.26224459804799238, -7.811016595343872382, 67.24713020387331142 ) ) ;
#27024 = ORIENTED_EDGE ( 'NONE', *, *, #22653, .T. ) ;
#27025 = CARTESIAN_POINT ( 'NONE',  ( -13.40955617598886995, -17.25032161083215598, 52.02966884056656482 ) ) ;
#27026 = CARTESIAN_POINT ( 'NONE',  ( -11.33476804054750531, -19.10151225439055978, 68.40184904730287485 ) ) ;
#27027 = DIRECTION ( 'NONE',  ( -3.071710424422018668E-17, 6.404604876783312462E-16, 1.000000000000000000 ) ) ;
#27028 = ORIENTED_EDGE ( 'NONE', *, *, #6855, .T. ) ;
#27029 = LINE ( 'NONE', #5355, #45440 ) ;
#27030 = CARTESIAN_POINT ( 'NONE',  ( -24.83263378688676326, -15.59489965655864374, 73.18799144572807336 ) ) ;
#27031 = DIRECTION ( 'NONE',  ( -1.000000000000000000, 4.164305804376849172E-17, -1.614929280266638808E-16 ) ) ;
#27032 = VERTEX_POINT ( 'NONE', #16597 ) ;
#27033 = CARTESIAN_POINT ( 'NONE',  ( -10.01440776720603765, -14.03439672543145988, 61.03325998023760235 ) ) ;
#27034 = ORIENTED_EDGE ( 'NONE', *, *, #28165, .T. ) ;
#27035 = DIRECTION ( 'NONE',  ( -5.731567514496413899E-31, -1.020425574103664789E-16, -1.000000000000000000 ) ) ;
#27036 = LINE ( 'NONE', #23597, #5222 ) ;
#27037 = ORIENTED_EDGE ( 'NONE', *, *, #14610, .T. ) ;
#27038 = DIRECTION ( 'NONE',  ( 1.075201461790892195E-05, -1.608194661606879754E-06, -0.9999999999409039386 ) ) ;
#27039 = CARTESIAN_POINT ( 'NONE',  ( -7.540694356433003342, -14.17955609235691661, 53.49999999999995026 ) ) ;
#27040 = CARTESIAN_POINT ( 'NONE',  ( 8.575906144586950219, 1.610468034064642007, 60.52947785690135163 ) ) ;
#27041 = ORIENTED_EDGE ( 'NONE', *, *, #3169, .T. ) ;
#27042 = CARTESIAN_POINT ( 'NONE',  ( -50.42609385541305755, -14.90920654474427565, 73.09411764705880898 ) ) ;
#27043 = EDGE_CURVE ( 'NONE', #47792, #11232, #9229, .T. ) ;
#27044 = CARTESIAN_POINT ( 'NONE',  ( -16.40208429260315626, -7.882922619732885217, 60.42858434934230871 ) ) ;
#27045 = CARTESIAN_POINT ( 'NONE',  ( -12.55296927903122040, -9.172306255172346212, 74.46923003722106671 ) ) ;
#27046 = EDGE_LOOP ( 'NONE', ( #14189, #4960, #25355, #852, #28937 ) ) ;
#27047 = CARTESIAN_POINT ( 'NONE',  ( -12.17725024227025621, -10.08844384719822429, 57.24502831558379512 ) ) ;
#27048 = AXIS2_PLACEMENT_3D ( 'NONE', #2807, #48348, #43712 ) ;
#27049 = B_SPLINE_CURVE_WITH_KNOTS ( 'NONE', 1,
 ( #33498, #6702 ),
 .UNSPECIFIED., .F., .F.,
 ( 2, 2 ),
 ( 0.000000000000000000, 1.000000000000000000 ),
 .UNSPECIFIED. ) ;
#27050 = CARTESIAN_POINT ( 'NONE',  ( -23.29040906673546729, -19.40173929881165193, 59.02377295306128957 ) ) ;
#27051 = EDGE_CURVE ( 'NONE', #10001, #10295, #24998, .T. ) ;
#27052 = AXIS2_PLACEMENT_3D ( 'NONE', #42249, #23542, #46430 ) ;
#27053 = ORIENTED_EDGE ( 'NONE', *, *, #15245, .T. ) ;
#27054 = ORIENTED_EDGE ( 'NONE', *, *, #35171, .T. ) ;
#27055 = CARTESIAN_POINT ( 'NONE',  ( -24.84733312566341823, -14.17682965153389674, 69.82992173574167794 ) ) ;
#27056 = CARTESIAN_POINT ( 'NONE',  ( -19.29284385759799036, -8.630756214087126565, 51.74842643355248129 ) ) ;
#27057 = DIRECTION ( 'NONE',  ( 8.329294198805576557E-07, -2.487164606213012505E-06, 0.9999999999965599740 ) ) ;
#27058 = CARTESIAN_POINT ( 'NONE',  ( -13.04909385759799001, -8.112991634885936776, 51.74999426922421719 ) ) ;
#27059 = CARTESIAN_POINT ( 'NONE',  ( -24.83515292193595769, -14.04764123926324082, 73.23776205861604183 ) ) ;
#27060 = DIRECTION ( 'NONE',  ( -2.866981220435666553E-17, 1.000000000000000000, 1.190614954331866791E-16 ) ) ;
#27061 = DIRECTION ( 'NONE',  ( -3.071710424422018668E-17, 6.404604876783312462E-16, 1.000000000000000000 ) ) ;
#27062 = VERTEX_POINT ( 'NONE', #24504 ) ;
#27063 = ORIENTED_EDGE ( 'NONE', *, *, #10574, .T. ) ;
#27064 = B_SPLINE_CURVE_WITH_KNOTS ( 'NONE', 1,
 ( #46510, #2404 ),
 .UNSPECIFIED., .F., .F.,
 ( 2, 2 ),
 ( 0.000000000000000000, 1.000000000000000000 ),
 .UNSPECIFIED. ) ;
#27065 = CARTESIAN_POINT ( 'NONE',  ( -11.50733966670835784, -18.64282282746206576, 64.75266899466718939 ) ) ;
#27066 = ADVANCED_FACE ( 'NONE', ( #6008 ), #5048, .T. ) ;
#27067 = CARTESIAN_POINT ( 'NONE',  ( -18.63018970549565978, -7.457396494496333794, 73.95569010969242640 ) ) ;
#27068 = CARTESIAN_POINT ( 'NONE',  ( -20.72450927900464634, -21.03929139025763106, 58.93003081252663833 ) ) ;
#27069 = ADVANCED_FACE ( 'NONE', ( #10201 ), #9951, .T. ) ;
#27070 = ORIENTED_EDGE ( 'NONE', *, *, #8617, .T. ) ;
#27071 = EDGE_CURVE ( 'NONE', #3400, #27869, #29742, .T. ) ;
#27072 = ORIENTED_EDGE ( 'NONE', *, *, #44407, .T. ) ;
#27073 = DIRECTION ( 'NONE',  ( 0.9687793358424819923, -0.2479245821708680464, 0.000000000000000000 ) ) ;
#27074 = CARTESIAN_POINT ( 'NONE',  ( -24.86251202286899442, -14.39255128295101471, 66.22646819999783929 ) ) ;
#27075 = DIRECTION ( 'NONE',  ( 0.000000000000000000, 0.000000000000000000, 1.000000000000000000 ) ) ;
#27076 = CARTESIAN_POINT ( 'NONE',  ( -11.53247254227971652, -18.68106628708273931, 65.04707076447483871 ) ) ;
#27077 = EDGE_CURVE ( 'NONE', #12698, #45155, #47858, .T. ) ;
#27078 = ORIENTED_EDGE ( 'NONE', *, *, #21393, .F. ) ;
#27079 = CARTESIAN_POINT ( 'NONE',  ( -10.53709241384829909, -16.06257281177559904, 67.97767780858876563 ) ) ;
#27080 = CIRCLE ( 'NONE', #38076, 2.500000000000000444 ) ;
#27081 = DIRECTION ( 'NONE',  ( 0.000000000000000000, 1.000000000000000000, 0.000000000000000000 ) ) ;
#27082 = PRODUCT_RELATED_PRODUCT_CATEGORY ( 'part', '', ( #38600 ) ) ;
#27083 = VECTOR ( 'NONE', #40846, 1000.000000000000000 ) ;
#27084 = VERTEX_POINT ( 'NONE', #14814 ) ;
#27085 = CARTESIAN_POINT ( 'NONE',  ( -22.63008487438422733, -10.12971324841507581, 70.31178520543817001 ) ) ;
#27086 = CYLINDRICAL_SURFACE ( 'NONE', #30485, 5.249999999999998224 ) ;
#27087 = ORIENTED_EDGE ( 'NONE', *, *, #25351, .T. ) ;
#27088 = CARTESIAN_POINT ( 'NONE',  ( -17.54761332253163886, -7.808689223265699475, 67.20966559432535803 ) ) ;
#27089 = EDGE_LOOP ( 'NONE', ( #29384, #7733, #33639 ) ) ;
#27090 = CARTESIAN_POINT ( 'NONE',  ( -17.04284385759799036, -7.587656875400192291, 49.25157356644813689 ) ) ;
#27091 = CARTESIAN_POINT ( 'NONE',  ( -42.67115267894246955, -14.80920654474410547, 61.02352941176469869 ) ) ;
#27092 = VERTEX_POINT ( 'NONE', #3516 ) ;
#27093 = CARTESIAN_POINT ( 'NONE',  ( -17.42409385541299471, -14.80920654474435771, 49.52966884056655772 ) ) ;
#27094 = DIRECTION ( 'NONE',  ( -3.413470714839332458E-33, 1.190614954331866791E-16, -1.000000000000000000 ) ) ;
#27095 = CARTESIAN_POINT ( 'NONE',  ( -16.42409385650551812, -6.426201560718813433, 50.50509628382439331 ) ) ;
#27096 = CARTESIAN_POINT ( 'NONE',  ( -10.83008762082782006, -12.29245259246931354, 60.94286399630310314 ) ) ;
#27097 = EDGE_CURVE ( 'NONE', #17527, #33284, #33290, .T. ) ;
#27098 = CARTESIAN_POINT ( 'NONE',  ( -19.43707224927095822, -8.044379180677138308, 63.57522333692026706 ) ) ;
#27099 = CARTESIAN_POINT ( 'NONE',  ( -14.80056043599933524, -21.78207186541723317, 61.82095768364339960 ) ) ;
#27100 = ORIENTED_EDGE ( 'NONE', *, *, #9712, .T. ) ;
#27101 = FACE_OUTER_BOUND ( 'NONE', #8303, .T. ) ;
#27102 = CYLINDRICAL_SURFACE ( 'NONE', #6128, 0.5000000000000004441 ) ;
#27103 = CARTESIAN_POINT ( 'NONE',  ( -18.45621107931398797, -21.73269801629363940, 69.00617840904642719 ) ) ;
#27104 = CARTESIAN_POINT ( 'NONE',  ( -20.69990079259183702, -20.99685563420014489, 62.18641693201382736 ) ) ;
#27105 = VERTEX_POINT ( 'NONE', #18529 ) ;
#27106 = ORIENTED_EDGE ( 'NONE', *, *, #15368, .F. ) ;
#27107 = PLANE ( 'NONE',  #32225 ) ;
#27108 = CARTESIAN_POINT ( 'NONE',  ( -22.88264614489240856, -10.34704276773305764, 63.35713876973677827 ) ) ;
#27109 = ORIENTED_EDGE ( 'NONE', *, *, #14011, .F. ) ;
#27110 = CARTESIAN_POINT ( 'NONE',  ( -10.39693166811831304, -15.37990016280386918, 57.58264896457095006 ) ) ;
#27111 = CARTESIAN_POINT ( 'NONE',  ( -15.76121213363234119, -7.547108953211918880, 67.24668947344561332 ) ) ;
#27112 = CARTESIAN_POINT ( 'NONE',  ( -22.55534385759799321, -8.623186033802570094, 49.24843789510466507 ) ) ;
#27113 = DIRECTION ( 'NONE',  ( 2.430360955834641685E-06, 9.751098515052924655E-07, -0.9999999999965711872 ) ) ;
#27114 = CARTESIAN_POINT ( 'NONE',  ( -17.98657259272421172, -21.83703102787368167, 62.16063850355641307 ) ) ;
#27115 = CARTESIAN_POINT ( 'NONE',  ( -15.77324524160535191, -8.006205000634873059, 70.62606529040051839 ) ) ;
#27116 = CARTESIAN_POINT ( 'NONE',  ( -24.72409385541305582, -14.80920654474410547, 56.99999999999998579 ) ) ;
#27117 = AXIS2_PLACEMENT_3D ( 'NONE', #39356, #16196, #42330 ) ;
#27118 = ORIENTED_EDGE ( 'NONE', *, *, #35841, .T. ) ;
#27119 = CARTESIAN_POINT ( 'NONE',  ( -10.02450680348118617, -15.67453976365170831, 61.13814800358835555 ) ) ;
#27120 = AXIS2_PLACEMENT_3D ( 'NONE', #8900, #42868, #23920 ) ;
#27121 = CARTESIAN_POINT ( 'NONE',  ( -35.32409385541306079, -2.423472813913224222, 48.79999999999998295 ) ) ;
#27122 = EDGE_CURVE ( 'NONE', #21395, #24418, #2964, .T. ) ;
#27123 = DIRECTION ( 'NONE',  ( 0.2479245821708712938, 0.9687793358424811041, 0.000000000000000000 ) ) ;
#27124 = CARTESIAN_POINT ( 'NONE',  ( -24.72409385541305582, -14.80920654474423159, 69.97058823529410176 ) ) ;
#27125 = CARTESIAN_POINT ( 'NONE',  ( -21.39967327233876304, -20.63170314183283693, 72.80974286114339122 ) ) ;
#27126 = EDGE_CURVE ( 'NONE', #21655, #10899, #38200, .T. ) ;
#27127 = B_SPLINE_CURVE_WITH_KNOTS ( 'NONE', 3,
 ( #3486, #18499, #48544, #23193, #19246, #8179, #4237, #30349, #781, #38684 ),
 .UNSPECIFIED., .F., .F.,
 ( 4, 2, 2, 2, 4 ),
 ( 0.000000000000000000, 0.2500000000000000000, 0.5000000000000000000, 0.7500000000000000000, 1.000000000000000000 ),
 .UNSPECIFIED. ) ;
#27128 =( BOUNDED_SURFACE ( )  B_SPLINE_SURFACE ( 3, 1, ( 
 ( #34510, #46091 ),
 ( #20897, #30603 ),
 ( #45628, #11879 ),
 ( #34760, #23210 ),
 ( #15791, #12353 ),
 ( #16267, #794 ),
 ( #1034, #37963 ) ),
 .UNSPECIFIED., .T., .F., .F. ) 
 B_SPLINE_SURFACE_WITH_KNOTS ( ( 4, 3, 4 ),
 ( 2, 2 ),
 ( 0.000000000000000000, 0.5000000000000000000, 1.000000000000000000 ),
 ( 0.000000000000000000, 1.000000000000000000 ),
 .UNSPECIFIED. ) 
 GEOMETRIC_REPRESENTATION_ITEM ( )  RATIONAL_B_SPLINE_SURFACE ( (
 ( 1.000000000000000000, 1.000000000000000000),
 ( 0.3333333333333335369, 0.3333333333333330373),
 ( 0.3333333333333335369, 0.3333333333333330373),
 ( 1.000000000000000000, 1.000000000000000000),
 ( 0.3333333333333333703, 0.3333333333333333703),
 ( 0.3333333333333333703, 0.3333333333333333703),
 ( 1.000000000000000000, 1.000000000000000000) ) ) 
 REPRESENTATION_ITEM ( '' )  SURFACE ( )  );
#27129 = CARTESIAN_POINT ( 'NONE',  ( -10.70566866894272984, -16.94585410378973123, 57.98760548748135335 ) ) ;
#27130 = VERTEX_POINT ( 'NONE', #25937 ) ;
#27131 = ORIENTED_EDGE ( 'NONE', *, *, #42518, .T. ) ;
#27132 = ADVANCED_FACE ( 'NONE', ( #17797 ), #2564, .T. ) ;
#27133 = ORIENTED_EDGE ( 'NONE', *, *, #31847, .F. ) ;
#27134 = CYLINDRICAL_SURFACE ( 'NONE', #5994, 4.686499999999997002 ) ;
#27135 = CARTESIAN_POINT ( 'NONE',  ( -10.04792990808071984, -13.75760301026566523, 57.63480408467697913 ) ) ;
#27136 = ADVANCED_FACE ( 'NONE', ( #25452 ), #43946, .T. ) ;
#27138 =( BOUNDED_SURFACE ( )  B_SPLINE_SURFACE ( 3, 1, ( 
 ( #35021, #8943 ),
 ( #19044, #8218 ),
 ( #12142, #41700 ),
 ( #7986, #27164 ),
 ( #34535, #34048 ),
 ( #15569, #15325 ),
 ( #37989, #19783 ) ),
 .UNSPECIFIED., .T., .F., .F. ) 
 B_SPLINE_SURFACE_WITH_KNOTS ( ( 4, 3, 4 ),
 ( 2, 2 ),
 ( 0.000000000000000000, 0.5000000000000000000, 1.000000000000000000 ),
 ( 0.000000000000000000, 1.000000000000000000 ),
 .UNSPECIFIED. ) 
 GEOMETRIC_REPRESENTATION_ITEM ( )  RATIONAL_B_SPLINE_SURFACE ( (
 ( 1.000000000000000000, 1.000000000000000000),
 ( 0.3333333333333335369, 0.3333333333333330373),
 ( 0.3333333333333335369, 0.3333333333333330373),
 ( 1.000000000000000000, 1.000000000000000000),
 ( 0.3333333333333333703, 0.3333333333333333703),
 ( 0.3333333333333333703, 0.3333333333333333703),
 ( 1.000000000000000000, 1.000000000000000000) ) ) 
 REPRESENTATION_ITEM ( '' )  SURFACE ( )  );
#27137 = B_SPLINE_CURVE_WITH_KNOTS ( 'NONE', 3,
 ( #34244, #30586, #1243, #530, #45843, #27111, #16249, #38179, #42140, #8405 ),
 .UNSPECIFIED., .F., .F.,
 ( 4, 2, 2, 2, 4 ),
 ( 0.6272669072877962160, 0.7522669073073026125, 0.8772669073268088979, 1.002266907346315294, 1.127266907365821691 ),
 .UNSPECIFIED. ) ;
#27139 = ORIENTED_EDGE ( 'NONE', *, *, #36502, .T. ) ;
#27140 =( BOUNDED_CURVE ( )  B_SPLINE_CURVE ( 3, ( #1868, #33034, #10891, #28468 ),
 .UNSPECIFIED., .F., .F. ) 
 B_SPLINE_CURVE_WITH_KNOTS ( ( 4, 4 ),
 ( 4.712388980384690562, 4.921828490624010399 ),
 .UNSPECIFIED. ) 
 CURVE ( )  GEOMETRIC_REPRESENTATION_ITEM ( )  RATIONAL_B_SPLINE_CURVE ( ( 1.000000000000000000, 0.9963479302455154896, 0.9963479302455154896, 1.000000000000000000 ) ) 
 REPRESENTATION_ITEM ( '' )  );
#27141 = DIRECTION ( 'NONE',  ( -0.9757441136919988711, -0.2189141945955433433, 0.000000000000000000 ) ) ;
#27142 = CARTESIAN_POINT ( 'NONE',  ( -10.95381480682210373, -17.48044017699314523, 68.09721944380058289 ) ) ;
#27143 = LINE ( 'NONE', #15549, #16732 ) ;
#27144 = ORIENTED_EDGE ( 'NONE', *, *, #1008, .F. ) ;
#27145 = CYLINDRICAL_SURFACE ( 'NONE', #13448, 4.686499999999997002 ) ;
#27146 = CARTESIAN_POINT ( 'NONE',  ( -19.30706997687812887, -22.01740875295033462, 58.64012098774584558 ) ) ;
#27147 = VERTEX_POINT ( 'NONE', #6506 ) ;
#27148 = LINE ( 'NONE', #8205, #39101 ) ;
#27149 = EDGE_CURVE ( 'NONE', #11955, #31941, #34767, .T. ) ;
#27150 = CARTESIAN_POINT ( 'NONE',  ( -23.95744578735505925, -17.32345456025280939, 69.69723189175576294 ) ) ;
#27151 =( BOUNDED_CURVE ( )  B_SPLINE_CURVE ( 3, ( #14494, #40873, #44115, #10369 ),
 .UNSPECIFIED., .F., .F. ) 
 B_SPLINE_CURVE_WITH_KNOTS ( ( 4, 4 ),
 ( 0.9074455897393589598, 1.000000000000000000 ),
 .UNSPECIFIED. ) 
 CURVE ( )  GEOMETRIC_REPRESENTATION_ITEM ( )  RATIONAL_B_SPLINE_CURVE ( ( 0.6983129098260724144, 0.7760317562606804387, 0.8765941196519896339, 1.000000000000000000 ) ) 
 REPRESENTATION_ITEM ( '' )  );
#27152 = EDGE_CURVE ( 'NONE', #22777, #18177, #48571, .T. ) ;
#27153 = VECTOR ( 'NONE', #38069, 1000.000000000000114 ) ;
#27154 = VERTEX_POINT ( 'NONE', #18040 ) ;
#27155 = CARTESIAN_POINT ( 'NONE',  ( -11.14487098867647674, -10.79975683114651375, 57.38716000137919337 ) ) ;
#27156 = CARTESIAN_POINT ( 'NONE',  ( -22.48430581236326731, -20.27711595259535571, 65.81926302645771898 ) ) ;
#27157 = CARTESIAN_POINT ( 'NONE',  ( -18.13659385541303948, -8.995762431863221664, 51.38120296130585984 ) ) ;
#27158 = ORIENTED_EDGE ( 'NONE', *, *, #34698, .F. ) ;
#27159 = CARTESIAN_POINT ( 'NONE',  ( -11.17855889551124982, -18.87086522978130532, 64.86211687253867808 ) ) ;
#27160 = VECTOR ( 'NONE', #47097, 1000.000000000000000 ) ;
#27161 = DIRECTION ( 'NONE',  ( 0.9687793358424821033, -0.2479245821708677133, 0.000000000000000000 ) ) ;
#27162 = B_SPLINE_CURVE_WITH_KNOTS ( 'NONE', 3,
 ( #19491, #34506, #542, #1505, #11874, #8189, #4976, #24168, #12109, #1029 ),
 .UNSPECIFIED., .F., .F.,
 ( 4, 2, 2, 2, 4 ),
 ( 0.000000000000000000, 0.2500000000000000000, 0.5000000000000000000, 0.7500000000000000000, 1.000000000000000000 ),
 .UNSPECIFIED. ) ;
#27163 = CARTESIAN_POINT ( 'NONE',  ( -10.83683317046381234, -12.44108562964681219, 57.62857332099802932 ) ) ;
#27164 = CARTESIAN_POINT ( 'NONE',  ( -24.49635618495769407, -12.46679672499890046, 73.35730262454691797 ) ) ;
#27165 = CARTESIAN_POINT ( 'NONE',  ( -15.49416032233947504, -8.028509233753512220, 74.07985659018983426 ) ) ;
#27166 = CARTESIAN_POINT ( 'NONE',  ( -13.52147574634739158, -20.68483581939294780, 65.07809159860286741 ) ) ;
#27167 = CARTESIAN_POINT ( 'NONE',  ( -20.75354924259569245, -21.52967727414722532, 54.27966884056655061 ) ) ;
#27168 = CARTESIAN_POINT ( 'NONE',  ( -20.94768682599708853, -20.85770162187707299, 62.30574560354166636 ) ) ;
#27169 = CARTESIAN_POINT ( 'NONE',  ( -10.49862800246030936, -15.82799116930659622, 64.50771590054291948 ) ) ;
#27170 = CARTESIAN_POINT ( 'NONE',  ( -15.43659385650551741, -6.915538690918075382, 49.31353937987644542 ) ) ;
#27171 = ORIENTED_EDGE ( 'NONE', *, *, #48076, .T. ) ;
#27172 = CARTESIAN_POINT ( 'NONE',  ( -17.91840021365262814, -21.79173196354552644, 62.17535923606572368 ) ) ;
#27173 = CARTESIAN_POINT ( 'NONE',  ( -10.47674162631993866, -17.49967561431467544, 64.74926642219794815 ) ) ;
#27174 = EDGE_LOOP ( 'NONE', ( #30187, #27255, #16503, #39964 ) ) ;
#27175 = CARTESIAN_POINT ( 'NONE',  ( -9.974456290884534226, -14.72748455880875795, 71.51278017970571454 ) ) ;
#27176 = CARTESIAN_POINT ( 'NONE',  ( -10.59994951589548151, -17.79852801025984732, 71.72864675479873142 ) ) ;
#27177 = CARTESIAN_POINT ( 'NONE',  ( -23.25757785049868787, -10.17517560731475967, 63.18690593950643120 ) ) ;
#27178 = DIRECTION ( 'NONE',  ( 8.563106566420985232E-06, -6.519503004583679708E-06, 0.9999999999420846608 ) ) ;
#27179 = ORIENTED_EDGE ( 'NONE', *, *, #40353, .F. ) ;
#27180 = CARTESIAN_POINT ( 'NONE',  ( -18.33016535318852291, -22.20398178282153623, 69.07160637178317586 ) ) ;
#27181 = CARTESIAN_POINT ( 'NONE',  ( -21.18000425931230168, -20.77541442555289919, 69.20450184740300870 ) ) ;
#27182 = B_SPLINE_CURVE_WITH_KNOTS ( 'NONE', 3,
 ( #15732, #26594, #23152, #4421, #25857, #11332, #40872, #19441, #22409, #7651 ),
 .UNSPECIFIED., .F., .F.,
 ( 4, 2, 2, 2, 4 ),
 ( 0.6272669072976577720, 0.7522669073146923679, 0.8772669073317270749, 1.002266907348761782, 1.127266907365796378 ),
 .UNSPECIFIED. ) ;
#27183 = CARTESIAN_POINT ( 'NONE',  ( -19.09948850906665285, -8.012659424734943414, 63.73089235424028942 ) ) ;
#27184 = EDGE_LOOP ( 'NONE', ( #10998, #4589, #30946, #30604 ) ) ;
#27185 = CARTESIAN_POINT ( 'NONE',  ( -17.29268214306257434, -7.359616301281327821, 70.67691090883880634 ) ) ;
#27186 = CARTESIAN_POINT ( 'NONE',  ( -26.42409385541305511, -8.109206544744111511, 50.50000000000000000 ) ) ;
#27187 = CARTESIAN_POINT ( 'NONE',  ( -48.42409385541304800, -27.10920654474410796, 79.99999999999998579 ) ) ;
#27188 = CARTESIAN_POINT ( 'NONE',  ( -17.79084088774825645, -7.768752266068900347, 60.08060768310445354 ) ) ;
#27189 = EDGE_LOOP ( 'NONE', ( #12210, #27072, #27131, #28949, #18312 ) ) ;
#27190 = VERTEX_POINT ( 'NONE', #25684 ) ;
#27191 = TOROIDAL_SURFACE ( 'NONE', #47614, 1.350000000000000311, 0.1000000000000000056 ) ;
#27192 = CARTESIAN_POINT ( 'NONE',  ( -21.39909385541304232, -8.105421454601382081, 49.25000573077640098 ) ) ;
#27193 = EDGE_CURVE ( 'NONE', #29528, #38066, #40701, .T. ) ;
#27194 = CARTESIAN_POINT ( 'NONE',  ( -10.73296288398890930, -12.58843297884804002, 60.79853574628657498 ) ) ;
#27195 = EDGE_CURVE ( 'NONE', #31755, #12655, #3285, .T. ) ;
#27196 = CARTESIAN_POINT ( 'NONE',  ( -20.50074447585702941, -8.457105438040551704, 70.39533052524389234 ) ) ;
#27197 = CARTESIAN_POINT ( 'NONE',  ( -13.83108299072750391, -21.33561835983412891, 72.04112301026525245 ) ) ;
#27198 = CARTESIAN_POINT ( 'NONE',  ( -17.70776945889202736, -22.25388964270624825, 58.52058054029878065 ) ) ;
#27199 = CARTESIAN_POINT ( 'NONE',  ( -10.38360249164154325, -14.43747963625415309, 67.87272197508832505 ) ) ;
#27200 = CARTESIAN_POINT ( 'NONE',  ( -10.38974003836240634, -14.29666208179129150, 68.27288787427933414 ) ) ;
#27201 = CARTESIAN_POINT ( 'NONE',  ( -24.32132670238839012, -16.30692182044891325, 66.20758098450045281 ) ) ;
#27202 = VERTEX_POINT ( 'NONE', #19515 ) ;
#27203 = CARTESIAN_POINT ( 'NONE',  ( -24.41485940220508510, -14.44976662329334616, 66.18292729254385165 ) ) ;
#27204 = ADVANCED_FACE ( 'NONE', ( #38464 ), #26422, .T. ) ;
#27205 = CARTESIAN_POINT ( 'NONE',  ( -10.46944733747312917, -15.96661384539355133, 67.99239968927004441 ) ) ;
#27206 = EDGE_CURVE ( 'NONE', #19106, #14369, #39792, .T. ) ;
#27207 = EDGE_LOOP ( 'NONE', ( #6037, #5667, #32207, #33970 ) ) ;
#27208 = CARTESIAN_POINT ( 'NONE',  ( -27.42409385541305511, -6.359206544744109735, 63.99999999999998579 ) ) ;
#27209 = CARTESIAN_POINT ( 'NONE',  ( -21.84079810191280657, -9.314188493807272096, 63.49153755726581494 ) ) ;
#27210 = ADVANCED_FACE ( 'NONE', ( #30620 ), #19272, .T. ) ;
#27212 = EDGE_CURVE ( 'NONE', #44794, #13527, #13037, .T. ) ;
#27211 = ORIENTED_EDGE ( 'NONE', *, *, #26798, .T. ) ;
#27213 = CARTESIAN_POINT ( 'NONE',  ( -18.11578073608761841, -22.22715074075463804, 65.52344916871619773 ) ) ;
#27214 = ADVANCED_FACE ( 'NONE', ( #38211 ), #34038, .T. ) ;
#27215 = VERTEX_POINT ( 'NONE', #41431 ) ;
#27216 = CARTESIAN_POINT ( 'NONE',  ( -16.39888349198502127, -21.73372412438269308, 62.05568132716130236 ) ) ;
#27217 = CARTESIAN_POINT ( 'NONE',  ( 23.52590614458706852, 1.890747609047893185, 50.53028072113869484 ) ) ;
#27218 = DIRECTION ( 'NONE',  ( 1.000000000000000000, 2.866981220435666553E-17, 0.000000000000000000 ) ) ;
#27219 = EDGE_LOOP ( 'NONE', ( #2278, #11026, #12194, #34121 ) ) ;
#27220 = CARTESIAN_POINT ( 'NONE',  ( -22.06352460594304787, -8.980016202103444201, 63.37649054182217867 ) ) ;
#27221 = CARTESIAN_POINT ( 'NONE',  ( -20.89545688568268389, -21.40122061776584772, 58.80508532579719372 ) ) ;
#27222 = LINE ( 'NONE', #45461, #30167 ) ;
#27223 = CIRCLE ( 'NONE', #5992, 1.999999999999999556 ) ;
#27224 = VECTOR ( 'NONE', #36850, 1000.000000000000114 ) ;
#27225 = FACE_BOUND ( 'NONE', #43761, .T. ) ;
#27226 = CARTESIAN_POINT ( 'NONE',  ( -11.40696025980006389, -18.38620811258373422, 57.82216998879101055 ) ) ;
#27227 = CARTESIAN_POINT ( 'NONE',  ( -24.72409385541305582, -14.80920654474422271, 68.06470588235292496 ) ) ;
#27228 = CARTESIAN_POINT ( 'NONE',  ( -10.66703363856100317, -12.79807828486586807, 64.26836111018113229 ) ) ;
#27229 = ORIENTED_EDGE ( 'NONE', *, *, #18820, .F. ) ;
#27230 = CARTESIAN_POINT ( 'NONE',  ( -12.05483347687720475, -10.31798811457585963, 67.79896870046731294 ) ) ;
#27231 = VERTEX_POINT ( 'NONE', #11639 ) ;
#27232 = DIRECTION ( 'NONE',  ( 0.1539336739619741601, 0.9880811829098681276, 6.607022902453645889E-08 ) ) ;
#27233 = CARTESIAN_POINT ( 'NONE',  ( -16.78341213209640159, -22.23169296657789928, 68.88056055876903372 ) ) ;
#27234 = B_SPLINE_CURVE_WITH_KNOTS ( 'NONE', 3,
 ( #47155, #9733, #17337, #14343, #37495, #21768, #48346, #44675, #18799, #22014 ),
 .UNSPECIFIED., .F., .F.,
 ( 4, 2, 2, 2, 4 ),
 ( 0.000000000000000000, 0.2500000000000000000, 0.5000000000000000000, 0.7500000000000000000, 1.000000000000000000 ),
 .UNSPECIFIED. ) ;
#27235 = VERTEX_POINT ( 'NONE', #7975 ) ;
#27236 = CARTESIAN_POINT ( 'NONE',  ( -15.03263910315855512, -8.176888424288378587, 56.86472059657746314 ) ) ;
#27237 = CARTESIAN_POINT ( 'NONE',  ( -12.73406765192711987, -9.020692726705027198, 71.04263666671683097 ) ) ;
#27238 = ORIENTED_EDGE ( 'NONE', *, *, #9089, .F. ) ;
#27239 = EDGE_CURVE ( 'NONE', #27904, #25059, #11694, .T. ) ;
#27240 = VERTEX_POINT ( 'NONE', #45643 ) ;
#27241 = ORIENTED_EDGE ( 'NONE', *, *, #42193, .F. ) ;
#27242 = DIRECTION ( 'NONE',  ( -0.9660698163281072892, -0.2582810677919976650, 5.363434502754641456E-08 ) ) ;
#27243 = PRESENTATION_STYLE_ASSIGNMENT (( #38558 ) ) ;
#27244 = CARTESIAN_POINT ( 'NONE',  ( -16.57554779340669882, -22.21081089906203943, 65.41059674993448425 ) ) ;
#27245 = CARTESIAN_POINT ( 'NONE',  ( -21.22399696191457252, -8.930295582149165412, 73.82801983812771596 ) ) ;
#27246 = DIRECTION ( 'NONE',  ( 0.000000000000000000, 1.000000000000000000, -0.000000000000000000 ) ) ;
#27247 = CARTESIAN_POINT ( 'NONE',  ( -10.43125871347677958, -13.91323993190135155, 57.59825034919892772 ) ) ;
#27248 = VERTEX_POINT ( 'NONE', #37732 ) ;
#27249 = ORIENTED_EDGE ( 'NONE', *, *, #35579, .T. ) ;
#27250 = CARTESIAN_POINT ( 'NONE',  ( -22.44284385650551528, -8.811426318492348031, 52.18089403414751359 ) ) ;
#27251 = EDGE_CURVE ( 'NONE', #46448, #32393, #40463, .T. ) ;
#27252 = CARTESIAN_POINT ( 'NONE',  ( -10.41614636368765900, -13.97037319380632248, 64.53236772669211518 ) ) ;
#27253 = CARTESIAN_POINT ( 'NONE',  ( -21.01047406150117070, -21.33922706731038232, 62.22197251680120189 ) ) ;
#27254 = CARTESIAN_POINT ( 'NONE',  ( -21.53009576834440608, -9.139789435051676847, 70.13132584627037147 ) ) ;
#27255 = ORIENTED_EDGE ( 'NONE', *, *, #34201, .T. ) ;
#27256 = CARTESIAN_POINT ( 'NONE',  ( -22.72409385650551528, -6.426201560718813433, 50.50509628382439331 ) ) ;
#27257 = AXIS2_PLACEMENT_3D ( 'NONE', #24059, #2123, #13180 ) ;
#27258 = VERTEX_POINT ( 'NONE', #15556 ) ;
#27259 = CARTESIAN_POINT ( 'NONE',  ( -14.73525069530193399, -21.75714069359356984, 61.89246344873641448 ) ) ;
#27260 = CARTESIAN_POINT ( 'NONE',  ( -10.37462438995674319, -14.89569194323783030, 74.79778901495059529 ) ) ;
#27261 = DIRECTION ( 'NONE',  ( 0.000000000000000000, 1.000000000000000000, -0.000000000000000000 ) ) ;
#27262 = CIRCLE ( 'NONE', #39061, 2.000000000000001332 ) ;
#27263 = EDGE_LOOP ( 'NONE', ( #43927, #36282, #30512, #31441, #33344 ) ) ;
#27264 = CARTESIAN_POINT ( 'NONE',  ( -17.42409385541299471, -14.80920654474435771, 49.52966884056655772 ) ) ;
#27265 = DIRECTION ( 'NONE',  ( 0.9562635972186038780, -0.2925062950340272527, 4.666065131241567634E-08 ) ) ;
#27266 = EDGE_CURVE ( 'NONE', #30119, #30489, #44848, .T. ) ;
#27267 = ADVANCED_FACE ( 'NONE', ( #37479 ), #28305, .T. ) ;
#27268 = CARTESIAN_POINT ( 'NONE',  ( -12.98444386793654459, -9.332658658743872238, 70.84925372438172531 ) ) ;
#27269 = ORIENTED_EDGE ( 'NONE', *, *, #39329, .F. ) ;
#27270 = CARTESIAN_POINT ( 'NONE',  ( -10.44050833889757079, -15.30664536039409107, 57.63963066593323248 ) ) ;
#27271 =( BOUNDED_CURVE ( )  B_SPLINE_CURVE ( 3, ( #25655, #7699, #37706, #3999 ),
 .UNSPECIFIED., .F., .F. ) 
 B_SPLINE_CURVE_WITH_KNOTS ( ( 4, 4 ),
 ( 4.712388980384689674, 4.921828490624009511 ),
 .UNSPECIFIED. ) 
 CURVE ( )  GEOMETRIC_REPRESENTATION_ITEM ( )  RATIONAL_B_SPLINE_CURVE ( ( 1.000000000000000000, 0.9963479302455154896, 0.9963479302455154896, 1.000000000000000000 ) ) 
 REPRESENTATION_ITEM ( '' )  );
#27272 = CARTESIAN_POINT ( 'NONE',  ( -11.46876066122178095, -18.48806595306161071, 61.57710833523393035 ) ) ;
#27273 = VERTEX_POINT ( 'NONE', #33792 ) ;
#27274 = LINE ( 'NONE', #42786, #36952 ) ;
#27275 = ORIENTED_EDGE ( 'NONE', *, *, #32515, .T. ) ;
#27276 = CARTESIAN_POINT ( 'NONE',  ( -15.15660932275500095, -21.48492473237050859, 65.39124617759186719 ) ) ;
#27277 = EDGE_CURVE ( 'NONE', #14849, #6686, #43267, .T. ) ;
#27278 = EDGE_CURVE ( 'NONE', #41019, #918, #16285, .T. ) ;
#27279 = CARTESIAN_POINT ( 'NONE',  ( -46.47622156840087371, -14.20920654474410760, 70.13000000000000966 ) ) ;
#27280 = ORIENTED_EDGE ( 'NONE', *, *, #37204, .F. ) ;
#27281 = CARTESIAN_POINT ( 'NONE',  ( -22.22034002972690203, -20.51002343881169665, 58.95717044630308123 ) ) ;
#27282 = CARTESIAN_POINT ( 'NONE',  ( -24.47273122526617684, -14.66856428242425636, 62.71296483725149784 ) ) ;
#27283 = CARTESIAN_POINT ( 'NONE',  ( -22.22619444978876757, -20.50513558618911958, 58.94938304221643222 ) ) ;
#27284 = ORIENTED_EDGE ( 'NONE', *, *, #24754, .T. ) ;
#27285 = FACE_OUTER_BOUND ( 'NONE', #12020, .T. ) ;
#27286 = DIRECTION ( 'NONE',  ( 0.000000000000000000, 0.000000000000000000, -1.000000000000000000 ) ) ;
#27287 = PLANE ( 'NONE',  #46402 ) ;
#27288 = CARTESIAN_POINT ( 'NONE',  ( -11.17692863878522225, -11.53409247417484274, 71.18040941340760241 ) ) ;
#27289 = ORIENTED_EDGE ( 'NONE', *, *, #3753, .T. ) ;
#27290 = CARTESIAN_POINT ( 'NONE',  ( -15.75283698213507755, -7.548994588147243334, 67.32502552484606895 ) ) ;
#27291 =( BOUNDED_SURFACE ( )  B_SPLINE_SURFACE ( 3, 1, ( 
 ( #43085, #35925 ),
 ( #17208, #5427 ),
 ( #42369, #39396 ),
 ( #35679, #23663 ),
 ( #24632, #34959 ),
 ( #24139, #39634 ),
 ( #5678, #47020 ) ),
 .UNSPECIFIED., .T., .F., .F. ) 
 B_SPLINE_SURFACE_WITH_KNOTS ( ( 4, 3, 4 ),
 ( 2, 2 ),
 ( 0.000000000000000000, 0.5000000000000000000, 1.000000000000000000 ),
 ( 0.000000000000000000, 1.000000000000000000 ),
 .UNSPECIFIED. ) 
 GEOMETRIC_REPRESENTATION_ITEM ( )  RATIONAL_B_SPLINE_SURFACE ( (
 ( 1.000000000000000000, 1.000000000000000000),
 ( 0.3333333333333335369, 0.3333333333333330373),
 ( 0.3333333333333335369, 0.3333333333333330373),
 ( 1.000000000000000000, 1.000000000000000000),
 ( 0.3333333333333333703, 0.3333333333333333703),
 ( 0.3333333333333333703, 0.3333333333333333703),
 ( 1.000000000000000000, 1.000000000000000000) ) ) 
 REPRESENTATION_ITEM ( '' )  SURFACE ( )  );
#27292 = AXIS2_PLACEMENT_3D ( 'NONE', #9947, #17318, #32367 ) ;
#27293 = CARTESIAN_POINT ( 'NONE',  ( -11.46028008028683942, -18.56947564720590194, 61.56238700194530367 ) ) ;
#27294 = EDGE_CURVE ( 'NONE', #13075, #7864, #6152, .T. ) ;
#27295 = ORIENTED_EDGE ( 'NONE', *, *, #37134, .F. ) ;
#27296 = EDGE_LOOP ( 'NONE', ( #6169, #19877 ) ) ;
#27297 = CARTESIAN_POINT ( 'NONE',  ( -10.48245837418595805, -15.71172178951755427, 61.05291461354959637 ) ) ;
#27298 = CARTESIAN_POINT ( 'NONE',  ( -50.42609385541305755, -14.90920654474421170, 67.95882352941174531 ) ) ;
#27299 = CARTESIAN_POINT ( 'NONE',  ( 6.575906144586949331, -8.109206544743660316, 50.50000000000031264 ) ) ;
#27300 = VECTOR ( 'NONE', #35793, 1000.000000000000114 ) ;
#27301 = CARTESIAN_POINT ( 'NONE',  ( -20.33034385650551812, -9.794322478646142471, 51.19202720610083901 ) ) ;
#27302 = CARTESIAN_POINT ( 'NONE',  ( -12.41955227442780263, -9.914691306276559146, 57.08935537464338239 ) ) ;
#27303 = DIRECTION ( 'NONE',  ( -3.071710424422018668E-17, 6.404604876783312462E-16, 1.000000000000000000 ) ) ;
#27304 = CARTESIAN_POINT ( 'NONE',  ( -19.78779399205855327, -21.87446732333777888, 65.60339696459925563 ) ) ;
#27305 = CARTESIAN_POINT ( 'NONE',  ( -12.89447938415233175, -16.05746464591689104, 49.52966884056655772 ) ) ;
#27306 = VERTEX_POINT ( 'NONE', #2010 ) ;
#27307 = ORIENTED_EDGE ( 'NONE', *, *, #43829, .T. ) ;
#27308 = LINE ( 'NONE', #39110, #4540 ) ;
#27309 = CARTESIAN_POINT ( 'NONE',  ( -13.59294679993987565, -20.73687756253419678, 68.60058253670568718 ) ) ;
#27310 = FACE_OUTER_BOUND ( 'NONE', #34628, .T. ) ;
#27311 = B_SPLINE_CURVE_WITH_KNOTS ( 'NONE', 3,
 ( #179, #3605, #18607, #48662, #22828, #34122, #15393, #27952, #8285, #34855 ),
 .UNSPECIFIED., .F., .F.,
 ( 4, 2, 2, 2, 4 ),
 ( 0.000000000000000000, 0.2500000000000000000, 0.5000000000000000000, 0.7500000000000000000, 1.000000000000000000 ),
 .UNSPECIFIED. ) ;
#27312 = ORIENTED_EDGE ( 'NONE', *, *, #17868, .T. ) ;
#27313 = ORIENTED_EDGE ( 'NONE', *, *, #9889, .T. ) ;
#27314 = DIRECTION ( 'NONE',  ( -1.000000000000000000, -2.866981220435666553E-17, -0.000000000000000000 ) ) ;
#27315 = CARTESIAN_POINT ( 'NONE',  ( -23.42915847708036381, -11.11517115755410146, 73.64721174900437006 ) ) ;
#27316 = CARTESIAN_POINT ( 'NONE',  ( -14.97414238684038068, -21.84485642299321029, 65.30585465654563393 ) ) ;
#27317 = CARTESIAN_POINT ( 'NONE',  ( -24.48759320265496342, -17.17788619462897159, 72.92690118282537526 ) ) ;
#27318 = ORIENTED_EDGE ( 'NONE', *, *, #42818, .F. ) ;
#27319 = CARTESIAN_POINT ( 'NONE',  ( -24.44689184067228638, -14.18710713894228093, 69.93803194250310185 ) ) ;
#27320 = VECTOR ( 'NONE', #37146, 1000.000000000000000 ) ;
#27321 = VECTOR ( 'NONE', #7480, 1000.000000000000000 ) ;
#27322 = CARTESIAN_POINT ( 'NONE',  ( -19.25861376934618363, -8.001921477138727923, 60.25533195930442787 ) ) ;
#27323 = EDGE_CURVE ( 'NONE', #14849, #313, #6372, .T. ) ;
#27324 = ORIENTED_EDGE ( 'NONE', *, *, #13860, .F. ) ;
#27325 = AXIS2_PLACEMENT_3D ( 'NONE', #12028, #5127, #8337 ) ;
#27326 = CARTESIAN_POINT ( 'NONE',  ( -22.27817919856018136, -9.157513542003881568, 59.83675792137641736 ) ) ;
#27327 = CARTESIAN_POINT ( 'NONE',  ( -24.23444832799638604, -16.42945440209323849, 59.13949121896713024 ) ) ;
#27328 = ORIENTED_EDGE ( 'NONE', *, *, #22179, .T. ) ;
#27329 = CARTESIAN_POINT ( 'NONE',  ( -23.67513346179213940, -18.86224369876040896, 69.49383191692929529 ) ) ;
#27330 = EDGE_LOOP ( 'NONE', ( #15247, #6029, #21466, #24364, #1402 ) ) ;
#27331 = EDGE_CURVE ( 'NONE', #43020, #47460, #31426, .T. ) ;
#27332 = CARTESIAN_POINT ( 'NONE',  ( -16.93034385759798965, -6.857644439848010087, 49.98602051094140108 ) ) ;
#27333 = CARTESIAN_POINT ( 'NONE',  ( -11.63929734443426867, -10.76555703936739938, 57.35336384308645563 ) ) ;
#27334 = ORIENTED_EDGE ( 'NONE', *, *, #23442, .F. ) ;
#27335 = CARTESIAN_POINT ( 'NONE',  ( -23.85820194903862657, -17.69173191509663923, 62.48833042115953873 ) ) ;
#27336 = CARTESIAN_POINT ( 'NONE',  ( -15.99909385541290341, -8.105421454601380304, 49.25000573077616650 ) ) ;
#27337 = EDGE_CURVE ( 'NONE', #15639, #7607, #32289, .T. ) ;
#27338 = CARTESIAN_POINT ( 'NONE',  ( -19.06784385650551528, -6.428312510596451368, 51.20221977374900035 ) ) ;
#27339 = CYLINDRICAL_SURFACE ( 'NONE', #45685, 0.1500000000000007161 ) ;
#27340 = EDGE_CURVE ( 'NONE', #8650, #11545, #9893, .T. ) ;
#27341 = CARTESIAN_POINT ( 'NONE',  ( -10.49189908542464522, -16.09426454567519116, 68.26295692486267797 ) ) ;
#27342 = ORIENTED_EDGE ( 'NONE', *, *, #18032, .T. ) ;
#27343 = CARTESIAN_POINT ( 'NONE',  ( -10.44202790750644461, -14.30845231023897846, 64.38803863533676974 ) ) ;
#27344 = CARTESIAN_POINT ( 'NONE',  ( -11.51414000101334345, -10.27201461766008350, 74.62540520127058130 ) ) ;
#27345 = CARTESIAN_POINT ( 'NONE',  ( -23.12302755141047683, -18.95946607990388699, 62.50406880580509750 ) ) ;
#27346 = DIRECTION ( 'NONE',  ( -0.8398192074808118468, -0.5428661886195298436, -7.907900705248004564E-08 ) ) ;
#27347 = DIRECTION ( 'NONE',  ( 0.4408917724886829981, 0.07492959997082451751, 0.8944271909999156334 ) ) ;
#27348 = ORIENTED_EDGE ( 'NONE', *, *, #7033, .F. ) ;
#27349 = ORIENTED_EDGE ( 'NONE', *, *, #8722, .F. ) ;
#27350 = DIRECTION ( 'NONE',  ( -0.09077643883959130022, 0.9958712959773466933, 4.338678762321648003E-08 ) ) ;
#27351 = CARTESIAN_POINT ( 'NONE',  ( -14.60479746972646886, -7.913168098764732150, 60.50491608655884335 ) ) ;
#27352 = EDGE_LOOP ( 'NONE', ( #44455, #13670, #41420, #35873, #20379 ) ) ;
#27354 = CARTESIAN_POINT ( 'NONE',  ( -22.53538519471304369, -20.22938801946909138, 65.74775819791243237 ) ) ;
#27353 = AXIS2_PLACEMENT_3D ( 'NONE', #3967, #41632, #31038 ) ;
#27355 = CARTESIAN_POINT ( 'NONE',  ( -16.37525608968913460, -22.18513123027473455, 61.87755341768041717 ) ) ;
#27356 = CARTESIAN_POINT ( 'NONE',  ( -22.49909385759799108, -8.105421454601382081, 49.25000573077640098 ) ) ;
#27357 = CARTESIAN_POINT ( 'NONE',  ( -17.24064252496611971, -7.811500653502258196, 70.49035835121620153 ) ) ;
#27358 = LINE ( 'NONE', #7695, #20411 ) ;
#27359 = CARTESIAN_POINT ( 'NONE',  ( -12.28547924108692335, -10.05564394636707348, 60.85918091186046297 ) ) ;
#27360 = VECTOR ( 'NONE', #5899, 1000.000000000000000 ) ;
#27361 = CARTESIAN_POINT ( 'NONE',  ( -20.34748183946319244, -8.389919497863246534, 63.51941420704543617 ) ) ;
#27362 = AXIS2_PLACEMENT_3D ( 'NONE', #13442, #21583, #17388 ) ;
#27363 = ORIENTED_EDGE ( 'NONE', *, *, #21286, .T. ) ;
#27364 = DIRECTION ( 'NONE',  ( 2.342027643795563533E-48, 1.912410701131276611E-32, 1.000000000000000000 ) ) ;
#27365 = LINE ( 'NONE', #16983, #29004 ) ;
#27366 = CARTESIAN_POINT ( 'NONE',  ( -23.30132152709437676, -10.22970227413176580, 63.25841351925517841 ) ) ;
#27367 = AXIS2_PLACEMENT_3D ( 'NONE', #27345, #15763, #4955 ) ;
#27368 = CARTESIAN_POINT ( 'NONE',  ( -17.67039273561237778, -7.813102812166079936, 63.56673625629110091 ) ) ;
#27369 = CARTESIAN_POINT ( 'NONE',  ( -12.28060247932822691, -9.983304365141403736, 64.44402973226354447 ) ) ;
#27370 = VECTOR ( 'NONE', #38176, 1000.000000000000114 ) ;
#27371 = ORIENTED_EDGE ( 'NONE', *, *, #20054, .F. ) ;
#27372 = ORIENTED_EDGE ( 'NONE', *, *, #10032, .T. ) ;
#27373 = CARTESIAN_POINT ( 'NONE',  ( -22.97409385650551528, -9.792211528768504536, 50.49490371617623197 ) ) ;
#27374 = VERTEX_POINT ( 'NONE', #35728 ) ;
#27375 = FACE_OUTER_BOUND ( 'NONE', #18916, .T. ) ;
#27376 = CARTESIAN_POINT ( 'NONE',  ( -18.46801905451614445, -7.836623195388688679, 74.12592262855558545 ) ) ;
#27377 = EDGE_CURVE ( 'NONE', #16726, #21204, #1139, .T. ) ;
#27378 = ORIENTED_EDGE ( 'NONE', *, *, #34087, .T. ) ;
#27379 = CARTESIAN_POINT ( 'NONE',  ( -21.89826351590202336, -8.852228842849337198, 66.84645279485334868 ) ) ;
#27380 = CARTESIAN_POINT ( 'NONE',  ( -18.30607514908327715, -7.810853278037157565, 73.84064121929586122 ) ) ;
#27381 = ORIENTED_EDGE ( 'NONE', *, *, #44078, .T. ) ;
#27382 = CARTESIAN_POINT ( 'NONE',  ( -13.89248387370423110, -21.36903859207333412, 71.96961763246901000 ) ) ;
#27383 = AXIS2_PLACEMENT_3D ( 'NONE', #24983, #28676, #46903 ) ;
#27384 = CARTESIAN_POINT ( 'NONE',  ( -23.83833616213321704, -17.61232902345998141, 62.77360984984811410 ) ) ;
#27385 = VECTOR ( 'NONE', #4716, 1000.000000000000227 ) ;
#27386 = B_SPLINE_CURVE_WITH_KNOTS ( 'NONE', 1,
 ( #8941, #31821 ),
 .UNSPECIFIED., .F., .F.,
 ( 2, 2 ),
 ( 0.000000000000000000, 1.000000000000000000 ),
 .UNSPECIFIED. ) ;
#27387 = VERTEX_POINT ( 'NONE', #8931 ) ;
#27388 = CARTESIAN_POINT ( 'NONE',  ( -19.97164249076357478, -21.81019033462135326, 69.11977790463622284 ) ) ;
#27389 = CARTESIAN_POINT ( 'NONE',  ( -23.92719435707370224, -11.17417392741853988, 70.00715344888816105 ) ) ;
#27390 = AXIS2_PLACEMENT_3D ( 'NONE', #43766, #25046, #31942 ) ;
#27391 = ORIENTED_EDGE ( 'NONE', *, *, #21422, .T. ) ;
#27392 = CARTESIAN_POINT ( 'NONE',  ( -21.78913961794832588, -8.771810275399618106, 70.24637145832762997 ) ) ;
#27393 = ORIENTED_EDGE ( 'NONE', *, *, #22295, .F. ) ;
#27394 = CARTESIAN_POINT ( 'NONE',  ( -10.93120642218817729, -11.15588000066243168, 64.27165164367140449 ) ) ;
#27395 = EDGE_CURVE ( 'NONE', #25922, #16677, #10967, .T. ) ;
#27396 = FACE_OUTER_BOUND ( 'NONE', #9482, .T. ) ;
#27397 = VECTOR ( 'NONE', #26488, 1000.000000000000000 ) ;
#27398 = EDGE_CURVE ( 'NONE', #27387, #45387, #23950, .T. ) ;
#27399 = LINE ( 'NONE', #5006, #45519 ) ;
#27400 = CARTESIAN_POINT ( 'NONE',  ( -10.55151165865014384, -17.68520938540437371, 68.28217272534745064 ) ) ;
#27401 = CARTESIAN_POINT ( 'NONE',  ( -17.49284385759798965, -8.630756214087126565, 51.74842643355248129 ) ) ;
#27402 = CARTESIAN_POINT ( 'NONE',  ( -10.41794148240616735, -15.59560519520519151, 61.04348844167599708 ) ) ;
#27403 = CARTESIAN_POINT ( 'NONE',  ( -10.76763535483202539, -17.13171813241336494, 61.30743118825921556 ) ) ;
#27404 = DIRECTION ( 'NONE',  ( -3.071710424422018668E-17, 6.404604876783312462E-16, 1.000000000000000000 ) ) ;
#27405 = EDGE_CURVE ( 'NONE', #21373, #44738, #30463, .T. ) ;
#27406 = CARTESIAN_POINT ( 'NONE',  ( -22.42594789675818845, -19.77792426076253918, 69.45945937764655298 ) ) ;
#27407 = CARTESIAN_POINT ( 'NONE',  ( -17.12409385650551741, -6.426201560718813433, 50.50509628382439331 ) ) ;
#27408 = ORIENTED_EDGE ( 'NONE', *, *, #4177, .F. ) ;
#27409 = DIRECTION ( 'NONE',  ( -9.880513536971593873E-06, -1.241746728590076822E-06, 0.9999999999504166626 ) ) ;
#27410 = DIRECTION ( 'NONE',  ( -1.140458109893898545E-06, -1.256740822519431765E-06, 0.9999999999985598187 ) ) ;
#27411 = VERTEX_POINT ( 'NONE', #20497 ) ;
#27412 = CARTESIAN_POINT ( 'NONE',  ( -24.38078725910958866, -15.95265972659957576, 66.36324896149729113 ) ) ;
#27413 = CARTESIAN_POINT ( 'NONE',  ( -12.55198883488284878, -12.25722835735234639, 53.49999999999995026 ) ) ;
#27414 = CARTESIAN_POINT ( 'NONE',  ( -24.43362360091611052, -14.05489060867666673, 73.42271507725003232 ) ) ;
#27415 = CARTESIAN_POINT ( 'NONE',  ( -24.33677527904861648, -16.19409071606989414, 62.59328707532291247 ) ) ;
#27416 = ADVANCED_FACE ( 'NONE', ( #35497 ), #6444, .F. ) ;
#27417 =( BOUNDED_SURFACE ( )  B_SPLINE_SURFACE ( 3, 1, ( 
 ( #13921, #21591 ),
 ( #36570, #32661 ),
 ( #10271, #2383 ),
 ( #25287, #36819 ),
 ( #43762, #44254 ),
 ( #17864, #28495 ),
 ( #32888, #10016 ) ),
 .UNSPECIFIED., .T., .F., .F. ) 
 B_SPLINE_SURFACE_WITH_KNOTS ( ( 4, 3, 4 ),
 ( 2, 2 ),
 ( 0.000000000000000000, 0.5000000000000000000, 1.000000000000000000 ),
 ( 0.000000000000000000, 1.000000000000000000 ),
 .UNSPECIFIED. ) 
 GEOMETRIC_REPRESENTATION_ITEM ( )  RATIONAL_B_SPLINE_SURFACE ( (
 ( 1.000000000000000000, 1.000000000000000000),
 ( 0.3333333333333335369, 0.3333333333333330373),
 ( 0.3333333333333335369, 0.3333333333333330373),
 ( 1.000000000000000000, 1.000000000000000000),
 ( 0.3333333333333333703, 0.3333333333333333703),
 ( 0.3333333333333333703, 0.3333333333333333703),
 ( 1.000000000000000000, 1.000000000000000000) ) ) 
 REPRESENTATION_ITEM ( '' )  SURFACE ( )  );
#27418 = ORIENTED_EDGE ( 'NONE', *, *, #24669, .F. ) ;
#27419 = CARTESIAN_POINT ( 'NONE',  ( -24.80865520860317730, -15.79540089610985021, 69.65494700136302697 ) ) ;
#27420 = CARTESIAN_POINT ( 'NONE',  ( -10.05839037049808127, -15.92727522337501611, 64.55125644017783770 ) ) ;
#27421 = CARTESIAN_POINT ( 'NONE',  ( -10.08432996298220630, -16.08613878457147450, 68.07793591119110488 ) ) ;
#27422 = ORIENTED_EDGE ( 'NONE', *, *, #30013, .T. ) ;
#27423 = CARTESIAN_POINT ( 'NONE',  ( -17.79084047922378531, -7.768752242298102573, 60.23060768310389790 ) ) ;
#27424 = VECTOR ( 'NONE', #8944, 1000.000000000000000 ) ;
#27425 = CARTESIAN_POINT ( 'NONE',  ( -24.38903048123337314, -17.45395020021824450, 69.55306401233070801 ) ) ;
#27426 = VECTOR ( 'NONE', #28408, 1000.000000000000000 ) ;
#27427 = DIRECTION ( 'NONE',  ( 0.9687793358424821033, -0.2479245821708679909, 0.000000000000000000 ) ) ;
#27428 = CARTESIAN_POINT ( 'NONE',  ( -23.42409385541304090, -9.359200813967568422, 50.49621490985803263 ) ) ;
#27429 = CARTESIAN_POINT ( 'NONE',  ( -19.24025795797341942, -7.996846695050864540, 60.24620885950562865 ) ) ;
#27430 =( BOUNDED_CURVE ( )  B_SPLINE_CURVE ( 3, ( #3007, #47832, #33035, #29123 ),
 .UNSPECIFIED., .F., .F. ) 
 B_SPLINE_CURVE_WITH_KNOTS ( ( 4, 4 ),
 ( 0.5000000000000000000, 0.9074455897393701731 ),
 .UNSPECIFIED. ) 
 CURVE ( )  GEOMETRIC_REPRESENTATION_ITEM ( )  RATIONAL_B_SPLINE_CURVE ( ( 0.9999999999999942268, 0.4567392136813220871, 0.3561768502900305444, 0.6983129098261133816 ) ) 
 REPRESENTATION_ITEM ( '' )  );
#27431 = ORIENTED_EDGE ( 'NONE', *, *, #40842, .F. ) ;
#27432 = ORIENTED_EDGE ( 'NONE', *, *, #36789, .T. ) ;
#27433 = CARTESIAN_POINT ( 'NONE',  ( -23.19909385541303948, -8.105421454601382081, 49.25000573077640098 ) ) ;
#27434 = CARTESIAN_POINT ( 'NONE',  ( -19.17437844398820701, -7.979623566120205957, 63.44561363416070776 ) ) ;
#27435 = CARTESIAN_POINT ( 'NONE',  ( -19.17604249790256077, -21.63836284480991878, 58.53979515915469278 ) ) ;
#27436 = VECTOR ( 'NONE', #46675, 1000.000000000000114 ) ;
#27437 = ADVANCED_FACE ( 'NONE', ( #36932 ), #17502, .F. ) ;
#27438 =( BOUNDED_CURVE ( )  B_SPLINE_CURVE ( 3, ( #48515, #17506, #32537, #33475 ),
 .UNSPECIFIED., .F., .F. ) 
 B_SPLINE_CURVE_WITH_KNOTS ( ( 4, 4 ),
 ( 0.5000000000000000000, 0.9074455897393645110 ),
 .UNSPECIFIED. ) 
 CURVE ( )  GEOMETRIC_REPRESENTATION_ITEM ( )  RATIONAL_B_SPLINE_CURVE ( ( 1.000000000000020428, 0.4567392136813446801, 0.3561768502900207189, 0.6983129098260705270 ) ) 
 REPRESENTATION_ITEM ( '' )  );
#27439 = CARTESIAN_POINT ( 'NONE',  ( -10.77075464306150110, -16.98888295467523335, 61.22913362936283477 ) ) ;
#27440 = CARTESIAN_POINT ( 'NONE',  ( -20.81971067820157728, -8.177204663279967534, 59.95469905373763453 ) ) ;
#27441 = CARTESIAN_POINT ( 'NONE',  ( -9.979603264230430426, -14.52052340097724148, 68.04295441848455539 ) ) ;
#27442 = CARTESIAN_POINT ( 'NONE',  ( -18.19230087906959170, -22.21957251972233749, 65.38886231616686473 ) ) ;
#27443 = VERTEX_POINT ( 'NONE', #21218 ) ;
#27444 = CARTESIAN_POINT ( 'NONE',  ( -22.45002512565393005, -19.68157916873682467, 69.28304101961816741 ) ) ;
#27445 = EDGE_CURVE ( 'NONE', #10296, #26347, #12825, .T. ) ;
#27446 = CARTESIAN_POINT ( 'NONE',  ( -20.37299732318518508, -8.405577239842552117, 66.93104082189577753 ) ) ;
#27447 = ORIENTED_EDGE ( 'NONE', *, *, #17702, .T. ) ;
#27448 = CARTESIAN_POINT ( 'NONE',  ( -18.11889279746774051, -21.82488571228486052, 65.49532159284275679 ) ) ;
#27449 = CARTESIAN_POINT ( 'NONE',  ( -9.974122264712642405, -14.85722068285092057, 74.92062023727633857 ) ) ;
#27450 = ORIENTED_EDGE ( 'NONE', *, *, #18188, .T. ) ;
#27451 = CARTESIAN_POINT ( 'NONE',  ( -17.82409385541305369, -14.80920654474410725, 47.99999999999998579 ) ) ;
#27452 = CARTESIAN_POINT ( 'NONE',  ( -19.96784385759798752, -9.357632978295827186, 49.97845033065683396 ) ) ;
#27453 = CIRCLE ( 'NONE', #14070, 7.500000000000002665 ) ;
#27454 = CARTESIAN_POINT ( 'NONE',  ( -11.76425449931685030, -10.60075661872682140, 70.85404331479517737 ) ) ;
#27455 = CARTESIAN_POINT ( 'NONE',  ( -10.33431723597471930, -12.52035407725662886, 60.98348989824278732 ) ) ;
#27456 = LINE ( 'NONE', #8504, #11917 ) ;
#27457 = ORIENTED_EDGE ( 'NONE', *, *, #5822, .T. ) ;
#27458 = CARTESIAN_POINT ( 'NONE',  ( -22.00903739223959477, -8.936221312270376416, 63.30498424023031845 ) ) ;
#27459 = PLANE ( 'NONE',  #37594 ) ;
#27460 = AXIS2_PLACEMENT_3D ( 'NONE', #26142, #15272, #30820 ) ;
#27462 = CARTESIAN_POINT ( 'NONE',  ( -23.62389146642398075, -18.18225743695742835, 72.91935080803692415 ) ) ;
#27461 = VECTOR ( 'NONE', #37020, 1000.000000000000000 ) ;
#27463 = FACE_BOUND ( 'NONE', #1759, .T. ) ;
#27464 = SHAPE_DEFINITION_REPRESENTATION ( #22879, #41459 ) ;
#27465 = EDGE_CURVE ( 'NONE', #44063, #29613, #2252, .T. ) ;
#27466 = CARTESIAN_POINT ( 'NONE',  ( -11.43691971525006679, -18.43613410775878236, 58.03387880510997121 ) ) ;
#27467 = EDGE_CURVE ( 'NONE', #38209, #43090, #44592, .T. ) ;
#27468 = CARTESIAN_POINT ( 'NONE',  ( -12.91230480768039790, -16.07689808402359688, 49.52966884056655772 ) ) ;
#27469 = EDGE_LOOP ( 'NONE', ( #46440, #33750, #3300, #2480, #40422 ) ) ;
#27470 = AXIS2_PLACEMENT_3D ( 'NONE', #1297, #42921, #42194 ) ;
#27471 = ADVANCED_FACE ( 'NONE', ( #14030 ), #17260, .T. ) ;
#27472 = ORIENTED_EDGE ( 'NONE', *, *, #35721, .F. ) ;
#27473 = CARTESIAN_POINT ( 'NONE',  ( -11.41592704872699748, -19.21438508446953364, 71.94331831479362904 ) ) ;
#27474 = CARTESIAN_POINT ( 'NONE',  ( -11.99264457154321484, -10.30873963881685285, 64.02914301436621258 ) ) ;
#27475 = ORIENTED_EDGE ( 'NONE', *, *, #35235, .T. ) ;
#27476 = DIRECTION ( 'NONE',  ( -3.071710424422018668E-17, 6.404604876783312462E-16, 1.000000000000000000 ) ) ;
#27477 = FACE_BOUND ( 'NONE', #28782, .T. ) ;
#27478 = EDGE_LOOP ( 'NONE', ( #13229, #48093, #45863, #21552, #13903 ) ) ;
#27479 = VERTEX_POINT ( 'NONE', #32533 ) ;
#27480 = VERTEX_POINT ( 'NONE', #40401 ) ;
#27481 = CARTESIAN_POINT ( 'NONE',  ( -10.61330293760801879, -12.98832031645814844, 67.88832347272310130 ) ) ;
#27482 = CARTESIAN_POINT ( 'NONE',  ( -16.07284047765482882, -7.413310693310465993, 54.02312124697527906 ) ) ;
#27483 = CARTESIAN_POINT ( 'NONE',  ( -17.42409385541299471, -14.80920654474435771, 49.52966884056655772 ) ) ;
#27484 = EDGE_CURVE ( 'NONE', #1662, #1410, #25620, .T. ) ;
#27485 = CARTESIAN_POINT ( 'NONE',  ( -10.64854695470030599, -12.86019059820356958, 64.55364013863997741 ) ) ;
#27486 = CARTESIAN_POINT ( 'NONE',  ( -10.70785621775489993, -16.78775467540145527, 57.87687636479810749 ) ) ;
#27487 = EDGE_CURVE ( 'NONE', #16763, #26691, #48270, .T. ) ;
#27488 = EDGE_LOOP ( 'NONE', ( #13246, #21982, #26127, #5084 ) ) ;
#27489 = ORIENTED_EDGE ( 'NONE', *, *, #37472, .F. ) ;
#27490 = B_SPLINE_CURVE_WITH_KNOTS ( 'NONE', 3,
 ( #16139, #2109, #32159, #9756, #46456, #27486, #27966, #39777, #23811, #12712 ),
 .UNSPECIFIED., .F., .F.,
 ( 4, 2, 2, 2, 4 ),
 ( 0.000000000000000000, 0.2500000000000000000, 0.5000000000000000000, 0.7500000000000000000, 1.000000000000000000 ),
 .UNSPECIFIED. ) ;
#27491 = CARTESIAN_POINT ( 'NONE',  ( -20.81159385650551386, -6.922745924619793101, 51.69366785382590024 ) ) ;
#27492 = EDGE_CURVE ( 'NONE', #38648, #41019, #1392, .T. ) ;
#27493 = EDGE_CURVE ( 'NONE', #18739, #1846, #11197, .T. ) ;
#27494 = CARTESIAN_POINT ( 'NONE',  ( -24.00983782305545233, -11.32632323363204385, 66.57214513468635175 ) ) ;
#27495 = VECTOR ( 'NONE', #48329, 1000.000000000000000 ) ;
#27496 = CARTESIAN_POINT ( 'NONE',  ( -10.72552559342236833, -12.61109755851567549, 60.94853568372188590 ) ) ;
#27497 = CARTESIAN_POINT ( 'NONE',  ( -10.56492563526530759, -13.18000101695786341, 71.20828586226983248 ) ) ;
#27498 = EDGE_LOOP ( 'NONE', ( #38754, #42846 ) ) ;
#27499 = CARTESIAN_POINT ( 'NONE',  ( -13.46784385650551741, -6.428312510596451368, 51.20221977374900035 ) ) ;
#27500 = AXIS2_PLACEMENT_3D ( 'NONE', #38860, #42320, #1181 ) ;
#27501 = EDGE_LOOP ( 'NONE', ( #48151, #37121 ) ) ;
#27502 = CARTESIAN_POINT ( 'NONE',  ( -12.43154959716778940, -9.826441625128287782, 60.65098055540761379 ) ) ;
#27503 = CARTESIAN_POINT ( 'NONE',  ( -23.17409385650551457, -9.792211528768504536, 50.49490371617623197 ) ) ;
#27504 = FACE_OUTER_BOUND ( 'NONE', #41857, .T. ) ;
#27505 = VECTOR ( 'NONE', #35689, 1000.000000000000000 ) ;
#27506 = EDGE_LOOP ( 'NONE', ( #32904, #35543, #33930, #37293, #43682 ) ) ;
#27507 = CARTESIAN_POINT ( 'NONE',  ( -22.05757754724333353, -8.975236167248709762, 63.36870640580771408 ) ) ;
#27508 = ADVANCED_FACE ( 'NONE', ( #10384 ), #26766, .T. ) ;
#27509 = DIRECTION ( 'NONE',  ( 1.000000000000000000, 2.866981220435666553E-17, 0.000000000000000000 ) ) ;
#27510 = VERTEX_POINT ( 'NONE', #2726 ) ;
#27511 = CARTESIAN_POINT ( 'NONE',  ( -12.26315819337278334, -19.61226149452583911, 58.22122601348936399 ) ) ;
#27512 = CARTESIAN_POINT ( 'NONE',  ( -22.96484330895583881, -19.08706763331013434, 59.18410642315183878 ) ) ;
#27513 = CARTESIAN_POINT ( 'NONE',  ( -20.86860741727135959, -11.63137574808859931, 49.52966884056655772 ) ) ;
#27514 = ORIENTED_EDGE ( 'NONE', *, *, #24002, .T. ) ;
#27515 = DIRECTION ( 'NONE',  ( -0.6827297667453423591, -0.7306709694519486487, -5.176517812513565093E-09 ) ) ;
#27516 = VERTEX_POINT ( 'NONE', #14272 ) ;
#27517 = CARTESIAN_POINT ( 'NONE',  ( -9.974229878692264961, -14.74184183210034149, 71.48816083323411874 ) ) ;
#27518 = CARTESIAN_POINT ( 'NONE',  ( -14.91112529534803066, -8.221969756899694559, 57.13527940342243028 ) ) ;
#27520 = VERTEX_POINT ( 'NONE', #28605 ) ;
#27519 = EDGE_CURVE ( 'NONE', #45418, #26221, #31461, .T. ) ;
#27521 = DIRECTION ( 'NONE',  ( -3.071710424422018668E-17, 6.404604876783312462E-16, 1.000000000000000000 ) ) ;
#27522 = CARTESIAN_POINT ( 'NONE',  ( -12.50766578132126483, -19.86205079821699115, 65.16674886870754335 ) ) ;
#27523 = CARTESIAN_POINT ( 'NONE',  ( -12.58019717620059197, -16.04882945559874585, 52.02966884056655061 ) ) ;
#27524 = VECTOR ( 'NONE', #26801, 1000.000000000000000 ) ;
#27525 = LINE ( 'NONE', #38847, #11730 ) ;
#27526 = EDGE_LOOP ( 'NONE', ( #34758, #5611, #29167, #12116, #30397 ) ) ;
#27527 = CARTESIAN_POINT ( 'NONE',  ( -23.89081516821958218, -17.62458393556817171, 58.88889748697027926 ) ) ;
#27528 = AXIS2_PLACEMENT_3D ( 'NONE', #26863, #19456, #12792 ) ;
#27529 = CARTESIAN_POINT ( 'NONE',  ( -15.12070311848097859, -21.89431190412215145, 68.75405669007906795 ) ) ;
#27530 = CARTESIAN_POINT ( 'NONE',  ( -12.16129776675651897, -10.11277993467359337, 67.59076956020265925 ) ) ;
#27531 = CARTESIAN_POINT ( 'NONE',  ( -22.28350170462084989, -9.162040689504776125, 59.89983962365610637 ) ) ;
#27532 = ORIENTED_EDGE ( 'NONE', *, *, #43199, .T. ) ;
#27533 = LINE ( 'NONE', #19909, #30267 ) ;
#27534 = VECTOR ( 'NONE', #10956, 1000.000000000000000 ) ;
#27535 = B_SPLINE_CURVE_WITH_KNOTS ( 'NONE', 3,
 ( #20989, #28621, #31593, #23968, #38971, #5247, #12864, #42917, #9189, #39216 ),
 .UNSPECIFIED., .F., .F.,
 ( 4, 2, 2, 2, 4 ),
 ( 0.000000000000000000, 0.2500000000000000000, 0.5000000000000000000, 0.7500000000000000000, 1.000000000000000000 ),
 .UNSPECIFIED. ) ;
#27536 = CARTESIAN_POINT ( 'NONE',  ( -24.73185694657778910, -16.25806987106194512, 62.79339884040287245 ) ) ;
#27537 = VERTEX_POINT ( 'NONE', #43632 ) ;
#27538 = ORIENTED_EDGE ( 'NONE', *, *, #29312, .T. ) ;
#27539 = CARTESIAN_POINT ( 'NONE',  ( -24.84681873822328413, -14.17034522304293098, 69.79128769184926284 ) ) ;
#27540 = CARTESIAN_POINT ( 'NONE',  ( -13.54893327507986456, -8.910214905335239521, 64.05379690000981441 ) ) ;
#27541 = CARTESIAN_POINT ( 'NONE',  ( -24.72409385541305582, -15.80920654474410725, 65.99999999999998579 ) ) ;
#27542 = CIRCLE ( 'NONE', #3932, 2.000000000000000888 ) ;
#27543 = CARTESIAN_POINT ( 'NONE',  ( -22.13034385650552238, -9.794322478646142471, 51.19202720610083901 ) ) ;
#27544 = CARTESIAN_POINT ( 'NONE',  ( -12.34408071644948279, -9.993246969730000373, 57.28038814785139010 ) ) ;
#27545 = CARTESIAN_POINT ( 'NONE',  ( -12.37192322991513471, -19.65436620064385664, 58.11785611954050523 ) ) ;
#27546 = CARTESIAN_POINT ( 'NONE',  ( -24.85359113602694237, -14.25571898851532460, 69.76779851910008290 ) ) ;
#27547 = EDGE_CURVE ( 'NONE', #43778, #30777, #36906, .T. ) ;
#27548 = CARTESIAN_POINT ( 'NONE',  ( -45.92409385541306222, -13.70421070448076861, 70.50000000000000000 ) ) ;
#27549 = ORIENTED_EDGE ( 'NONE', *, *, #25377, .T. ) ;
#27550 = ORIENTED_EDGE ( 'NONE', *, *, #20559, .T. ) ;
#27551 = CARTESIAN_POINT ( 'NONE',  ( -11.08030728566740741, -11.72680384936461806, 74.97328630331448096 ) ) ;
#27552 = EDGE_CURVE ( 'NONE', #3552, #35369, #39921, .T. ) ;
#27553 = EDGE_CURVE ( 'NONE', #45387, #11424, #38532, .T. ) ;
#27554 = DIRECTION ( 'NONE',  ( 1.000000000000000000, 0.000000000000000000, 0.000000000000000000 ) ) ;
#27555 = CARTESIAN_POINT ( 'NONE',  ( -23.67460905091340706, -11.65500745809028338, 66.49384777452590356 ) ) ;
#27556 = CARTESIAN_POINT ( 'NONE',  ( -24.54463936542308744, -12.61820580661037106, 69.87219370530908691 ) ) ;
#27557 = CARTESIAN_POINT ( 'NONE',  ( -23.88415217903649079, -17.63235132829416685, 62.77360984996715842 ) ) ;
#27558 = EDGE_CURVE ( 'NONE', #21562, #47432, #37669, .T. ) ;
#27559 = EDGE_LOOP ( 'NONE', ( #42680, #31137, #19169, #11642, #36063 ) ) ;
#27560 = FACE_OUTER_BOUND ( 'NONE', #10600, .T. ) ;
#27561 = CYLINDRICAL_SURFACE ( 'NONE', #47318, 0.1499999999999974132 ) ;
#27562 = CIRCLE ( 'NONE', #29138, 1.250000000000001110 ) ;
#27563 = CYLINDRICAL_SURFACE ( 'NONE', #5656, 1.249999999999998668 ) ;
#27564 = CARTESIAN_POINT ( 'NONE',  ( -13.74909385541286788, -8.112991634885936776, 51.74999426922452272 ) ) ;
#27565 =( BOUNDED_CURVE ( )  B_SPLINE_CURVE ( 3, ( #4166, #7863, #45287, #7371 ),
 .UNSPECIFIED., .F., .F. ) 
 B_SPLINE_CURVE_WITH_KNOTS ( ( 4, 4 ),
 ( 0.5000000000000000000, 0.9074455897393631787 ),
 .UNSPECIFIED. ) 
 CURVE ( )  GEOMETRIC_REPRESENTATION_ITEM ( )  RATIONAL_B_SPLINE_CURVE ( ( 1.000000000000017319, 0.4567392136813416825, 0.3561768502900215516, 0.6983129098260758560 ) ) 
 REPRESENTATION_ITEM ( '' )  );
#27566 = ORIENTED_EDGE ( 'NONE', *, *, #22503, .T. ) ;
#27567 = VECTOR ( 'NONE', #46757, 1000.000000000000114 ) ;
#27568 = CARTESIAN_POINT ( 'NONE',  ( -24.42549660922115251, -13.91739599595199728, 69.80842429065324950 ) ) ;
#27569 = CARTESIAN_POINT ( 'NONE',  ( 23.52590614458706852, 1.890747609047893185, 50.53028072113869484 ) ) ;
#27570 = EDGE_CURVE ( 'NONE', #37730, #41749, #37921, .T. ) ;
#27571 = ORIENTED_EDGE ( 'NONE', *, *, #29940, .T. ) ;
#27572 = AXIS2_PLACEMENT_3D ( 'NONE', #5990, #43925, #36491 ) ;
#27573 = CARTESIAN_POINT ( 'NONE',  ( -12.23849770038826712, -15.62901903366650380, 49.52966884056655772 ) ) ;
#27574 = CARTESIAN_POINT ( 'NONE',  ( -16.17583575424048092, -10.27959207348368587, 52.02966884056656482 ) ) ;
#27575 = ORIENTED_EDGE ( 'NONE', *, *, #385, .F. ) ;
#27576 = CARTESIAN_POINT ( 'NONE',  ( -23.70015292207183322, -18.82353835121273988, 69.47867366044893345 ) ) ;
#27577 =( BOUNDED_SURFACE ( )  B_SPLINE_SURFACE ( 3, 1, ( 
 ( #6220, #17531 ),
 ( #21244, #9442 ),
 ( #36243, #46860 ),
 ( #2525, #43421 ),
 ( #20522, #32081 ),
 ( #35525, #9687 ),
 ( #35754, #1800 ) ),
 .UNSPECIFIED., .T., .F., .F. ) 
 B_SPLINE_SURFACE_WITH_KNOTS ( ( 4, 3, 4 ),
 ( 2, 2 ),
 ( 0.000000000000000000, 0.5000000000000000000, 1.000000000000000000 ),
 ( 0.000000000000000000, 1.000000000000000000 ),
 .UNSPECIFIED. ) 
 GEOMETRIC_REPRESENTATION_ITEM ( )  RATIONAL_B_SPLINE_SURFACE ( (
 ( 1.000000000000000000, 1.000000000000000000),
 ( 0.3333333333333335369, 0.3333333333333330373),
 ( 0.3333333333333335369, 0.3333333333333330373),
 ( 1.000000000000000000, 1.000000000000000000),
 ( 0.3333333333333333703, 0.3333333333333333703),
 ( 0.3333333333333333703, 0.3333333333333333703),
 ( 1.000000000000000000, 1.000000000000000000) ) ) 
 REPRESENTATION_ITEM ( '' )  SURFACE ( )  );
#27578 = ORIENTED_EDGE ( 'NONE', *, *, #28229, .F. ) ;
#27579 = EDGE_LOOP ( 'NONE', ( #18140, #29280 ) ) ;
#27580 = CARTESIAN_POINT ( 'NONE',  ( -23.74985771237617627, -17.93965049410213197, 62.61793715156320417 ) ) ;
#27581 = CARTESIAN_POINT ( 'NONE',  ( -17.98089531606498781, -21.84518143609853524, 68.95947724711012938 ) ) ;
#27582 = VECTOR ( 'NONE', #4030, 1000.000000000000000 ) ;
#27583 = CARTESIAN_POINT ( 'NONE',  ( -16.98659385650551812, -9.302874398569244363, 51.68646062012417985 ) ) ;
#27584 = CARTESIAN_POINT ( 'NONE',  ( -12.88390949798720619, -15.97110509908812936, 49.52966884056655772 ) ) ;
#27585 = CARTESIAN_POINT ( 'NONE',  ( -24.47638328979802225, -14.67261064969091322, 66.27472727418629006 ) ) ;
#27586 = CARTESIAN_POINT ( 'NONE',  ( -20.92409385541305511, -10.10920654474410618, 78.99999999999998579 ) ) ;
#27587 = ORIENTED_EDGE ( 'NONE', *, *, #26873, .F. ) ;
#27588 = FACE_OUTER_BOUND ( 'NONE', #14249, .T. ) ;
#27589 = CARTESIAN_POINT ( 'NONE',  ( -10.47425521701617157, -17.49314416303823450, 64.81234701634230078 ) ) ;
#27590 = DIRECTION ( 'NONE',  ( 2.081668171172170091E-15, 0.000000000000000000, -1.000000000000000000 ) ) ;
#27591 = FACE_OUTER_BOUND ( 'NONE', #24589, .T. ) ;
#27592 = AXIS2_PLACEMENT_3D ( 'NONE', #3942, #45078, #30296 ) ;
#27593 = CARTESIAN_POINT ( 'NONE',  ( -24.77321845510417830, -16.03108965430551436, 66.26313693903748003 ) ) ;
#27594 = EDGE_LOOP ( 'NONE', ( #30785, #5482, #2465, #992 ) ) ;
#27595 = EDGE_LOOP ( 'NONE', ( #15834, #11455, #10833, #9646 ) ) ;
#27596 = AXIS2_PLACEMENT_3D ( 'NONE', #45055, #468, #15446 ) ;
#27597 = CARTESIAN_POINT ( 'NONE',  ( -18.18338144371267617, -21.81849904615365432, 65.63060065626805795 ) ) ;
#27598 = CARTESIAN_POINT ( 'NONE',  ( -33.52409385541305653, -6.359206544744109735, 52.29999999999998295 ) ) ;
#27599 = VERTEX_POINT ( 'NONE', #15008 ) ;
#27600 = CARTESIAN_POINT ( 'NONE',  ( -24.35082266418244146, -15.81936897246520957, 66.25427998382291150 ) ) ;
#27601 = CARTESIAN_POINT ( 'NONE',  ( -22.44284385759799250, -7.587656875400192291, 49.25157356644813689 ) ) ;
#27602 = CARTESIAN_POINT ( 'NONE',  ( -24.37683822056718697, -15.97618770311995640, 66.06324926631656069 ) ) ;
#27603 = CARTESIAN_POINT ( 'NONE',  ( -11.24831865710118173, -11.40878463452673053, 64.44882016688482906 ) ) ;
#27604 = CARTESIAN_POINT ( 'NONE',  ( -12.28549284030545508, -10.05562942188838704, 60.55918091183862373 ) ) ;
#27605 = AXIS2_PLACEMENT_3D ( 'NONE', #23332, #5596, #20115 ) ;
#27606 = ORIENTED_EDGE ( 'NONE', *, *, #26525, .T. ) ;
#27607 = CARTESIAN_POINT ( 'NONE',  ( -22.42594789675818845, -19.77792426076253918, 69.45945937764655298 ) ) ;
#27608 = EDGE_CURVE ( 'NONE', #39678, #1919, #18973, .T. ) ;
#27609 =( NAMED_UNIT ( * ) PLANE_ANGLE_UNIT ( ) SI_UNIT ( $, .RADIAN. ) );
#27610 = VECTOR ( 'NONE', #30959, 1000.000000000000227 ) ;
#27611 = CARTESIAN_POINT ( 'NONE',  ( -12.30857103994386925, -9.957812909820729530, 60.56477846553902822 ) ) ;
#27612 = FACE_OUTER_BOUND ( 'NONE', #39176, .T. ) ;
#27613 = CARTESIAN_POINT ( 'NONE',  ( -23.12535539932854078, -10.01343808792704237, 66.65686846082743955 ) ) ;
#27614 = ORIENTED_EDGE ( 'NONE', *, *, #14486, .T. ) ;
#27615 = ORIENTED_EDGE ( 'NONE', *, *, #46462, .T. ) ;
#27616 = ADVANCED_FACE ( 'NONE', ( #45328 ), #21266, .T. ) ;
#27617 = DIRECTION ( 'NONE',  ( 8.993561279826231301E-07, -8.977735708137639859E-07, -0.9999999999991926458 ) ) ;
#27618 = EDGE_CURVE ( 'NONE', #1270, #8865, #13224, .T. ) ;
#27619 = ORIENTED_EDGE ( 'NONE', *, *, #38941, .F. ) ;
#27620 = CARTESIAN_POINT ( 'NONE',  ( -12.00971705810820467, -9.691755786776280246, 60.67422651510300113 ) ) ;
#27621 = CIRCLE ( 'NONE', #40974, 0.5000000000000004441 ) ;
#27622 = EDGE_CURVE ( 'NONE', #26632, #19018, #41974, .T. ) ;
#27623 = CARTESIAN_POINT ( 'NONE',  ( -24.07241877824284160, -12.61836747239114409, 69.96346150519261187 ) ) ;
#27624 = ADVANCED_FACE ( 'NONE', ( #15495 ), #10243, .F. ) ;
#27625 = ORIENTED_EDGE ( 'NONE', *, *, #34075, .T. ) ;
#27626 = CARTESIAN_POINT ( 'NONE',  ( -22.09908899289463591, -14.48102562737866705, 49.52966884056655772 ) ) ;
#27627 = B_SPLINE_CURVE_WITH_KNOTS ( 'NONE', 1,
 ( #18682, #249 ),
 .UNSPECIFIED., .F., .F.,
 ( 2, 2 ),
 ( 0.000000000000000000, 1.000000000000000000 ),
 .UNSPECIFIED. ) ;
#27628 =( GEOMETRIC_REPRESENTATION_CONTEXT ( 3 ) GLOBAL_UNCERTAINTY_ASSIGNED_CONTEXT ( ( #1671 ) ) GLOBAL_UNIT_ASSIGNED_CONTEXT ( ( #47548, #5937, #25138 ) ) REPRESENTATION_CONTEXT ( 'NONE', 'WORKASPACE' ) );
#27629 = CARTESIAN_POINT ( 'NONE',  ( -10.39693166811831304, -15.37990016280386918, 57.58264896457095006 ) ) ;
#27630 = ADVANCED_FACE ( 'NONE', ( #30800 ), #45818, .T. ) ;
#27631 = VERTEX_POINT ( 'NONE', #28050 ) ;
#27632 = CARTESIAN_POINT ( 'NONE',  ( -23.14996626141612523, -18.92247510852853765, 62.64847065521940550 ) ) ;
#27633 = VERTEX_POINT ( 'NONE', #35193 ) ;
#27634 = CARTESIAN_POINT ( 'NONE',  ( -11.32267065936820316, -11.37785446942383949, 64.14882076995250770 ) ) ;
#27635 = VECTOR ( 'NONE', #18708, 1000.000000000000114 ) ;
#27636 = CARTESIAN_POINT ( 'NONE',  ( -23.59327504554355315, -11.39630409041826020, 69.90682860766239060 ) ) ;
#27637 = EDGE_LOOP ( 'NONE', ( #33435, #30048, #5983, #3836, #16691 ) ) ;
#27638 = CARTESIAN_POINT ( 'NONE',  ( -24.47304815678895196, -15.04811744431364140, 59.65788834854969735 ) ) ;
#27639 = CARTESIAN_POINT ( 'NONE',  ( -12.36794914932409561, -19.72224030764921565, 61.39678633597973345 ) ) ;
#27640 = CARTESIAN_POINT ( 'NONE',  ( -19.03984369153074141, -21.67464089235836511, 58.93996235972087305 ) ) ;
#27641 = ORIENTED_EDGE ( 'NONE', *, *, #9354, .T. ) ;
#27642 = LINE ( 'NONE', #35734, #1079 ) ;
#27643 = DIRECTION ( 'NONE',  ( -3.071710424422018668E-17, 6.404604876783312462E-16, 1.000000000000000000 ) ) ;
#27644 = AXIS2_PLACEMENT_3D ( 'NONE', #4927, #8366, #34939 ) ;
#27645 = CARTESIAN_POINT ( 'NONE',  ( -10.78978129071826686, -12.42417052737943095, 57.32857332104951098 ) ) ;
#27646 = CARTESIAN_POINT ( 'NONE',  ( -7.424093855413048892, -25.10920654474410441, 63.99999999999998579 ) ) ;
#27647 = DIRECTION ( 'NONE',  ( -0.000000000000000000, -1.000000000000000000, -0.000000000000000000 ) ) ;
#27648 = VERTEX_POINT ( 'NONE', #38396 ) ;
#27649 = DIRECTION ( 'NONE',  ( -5.731567514496413899E-31, -1.020425574103664789E-16, -1.000000000000000000 ) ) ;
#27650 = PLANE ( 'NONE',  #44734 ) ;
#27651 = CARTESIAN_POINT ( 'NONE',  ( -15.89884937297370193, -7.926133255677830114, 67.14007309771254484 ) ) ;
#27652 = CARTESIAN_POINT ( 'NONE',  ( -18.02409385650551599, -6.426201560718813433, 50.50509628382439331 ) ) ;
#27653 = AXIS2_PLACEMENT_3D ( 'NONE', #33739, #3720, #29335 ) ;
#27654 = ORIENTED_EDGE ( 'NONE', *, *, #13657, .T. ) ;
#27655 = CARTESIAN_POINT ( 'NONE',  ( -10.42302287260171312, -13.97751933429587012, 57.73352905910142852 ) ) ;
#27656 = DIRECTION ( 'NONE',  ( 0.6264825908887947659, -0.7794354131762692983, 3.858680029754496854E-08 ) ) ;
#27657 = VERTEX_POINT ( 'NONE', #46549 ) ;
#27658 = LINE ( 'NONE', #1300, #15016 ) ;
#27659 = CARTESIAN_POINT ( 'NONE',  ( -14.98896517277256635, -21.85004359773310156, 65.21258386126636708 ) ) ;
#27661 = CARTESIAN_POINT ( 'NONE',  ( -21.29196722032537537, -20.70380199363843232, 72.53918572867779346 ) ) ;
#27660 =( BOUNDED_CURVE ( )  B_SPLINE_CURVE ( 3, ( #39590, #5867, #42811, #42586 ),
 .UNSPECIFIED., .F., .F. ) 
 B_SPLINE_CURVE_WITH_KNOTS ( ( 4, 4 ),
 ( 0.4074455897393656767, 0.5000000000000000000 ),
 .UNSPECIFIED. ) 
 CURVE ( )  GEOMETRIC_REPRESENTATION_ITEM ( )  RATIONAL_B_SPLINE_CURVE ( ( 0.6983129098260891787, 0.7760317562606972031, 0.8765941196520016243, 1.000000000000003775 ) ) 
 REPRESENTATION_ITEM ( '' )  );
#27662 = CARTESIAN_POINT ( 'NONE',  ( -22.44308142039503906, -9.846875392603276822, 70.16745681354213104 ) ) ;
#27663 = CARTESIAN_POINT ( 'NONE',  ( -20.72573862760241070, -8.580110178657996300, 60.14125250079693785 ) ) ;
#27664 = EDGE_CURVE ( 'NONE', #30899, #48422, #34430, .T. ) ;
#27665 = ORIENTED_EDGE ( 'NONE', *, *, #22655, .F. ) ;
#27666 = DIRECTION ( 'NONE',  ( 0.9999889394985579383, 0.004703284017506803583, -7.734398264755851970E-09 ) ) ;
#27667 = DIRECTION ( 'NONE',  ( 1.149299188226319421E-05, -1.849289876324834950E-06, 0.9999999999322456423 ) ) ;
#27668 = CIRCLE ( 'NONE', #48114, 0.3999999999999975797 ) ;
#27669 = CARTESIAN_POINT ( 'NONE',  ( -11.91307475890685552, -9.794993484201089728, 60.67262835395951015 ) ) ;
#27670 = EDGE_CURVE ( 'NONE', #8529, #16401, #993, .T. ) ;
#27671 = ORIENTED_EDGE ( 'NONE', *, *, #4365, .T. ) ;
#27672 = CARTESIAN_POINT ( 'NONE',  ( -11.43788345834500220, -18.53998761144092455, 58.01534399077101511 ) ) ;
#27673 = AXIS2_PLACEMENT_3D ( 'NONE', #15233, #7149, #6653 ) ;
#27674 = DIRECTION ( 'NONE',  ( 0.000000000000000000, -0.9999954153791273948, -0.003028072113819838245 ) ) ;
#27675 = CARTESIAN_POINT ( 'NONE',  ( -17.19811928533322387, -9.313850733363548073, 54.07175714974879099 ) ) ;
#27676 = DIRECTION ( 'NONE',  ( 4.115385489419834812E-17, 0.9999954153791273948, 0.003028072113822188795 ) ) ;
#27677 = DIRECTION ( 'NONE',  ( -0.000000000000000000, -1.000000000000000000, -0.000000000000000000 ) ) ;
#27678 = VERTEX_POINT ( 'NONE', #4940 ) ;
#27679 = VERTEX_POINT ( 'NONE', #27810 ) ;
#27680 = CARTESIAN_POINT ( 'NONE',  ( -20.72409385541304161, -9.359200813967568422, 50.49621490985803263 ) ) ;
#27681 = DIRECTION ( 'NONE',  ( -0.8447509909909771686, 0.5351595679979589404, 0.000000000000000000 ) ) ;
#27682 = EDGE_CURVE ( 'NONE', #15747, #31661, #41369, .T. ) ;
#27683 = CARTESIAN_POINT ( 'NONE',  ( -14.04552000357412211, -8.169287140739843522, 70.92231787642808172 ) ) ;
#27684 = EDGE_CURVE ( 'NONE', #37849, #45322, #18882, .T. ) ;
#27685 = EDGE_CURVE ( 'NONE', #22071, #29021, #33824, .T. ) ;
#27686 = CARTESIAN_POINT ( 'NONE',  ( -14.20445937233222367, -8.593517467233848350, 70.74460083025394397 ) ) ;
#27687 = LINE ( 'NONE', #16589, #2594 ) ;
#27688 = ORIENTED_EDGE ( 'NONE', *, *, #18660, .F. ) ;
#27689 = CARTESIAN_POINT ( 'NONE',  ( -18.92057809895272058, -7.919864474132484844, 66.90071783790342863 ) ) ;
#27690 = CARTESIAN_POINT ( 'NONE',  ( -24.23070293473816506, -17.83824296527514264, 62.63507471626854084 ) ) ;
#27691 = EDGE_CURVE ( 'NONE', #43420, #40354, #35566, .T. ) ;
#27692 = ORIENTED_EDGE ( 'NONE', *, *, #26597, .F. ) ;
#27693 = CARTESIAN_POINT ( 'NONE',  ( -23.77562434277295367, -17.86939608417919345, 59.01850491586762359 ) ) ;
#27694 = CARTESIAN_POINT ( 'NONE',  ( -17.14068089774974624, -7.813665893538186857, 74.18848128627297456 ) ) ;
#27695 = ORIENTED_EDGE ( 'NONE', *, *, #25485, .T. ) ;
#27696 = B_SPLINE_CURVE_WITH_KNOTS ( 'NONE', 1,
 ( #10841, #28827 ),
 .UNSPECIFIED., .F., .F.,
 ( 2, 2 ),
 ( 0.000000000000000000, 1.000000000000000000 ),
 .UNSPECIFIED. ) ;
#27697 = CARTESIAN_POINT ( 'NONE',  ( -12.41310947992116098, -19.76871611099698001, 61.68206578716802113 ) ) ;
#27698 = ORIENTED_EDGE ( 'NONE', *, *, #44407, .F. ) ;
#27699 = CARTESIAN_POINT ( 'NONE',  ( -6.424093855413055110, -25.10920654474410441, 45.99999999999998579 ) ) ;
#27700 =( BOUNDED_SURFACE ( )  B_SPLINE_SURFACE ( 3, 1, ( 
 ( #4135, #41547 ),
 ( #14666, #37583 ),
 ( #41058, #19134 ),
 ( #45747, #26526 ),
 ( #34142, #435 ),
 ( #38078, #18627 ),
 ( #11997, #11266 ) ),
 .UNSPECIFIED., .T., .F., .F. ) 
 B_SPLINE_SURFACE_WITH_KNOTS ( ( 4, 3, 4 ),
 ( 2, 2 ),
 ( 0.000000000000000000, 0.5000000000000000000, 1.000000000000000000 ),
 ( 0.000000000000000000, 1.000000000000000000 ),
 .UNSPECIFIED. ) 
 GEOMETRIC_REPRESENTATION_ITEM ( )  RATIONAL_B_SPLINE_SURFACE ( (
 ( 1.000000000000000000, 1.000000000000000000),
 ( 0.3333333333333335369, 0.3333333333333330373),
 ( 0.3333333333333335369, 0.3333333333333330373),
 ( 1.000000000000000000, 1.000000000000000000),
 ( 0.3333333333333333703, 0.3333333333333333703),
 ( 0.3333333333333333703, 0.3333333333333333703),
 ( 1.000000000000000000, 1.000000000000000000) ) ) 
 REPRESENTATION_ITEM ( '' )  SURFACE ( )  );
#27701 = CARTESIAN_POINT ( 'NONE',  ( -19.28352822169459202, -22.07505156356299381, 53.49999999999994316 ) ) ;
#27702 = CARTESIAN_POINT ( 'NONE',  ( -22.53422763456337918, -19.59328113293763352, 72.65903032234385250 ) ) ;
#27703 = EDGE_LOOP ( 'NONE', ( #28570, #34777, #33198, #36229, #31911 ) ) ;
#27704 = CARTESIAN_POINT ( 'NONE',  ( -11.21783165637758550, -18.93062460193366192, 64.93202459354702683 ) ) ;
#27705 = DIRECTION ( 'NONE',  ( -3.071710424422018668E-17, 6.404604876783312462E-16, 1.000000000000000000 ) ) ;
#27706 = LINE ( 'NONE', #42737, #42773 ) ;
#27707 = CYLINDRICAL_SURFACE ( 'NONE', #28935, 0.1500000000000039913 ) ;
#27708 = CARTESIAN_POINT ( 'NONE',  ( -23.04367560227575140, -10.55211830211007218, 59.60203429193362723 ) ) ;
#27709 = CARTESIAN_POINT ( 'NONE',  ( -11.46947271230222931, -11.12676175853379412, 60.90715737523439799 ) ) ;
#27710 = LINE ( 'NONE', #27228, #12490 ) ;
#27711 = EDGE_LOOP ( 'NONE', ( #20034, #26570, #6287 ) ) ;
#27712 = CARTESIAN_POINT ( 'NONE',  ( -12.14070192025202743, -10.21533219252760105, 67.72726724898851103 ) ) ;
#27713 = VERTEX_POINT ( 'NONE', #31996 ) ;
#27714 = CARTESIAN_POINT ( 'NONE',  ( -11.63532267033605372, -18.83847007233952908, 72.10174756685907482 ) ) ;
#27715 = CARTESIAN_POINT ( 'NONE',  ( -17.59331747086620013, -7.761237804118463757, 63.85057029381062677 ) ) ;
#27716 = ADVANCED_FACE ( 'NONE', ( #35436, #31265 ), #8631, .F. ) ;
#27717 = ORIENTED_EDGE ( 'NONE', *, *, #7915, .T. ) ;
#27718 =( BOUNDED_CURVE ( )  B_SPLINE_CURVE ( 3, ( #21603, #17875, #32204, #33141 ),
 .UNSPECIFIED., .F., .F. ) 
 B_SPLINE_CURVE_WITH_KNOTS ( ( 4, 4 ),
 ( 0.000000000000000000, 0.4074455897393596815 ),
 .UNSPECIFIED. ) 
 CURVE ( )  GEOMETRIC_REPRESENTATION_ITEM ( )  RATIONAL_B_SPLINE_CURVE ( ( 1.000000000000000000, 0.4567392136813367975, 0.3561768502900320987, 0.6983129098260858481 ) ) 
 REPRESENTATION_ITEM ( '' )  );
#27719 = CARTESIAN_POINT ( 'NONE',  ( -21.52725980274252393, -9.076272844571150245, 70.43132538913751262 ) ) ;
#27720 = FACE_BOUND ( 'NONE', #39647, .T. ) ;
#27721 = ORIENTED_EDGE ( 'NONE', *, *, #8108, .T. ) ;
#27722 = VERTEX_POINT ( 'NONE', #31756 ) ;
#27723 = ORIENTED_EDGE ( 'NONE', *, *, #40893, .T. ) ;
#27724 = CARTESIAN_POINT ( 'NONE',  ( -17.84478125091072087, -22.24806977446377942, 62.06191208170499607 ) ) ;
#27725 = FACE_OUTER_BOUND ( 'NONE', #39427, .T. ) ;
#27726 = CYLINDRICAL_SURFACE ( 'NONE', #11016, 1.999999999999999556 ) ;
#27727 = CARTESIAN_POINT ( 'NONE',  ( -12.58533692436079754, -19.86927994801577668, 68.40827630894551703 ) ) ;
#27728 = CARTESIAN_POINT ( 'NONE',  ( -22.82405744922300528, -15.92202671434138672, 53.69233794759168887 ) ) ;
#27729 =( BOUNDED_SURFACE ( )  B_SPLINE_SURFACE ( 3, 1, ( 
 ( #31676, #42765 ),
 ( #4856, #1873 ),
 ( #9037, #23816 ),
 ( #16146, #20600 ),
 ( #31189, #35598 ),
 ( #16874, #28221 ),
 ( #24053, #43253 ) ),
 .UNSPECIFIED., .T., .F., .F. ) 
 B_SPLINE_SURFACE_WITH_KNOTS ( ( 4, 3, 4 ),
 ( 2, 2 ),
 ( 0.000000000000000000, 0.5000000000000000000, 1.000000000000000000 ),
 ( 0.000000000000000000, 1.000000000000000000 ),
 .UNSPECIFIED. ) 
 GEOMETRIC_REPRESENTATION_ITEM ( )  RATIONAL_B_SPLINE_SURFACE ( (
 ( 1.000000000000000000, 1.000000000000000000),
 ( 0.3333333333333335369, 0.3333333333333330373),
 ( 0.3333333333333335369, 0.3333333333333330373),
 ( 1.000000000000000000, 1.000000000000000000),
 ( 0.3333333333333333703, 0.3333333333333333703),
 ( 0.3333333333333333703, 0.3333333333333333703),
 ( 1.000000000000000000, 1.000000000000000000) ) ) 
 REPRESENTATION_ITEM ( '' )  SURFACE ( )  );
#27730 = ORIENTED_EDGE ( 'NONE', *, *, #3199, .T. ) ;
#27731 = ORIENTED_EDGE ( 'NONE', *, *, #6339, .T. ) ;
#27732 = CARTESIAN_POINT ( 'NONE',  ( -10.35661267713556022, -12.45241038966069347, 60.91358145539074798 ) ) ;
#27733 = EDGE_CURVE ( 'NONE', #20377, #39922, #46431, .T. ) ;
#27734 = DIRECTION ( 'NONE',  ( -3.071710424422018668E-17, 6.404604876783312462E-16, 1.000000000000000000 ) ) ;
#27735 = FACE_OUTER_BOUND ( 'NONE', #45928, .T. ) ;
#27736 = DIRECTION ( 'NONE',  ( 0.4683180279402422430, -0.8835599723313412035, 4.589753183357165928E-08 ) ) ;
#27737 = CARTESIAN_POINT ( 'NONE',  ( -22.16159385650551528, -9.295667164867525756, 49.30633214617472504 ) ) ;
#27738 = EDGE_LOOP ( 'NONE', ( #2749, #28405, #13723, #20889 ) ) ;
#27739 = EDGE_CURVE ( 'NONE', #27062, #383, #31481, .T. ) ;
#27740 = CARTESIAN_POINT ( 'NONE',  ( -14.74177589038128033, -21.75963160520128170, 61.82938730834030849 ) ) ;
#27741 = CARTESIAN_POINT ( 'NONE',  ( -12.05615996164320691, -19.97535249625256526, 61.51183308442717390 ) ) ;
#27742 = CARTESIAN_POINT ( 'NONE',  ( -12.44661323591510715, -19.73288383789282463, 65.09504664347453229 ) ) ;
#27743 = ADVANCED_FACE ( 'NONE', ( #42613 ), #32707, .T. ) ;
#27744 = ORIENTED_EDGE ( 'NONE', *, *, #26392, .F. ) ;
#27745 = B_SPLINE_CURVE_WITH_KNOTS ( 'NONE', 3,
 ( #29578, #44608, #25886, #40901 ),
 .UNSPECIFIED., .F., .F.,
 ( 4, 4 ),
 ( 0.001310108020966226300, 0.002761379516309090103 ),
 .UNSPECIFIED. ) ;
#27746 = CARTESIAN_POINT ( 'NONE',  ( -12.91576191806997365, -9.388722997169709927, 71.13453240065665284 ) ) ;
#27747 = CARTESIAN_POINT ( 'NONE',  ( -24.42218830512229388, -14.64588455312011739, 63.01296487252135137 ) ) ;
#27748 = CARTESIAN_POINT ( 'NONE',  ( -10.42892865687001169, -14.54580309686654083, 68.15800118612639835 ) ) ;
#27749 = CARTESIAN_POINT ( 'NONE',  ( -14.40728840208385542, -7.997212190190129633, 63.96695762048931755 ) ) ;
#27750 = VECTOR ( 'NONE', #28175, 1000.000000000000227 ) ;
#27751 = EDGE_LOOP ( 'NONE', ( #20605, #29767, #2122, #6146 ) ) ;
#27752 = DIRECTION ( 'NONE',  ( -0.8017593358536256876, -0.5976470257363775129, 1.209213344977627448E-07 ) ) ;
#27753 = EDGE_CURVE ( 'NONE', #16463, #33928, #32249, .T. ) ;
#27754 = DIRECTION ( 'NONE',  ( -0.000000000000000000, -1.000000000000000000, -0.000000000000000000 ) ) ;
#27755 = CARTESIAN_POINT ( 'NONE',  ( -11.42761092774205345, -18.42145285602150651, 61.56094325674602885 ) ) ;
#27756 = ORIENTED_EDGE ( 'NONE', *, *, #42783, .F. ) ;
#27757 = FACE_OUTER_BOUND ( 'NONE', #42169, .T. ) ;
#27758 = EDGE_CURVE ( 'NONE', #2612, #33183, #3308, .T. ) ;
#27759 = ORIENTED_EDGE ( 'NONE', *, *, #12475, .T. ) ;
#27760 = CARTESIAN_POINT ( 'NONE',  ( -19.19517940744574602, -7.572777289964699676, 63.53065599075442549 ) ) ;
#27761 = CARTESIAN_POINT ( 'NONE',  ( -14.61275832261265784, -7.909957978881497098, 60.42657991558792219 ) ) ;
#27762 = ORIENTED_EDGE ( 'NONE', *, *, #29523, .F. ) ;
#27763 = EDGE_CURVE ( 'NONE', #13430, #6817, #29891, .T. ) ;
#27764 = DIRECTION ( 'NONE',  ( -0.9243256318339801991, 0.3816046728418207024, -8.614662759602030584E-09 ) ) ;
#27765 = CARTESIAN_POINT ( 'NONE',  ( -17.50221816081645798, -7.047512361584055363, 53.27966884056655061 ) ) ;
#27766 = CARTESIAN_POINT ( 'NONE',  ( -24.25372093726098655, -13.26839283772111955, 62.90434541420221137 ) ) ;
#27767 = B_SPLINE_CURVE_WITH_KNOTS ( 'NONE', 3,
 ( #30782, #4921, #38136, #31491, #46529, #41607, #15474, #34439, #45561, #37903 ),
 .UNSPECIFIED., .F., .F.,
 ( 4, 2, 2, 2, 4 ),
 ( 0.000000000000000000, 0.2500000000000000000, 0.5000000000000000000, 0.7500000000000000000, 1.000000000000000000 ),
 .UNSPECIFIED. ) ;
#27768 = DIRECTION ( 'NONE',  ( -0.4501286257827957216, -0.8929637284072022840, 1.500157795982635434E-08 ) ) ;
#27769 = EDGE_LOOP ( 'NONE', ( #45609, #21281 ) ) ;
#27770 = CARTESIAN_POINT ( 'NONE',  ( -24.12016595861979695, -18.07666464397348349, 59.19033703419022885 ) ) ;
#27771 = CARTESIAN_POINT ( 'NONE',  ( -15.11389443855535220, -21.89214149219162309, 68.73739423610683730 ) ) ;
#27772 = CARTESIAN_POINT ( 'NONE',  ( -10.51631473918724780, -16.23308084970759069, 67.86278957288837432 ) ) ;
#27773 = ORIENTED_EDGE ( 'NONE', *, *, #46172, .T. ) ;
#27774 = CARTESIAN_POINT ( 'NONE',  ( -10.37578944195559494, -14.53307773176141815, 64.38803750143166837 ) ) ;
#27775 = FACE_OUTER_BOUND ( 'NONE', #45810, .T. ) ;
#27776 = ORIENTED_EDGE ( 'NONE', *, *, #23391, .F. ) ;
#27777 = ORIENTED_EDGE ( 'NONE', *, *, #31082, .T. ) ;
#27778 = CARTESIAN_POINT ( 'NONE',  ( -23.42856991828856650, -18.40753713903406918, 72.76368185885715434 ) ) ;
#27779 = CARTESIAN_POINT ( 'NONE',  ( -19.96994565995125015, -21.32983830779690848, 72.70478737306767414 ) ) ;
#27780 = CARTESIAN_POINT ( 'NONE',  ( -11.29219319990544079, -18.28864530752396433, 57.82186711835544912 ) ) ;
#27781 = CARTESIAN_POINT ( 'NONE',  ( -16.56159385650551386, -9.295667164867525756, 49.30633214617472504 ) ) ;
#27782 = LINE ( 'NONE', #8848, #31322 ) ;
#27783 = CARTESIAN_POINT ( 'NONE',  ( -16.50258162057404832, -20.23145840177225452, 54.07175714974879099 ) ) ;
#27784 = CARTESIAN_POINT ( 'NONE',  ( -24.27602536896142738, -13.14965745380569828, 62.83264206442589028 ) ) ;
#27785 = B_SPLINE_CURVE_WITH_KNOTS ( 'NONE', 3,
 ( #40510, #16943, #47001, #2183, #46768, #35902, #14378, #28042, #5658, #3570 ),
 .UNSPECIFIED., .F., .F.,
 ( 4, 2, 2, 2, 4 ),
 ( 0.1272669073657635708, 0.2522669073487474045, 0.3772669073317311828, 0.5022669073147150165, 0.6272669072976988502 ),
 .UNSPECIFIED. ) ;
#27786 = CARTESIAN_POINT ( 'NONE',  ( -22.87867891474110849, -19.28048576922455837, 59.29899440274890310 ) ) ;
#27787 = ORIENTED_EDGE ( 'NONE', *, *, #21741, .F. ) ;
#27788 = VERTEX_POINT ( 'NONE', #29273 ) ;
#27789 = CARTESIAN_POINT ( 'NONE',  ( -11.03230825063491594, -10.98182429003440674, 60.79390496990795612 ) ) ;
#27790 = DIRECTION ( 'NONE',  ( 0.000000000000000000, 0.000000000000000000, 1.000000000000000000 ) ) ;
#27791 = VECTOR ( 'NONE', #4442, 1000.000000000000000 ) ;
#27792 = CARTESIAN_POINT ( 'NONE',  ( -22.63659385541299685, -8.995762431863267850, 51.38120296130590958 ) ) ;
#27793 = CARTESIAN_POINT ( 'NONE',  ( -13.32057209662121267, -9.066726955530414855, 57.12534593251891124 ) ) ;
#27794 = CARTESIAN_POINT ( 'NONE',  ( -20.96474559848019226, -20.91483931500396309, 58.80042297414523489 ) ) ;
#27795 = EDGE_LOOP ( 'NONE', ( #37547, #30301, #48600, #1817 ) ) ;
#27796 = EDGE_CURVE ( 'NONE', #23337, #10698, #20314, .T. ) ;
#27797 = DIRECTION ( 'NONE',  ( 2.231660450020913765E-16, 0.9999954153791275058, 0.003028072113822189229 ) ) ;
#27798 = CARTESIAN_POINT ( 'NONE',  ( -10.33431723597471930, -12.52035407725662886, 60.98348989824278732 ) ) ;
#27799 = EDGE_CURVE ( 'NONE', #10314, #31867, #21821, .T. ) ;
#27800 = CARTESIAN_POINT ( 'NONE',  ( -15.55847894090159933, -21.55608122201934052, 72.06077882257353906 ) ) ;
#27801 = CARTESIAN_POINT ( 'NONE',  ( -11.09194279281618556, -18.73431720802965117, 61.47699602486266457 ) ) ;
#27802 = ORIENTED_EDGE ( 'NONE', *, *, #5131, .T. ) ;
#27803 = CARTESIAN_POINT ( 'NONE',  ( -20.80117294895647717, -20.99790032493542213, 62.12031196887301121 ) ) ;
#27804 = DIRECTION ( 'NONE',  ( -3.071710424422018668E-17, 6.404604876783312462E-16, 1.000000000000000000 ) ) ;
#27805 = ORIENTED_EDGE ( 'NONE', *, *, #11132, .T. ) ;
#27806 = DIRECTION ( 'NONE',  ( 0.000000000000000000, 1.000000000000000000, -0.000000000000000000 ) ) ;
#27807 = DIRECTION ( 'NONE',  ( 8.262539640598030559E-06, -9.998826076706305650E-07, -0.9999999999653652605 ) ) ;
#27808 = CARTESIAN_POINT ( 'NONE',  ( -24.23444905059911392, -16.42945129436568408, 59.40715929003106055 ) ) ;
#27809 = ORIENTED_EDGE ( 'NONE', *, *, #10803, .F. ) ;
#27810 = CARTESIAN_POINT ( 'NONE',  ( -22.26799053462541522, -13.56958363389006905, 53.27966884056655061 ) ) ;
#27811 = ADVANCED_FACE ( 'NONE', ( #39862 ), #14218, .T. ) ;
#27812 = EDGE_LOOP ( 'NONE', ( #3222, #14692, #19470, #43602, #25714 ) ) ;
#27813 = DIRECTION ( 'NONE',  ( 2.866981220435666553E-17, -1.000000000000000000, -1.190614954331866791E-16 ) ) ;
#27814 = CARTESIAN_POINT ( 'NONE',  ( -18.44528782684011503, -21.78515541812411982, 72.29983070759432451 ) ) ;
#27815 = ORIENTED_EDGE ( 'NONE', *, *, #30594, .T. ) ;
#27816 = CARTESIAN_POINT ( 'NONE',  ( -19.81074488107690001, -24.17086428735163040, 54.49999999999995026 ) ) ;
#27817 = EDGE_CURVE ( 'NONE', #13690, #13051, #25979, .T. ) ;
#27818 = EDGE_CURVE ( 'NONE', #47353, #32996, #10557, .T. ) ;
#27819 = EDGE_CURVE ( 'NONE', #11232, #32982, #5897, .T. ) ;
#27820 = CARTESIAN_POINT ( 'NONE',  ( -15.94284385541290483, -7.587656875400093703, 49.25157356644789530 ) ) ;
#27821 = AXIS2_PLACEMENT_3D ( 'NONE', #36231, #9676, #47091 ) ;
#27822 = CARTESIAN_POINT ( 'NONE',  ( -18.05534385650551599, -7.417179338643134834, 52.18511593390279302 ) ) ;
#27823 = ORIENTED_EDGE ( 'NONE', *, *, #27465, .F. ) ;
#27824 = FACE_OUTER_BOUND ( 'NONE', #13040, .T. ) ;
#27825 = CARTESIAN_POINT ( 'NONE',  ( -24.08343163355289818, -12.65065354144157084, 73.52609009109720262 ) ) ;
#27826 = CARTESIAN_POINT ( 'NONE',  ( -16.18802525292456096, -21.75305063948447426, 62.17057002965735535 ) ) ;
#27827 = ORIENTED_EDGE ( 'NONE', *, *, #30733, .T. ) ;
#27828 = CARTESIAN_POINT ( 'NONE',  ( -23.85492384001828725, -17.57437228381108341, 62.47360986607454691 ) ) ;
#27829 = CARTESIAN_POINT ( 'NONE',  ( -12.73044152958719977, -14.59664269629646682, 49.52966884056655772 ) ) ;
#27830 = CYLINDRICAL_SURFACE ( 'NONE', #40747, 0.1500000000000043243 ) ;
#27831 = CARTESIAN_POINT ( 'NONE',  ( -24.61605457543312525, -12.86511826566283290, 66.41751344402152313 ) ) ;
#27832 = DIRECTION ( 'NONE',  ( -0.3303050442826436228, 0.9438742382973701606, 3.829623549872328137E-09 ) ) ;
#27833 = ORIENTED_EDGE ( 'NONE', *, *, #8114, .F. ) ;
#27834 = ORIENTED_EDGE ( 'NONE', *, *, #38866, .T. ) ;
#27835 = CARTESIAN_POINT ( 'NONE',  ( -11.72780659764178601, -18.87776260402302597, 68.23192005210353273 ) ) ;
#27836 = CARTESIAN_POINT ( 'NONE',  ( -22.29619887594318328, -17.36118473213641167, 54.07175714974878389 ) ) ;
#27837 = ORIENTED_EDGE ( 'NONE', *, *, #33689, .F. ) ;
#27838 = DIRECTION ( 'NONE',  ( 3.413470714839332458E-33, -1.190614954331866791E-16, 1.000000000000000000 ) ) ;
#27839 = CARTESIAN_POINT ( 'NONE',  ( -24.17899278864585355, -11.66673636667039027, 59.66731167108189737 ) ) ;
#27840 = CARTESIAN_POINT ( 'NONE',  ( -19.06784385759798894, -9.357632978295830739, 49.97845033065684106 ) ) ;
#27841 = CARTESIAN_POINT ( 'NONE',  ( -13.01970113850136634, -8.800494951336613525, 64.10220657692070745 ) ) ;
#27842 = CARTESIAN_POINT ( 'NONE',  ( -22.42594789675818845, -19.77792426076253918, 69.45945937764655298 ) ) ;
#27843 = CARTESIAN_POINT ( 'NONE',  ( -10.74573065459234478, -12.54952415110468422, 60.81325645027152405 ) ) ;
#27844 = ORIENTED_EDGE ( 'NONE', *, *, #6275, .F. ) ;
#27845 = CARTESIAN_POINT ( 'NONE',  ( -22.79734292848665334, -10.24514101169484448, 66.84182257473258915 ) ) ;
#27846 = ADVANCED_FACE ( 'NONE', ( #44306 ), #47267, .T. ) ;
#27847 = CARTESIAN_POINT ( 'NONE',  ( -19.31122959855452237, -8.013358182787271744, 63.84578077065769719 ) ) ;
#27848 = CARTESIAN_POINT ( 'NONE',  ( -12.17647495751581133, -14.96730746957505254, 49.52966884056655772 ) ) ;
#27849 = CARTESIAN_POINT ( 'NONE',  ( -22.84886471163500588, -9.702775354051940582, 73.59665661135821324 ) ) ;
#27850 = CARTESIAN_POINT ( 'NONE',  ( -21.37496138168859972, -9.030742569741930126, 70.32235629077148076 ) ) ;
#27851 =( BOUNDED_CURVE ( )  B_SPLINE_CURVE ( 3, ( #1534, #20251, #42432, #46115 ),
 .UNSPECIFIED., .F., .F. ) 
 B_SPLINE_CURVE_WITH_KNOTS ( ( 4, 4 ),
 ( 0.000000000000000000, 0.4074455897393636228 ),
 .UNSPECIFIED. ) 
 CURVE ( )  GEOMETRIC_REPRESENTATION_ITEM ( )  RATIONAL_B_SPLINE_CURVE ( ( 1.000000000000000000, 0.4567392136813317460, 0.3561768502900302114, 0.6983129098260953960 ) ) 
 REPRESENTATION_ITEM ( '' )  );
#27852 = ORIENTED_EDGE ( 'NONE', *, *, #23191, .T. ) ;
#27853 = ORIENTED_EDGE ( 'NONE', *, *, #1831, .T. ) ;
#27854 = CIRCLE ( 'NONE', #25489, 4.686499999999998778 ) ;
#27855 = ORIENTED_EDGE ( 'NONE', *, *, #22104, .T. ) ;
#27856 = CARTESIAN_POINT ( 'NONE',  ( -10.83683315258895519, -12.44108567723101899, 57.32857332099802505 ) ) ;
#27857 = CIRCLE ( 'NONE', #35713, 4.686499999999997002 ) ;
#27858 = EDGE_CURVE ( 'NONE', #44291, #20782, #46409, .T. ) ;
#27859 = CARTESIAN_POINT ( 'NONE',  ( -17.42409385541299471, -14.80920654474435594, 52.02966884056656482 ) ) ;
#27860 = ORIENTED_EDGE ( 'NONE', *, *, #47650, .F. ) ;
#27861 =( BOUNDED_CURVE ( )  B_SPLINE_CURVE ( 3, ( #27557, #4414, #46275, #1200 ),
 .UNSPECIFIED., .F., .F. ) 
 B_SPLINE_CURVE_WITH_KNOTS ( ( 4, 4 ),
 ( 0.9074455897393690629, 1.000000000000000000 ),
 .UNSPECIFIED. ) 
 CURVE ( )  GEOMETRIC_REPRESENTATION_ITEM ( )  RATIONAL_B_SPLINE_CURVE ( ( 0.6983129098261063872, 0.7760317562607097486, 0.8765941196520076195, 1.000000000000000000 ) ) 
 REPRESENTATION_ITEM ( '' )  );
#27862 = CARTESIAN_POINT ( 'NONE',  ( -10.83518795442179972, -11.33195075051574108, 67.78011127842214023 ) ) ;
#27863 = CARTESIAN_POINT ( 'NONE',  ( -10.00761937521931522, -15.51608998476985946, 57.75288115419267854 ) ) ;
#27864 = VERTEX_POINT ( 'NONE', #10323 ) ;
#27865 = CARTESIAN_POINT ( 'NONE',  ( -10.60570718526854961, -17.81143598018131158, 71.68222757358374508 ) ) ;
#27866 = CARTESIAN_POINT ( 'NONE',  ( -23.80698208075059341, -17.68407496960266201, 62.48977578363538044 ) ) ;
#27867 = EDGE_LOOP ( 'NONE', ( #15915, #41013, #42108, #17863 ) ) ;
#27868 = CARTESIAN_POINT ( 'NONE',  ( -19.97013658168673800, -21.81073013994861398, 68.97836559665680056 ) ) ;
#27869 = VERTEX_POINT ( 'NONE', #18169 ) ;
#27870 = CARTESIAN_POINT ( 'NONE',  ( -22.11774618123879677, -15.02177039319221130, 52.02966884056656482 ) ) ;
#27871 = ORIENTED_EDGE ( 'NONE', *, *, #42837, .T. ) ;
#27872 = FACE_OUTER_BOUND ( 'NONE', #22226, .T. ) ;
#27873 = CARTESIAN_POINT ( 'NONE',  ( -16.78341102624552050, -22.23169286577646986, 68.88055947109249644 ) ) ;
#27874 = CARTESIAN_POINT ( 'NONE',  ( -19.30861700655685098, -22.01699669475148724, 58.78153328179137560 ) ) ;
#27875 = ORIENTED_EDGE ( 'NONE', *, *, #1093, .T. ) ;
#27876 = CARTESIAN_POINT ( 'NONE',  ( -26.42409385541305511, -15.80920654474410725, 48.99999999999997868 ) ) ;
#27877 = ADVANCED_FACE ( 'NONE', ( #40117 ), #21639, .T. ) ;
#27878 = EDGE_CURVE ( 'NONE', #22320, #34081, #20925, .T. ) ;
#27879 = CARTESIAN_POINT ( 'NONE',  ( -21.34581862946232889, -20.66775363590295100, 72.52446429492309221 ) ) ;
#27880 = CARTESIAN_POINT ( 'NONE',  ( -17.85903083518457635, -21.79574121735856451, 58.47841500721298047 ) ) ;
#27881 = CARTESIAN_POINT ( 'NONE',  ( -24.45422819554991278, -14.24171526414585287, 66.06804100909725719 ) ) ;
#27882 = CARTESIAN_POINT ( 'NONE',  ( -10.47299139157196990, -15.63514485490427575, 61.03789045487297926 ) ) ;
#27883 = CARTESIAN_POINT ( 'NONE',  ( -20.57444551192666538, -21.06071957749239232, 58.66091790465502953 ) ) ;
#27884 = ORIENTED_EDGE ( 'NONE', *, *, #11323, .F. ) ;
#27885 = DIRECTION ( 'NONE',  ( 0.000000000000000000, 0.000000000000000000, 1.000000000000000000 ) ) ;
#27886 = FACE_OUTER_BOUND ( 'NONE', #22511, .T. ) ;
#27887 = CARTESIAN_POINT ( 'NONE',  ( -16.18369095565973836, -7.463183609464278057, 60.30004841332083743 ) ) ;
#27888 = CIRCLE ( 'NONE', #27117, 1.999999999999999556 ) ;
#27889 = ADVANCED_FACE ( 'NONE', ( #11780 ), #3648, .T. ) ;
#27890 = EDGE_CURVE ( 'NONE', #16629, #37435, #38101, .T. ) ;
#27891 = CARTESIAN_POINT ( 'NONE',  ( -24.87384330133638599, -14.87999890626018384, 59.35804801245023299 ) ) ;
#27892 = CARTESIAN_POINT ( 'NONE',  ( -17.77409385759798965, -6.859212275519751323, 50.50378509014259265 ) ) ;
#27893 = CARTESIAN_POINT ( 'NONE',  ( -15.32409385650551670, -6.426201560718813433, 50.50509628382439331 ) ) ;
#27895 = EDGE_CURVE ( 'NONE', #18577, #9916, #9158, .T. ) ;
#27894 = VERTEX_POINT ( 'NONE', #37363 ) ;
#27896 = FACE_OUTER_BOUND ( 'NONE', #13385, .T. ) ;
#27897 = CARTESIAN_POINT ( 'NONE',  ( -18.72681101482838173, -7.880611649715417499, 70.37068030201731972 ) ) ;
#27898 = VERTEX_POINT ( 'NONE', #22133 ) ;
#27899 = CARTESIAN_POINT ( 'NONE',  ( -4.424093855413053333, -27.10920654474410796, 63.99999999999998579 ) ) ;
#27900 = CARTESIAN_POINT ( 'NONE',  ( -10.53028993777715883, -16.28642212234895226, 71.73278239416407587 ) ) ;
#27901 = CARTESIAN_POINT ( 'NONE',  ( -23.08009853854674986, -9.960157477770804846, 66.58536326842445874 ) ) ;
#27902 = CARTESIAN_POINT ( 'NONE',  ( -22.88264614489240856, -10.34704276773305764, 63.35713876973677827 ) ) ;
#27903 = B_SPLINE_CURVE_WITH_KNOTS ( 'NONE', 3,
 ( #16487, #1227, #46057, #16232, #13265, #12317, #28322, #20923, #28061, #39143 ),
 .UNSPECIFIED., .F., .F.,
 ( 4, 2, 2, 2, 4 ),
 ( 0.000000000000000000, 0.2500000000000000000, 0.5000000000000000000, 0.7500000000000000000, 1.000000000000000000 ),
 .UNSPECIFIED. ) ;
#27904 = VERTEX_POINT ( 'NONE', #15437 ) ;
#27905 = CARTESIAN_POINT ( 'NONE',  ( -24.80084942886774257, -15.85139998926299398, 69.63333248085599791 ) ) ;
#27906 = DIRECTION ( 'NONE',  ( -0.000000000000000000, -1.000000000000000000, 0.000000000000000000 ) ) ;
#27907 = CARTESIAN_POINT ( 'NONE',  ( -11.96084906401204506, -9.743958800322932490, 60.74413413563605957 ) ) ;
#27908 = EDGE_CURVE ( 'NONE', #15441, #1628, #9473, .T. ) ;
#27909 = ORIENTED_EDGE ( 'NONE', *, *, #43522, .T. ) ;
#27910 = CARTESIAN_POINT ( 'NONE',  ( -17.08147026401541524, -7.366339275741904835, 70.60380589010705421 ) ) ;
#27911 = CARTESIAN_POINT ( 'NONE',  ( -10.43031943402893269, -12.24169207515381785, 57.46823944168010456 ) ) ;
#27912 = B_SPLINE_CURVE_WITH_KNOTS ( 'NONE', 1,
 ( #34734, #34967 ),
 .UNSPECIFIED., .F., .F.,
 ( 2, 2 ),
 ( 0.000000000000000000, 1.000000000000000000 ),
 .UNSPECIFIED. ) ;
#27913 = CARTESIAN_POINT ( 'NONE',  ( -16.70534385759799534, -7.595227055684746986, 51.75156210489594599 ) ) ;
#27914 = CARTESIAN_POINT ( 'NONE',  ( -50.42609385541305755, -14.80920654474427600, 73.09411764705880898 ) ) ;
#27915 = ORIENTED_EDGE ( 'NONE', *, *, #8810, .T. ) ;
#27916 = EDGE_LOOP ( 'NONE', ( #23373, #33754, #3439 ) ) ;
#27917 = CARTESIAN_POINT ( 'NONE',  ( -21.68034385541304587, -9.360768649639302552, 51.01397948905921709 ) ) ;
#27918 = B_SPLINE_CURVE_WITH_KNOTS ( 'NONE', 1,
 ( #37957, #17237 ),
 .UNSPECIFIED., .F., .F.,
 ( 2, 2 ),
 ( 0.000000000000000000, 1.000000000000000000 ),
 .UNSPECIFIED. ) ;
#27919 = CARTESIAN_POINT ( 'NONE',  ( -15.55648817577099585, -8.010769314271311003, 74.09457776258329886 ) ) ;
#27920 = CARTESIAN_POINT ( 'NONE',  ( -24.87401146225354864, -14.84424530793535624, 59.39300237368605906 ) ) ;
#27921 = VECTOR ( 'NONE', #4595, 1000.000000000000114 ) ;
#27922 = CARTESIAN_POINT ( 'NONE',  ( -42.55865267894247239, -14.80920654474414810, 61.92352941176469727 ) ) ;
#27923 = CARTESIAN_POINT ( 'NONE',  ( -12.27729925481933471, -9.991218852276041673, 60.55918086709623083 ) ) ;
#27924 = VECTOR ( 'NONE', #18425, 1000.000000000000114 ) ;
#27925 = LINE ( 'NONE', #43203, #19414 ) ;
#27926 = EDGE_CURVE ( 'NONE', #28111, #17101, #14689, .T. ) ;
#27927 = ORIENTED_EDGE ( 'NONE', *, *, #2242, .F. ) ;
#27928 = CARTESIAN_POINT ( 'NONE',  ( -40.92409385541305511, -14.80920654474410725, 74.99999999999998579 ) ) ;
#27929 = DIRECTION ( 'NONE',  ( -3.071710424422018668E-17, 6.404604876783312462E-16, 1.000000000000000000 ) ) ;
#27930 = ORIENTED_EDGE ( 'NONE', *, *, #43510, .F. ) ;
#27931 = CARTESIAN_POINT ( 'NONE',  ( -10.29245896349820200, -16.96639176515380854, 57.87415878384224044 ) ) ;
#27932 = CARTESIAN_POINT ( 'NONE',  ( -18.52415950777489684, -7.896185818571675341, 74.14064402152244782 ) ) ;
#27933 = ORIENTED_EDGE ( 'NONE', *, *, #43497, .T. ) ;
#27934 = CARTESIAN_POINT ( 'NONE',  ( 18.57590614458706924, 1.890747609047612077, 50.53028072113853142 ) ) ;
#27935 = EDGE_CURVE ( 'NONE', #16774, #8094, #11042, .T. ) ;
#27936 = CARTESIAN_POINT ( 'NONE',  ( -10.00551284293887910, -15.49280627557078382, 57.66769182383846726 ) ) ;
#27937 = FACE_OUTER_BOUND ( 'NONE', #35552, .T. ) ;
#27938 = FACE_OUTER_BOUND ( 'NONE', #5118, .T. ) ;
#27939 = ORIENTED_EDGE ( 'NONE', *, *, #6730, .T. ) ;
#27940 = CARTESIAN_POINT ( 'NONE',  ( -18.57335281209669375, -21.76520412651811043, 72.57038810541313012 ) ) ;
#27941 = CARTESIAN_POINT ( 'NONE',  ( -30.42409385541305156, -6.359206544744109735, 52.99999999999997158 ) ) ;
#27942 = CARTESIAN_POINT ( 'NONE',  ( -36.42409385541304800, -9.359200813967566646, 50.49621490985803263 ) ) ;
#27943 = CARTESIAN_POINT ( 'NONE',  ( -21.14127837747716043, -20.79979359094293656, 69.06010003804692587 ) ) ;
#27944 = EDGE_CURVE ( 'NONE', #45965, #24590, #33666, .T. ) ;
#27945 = CARTESIAN_POINT ( 'NONE',  ( -24.87417962317557496, -14.80849170857717567, 59.42795673386487465 ) ) ;
#27946 = CARTESIAN_POINT ( 'NONE',  ( -23.34452670104532146, -10.97471634670236718, 73.36193064516098161 ) ) ;
#27947 = EDGE_CURVE ( 'NONE', #36933, #25852, #46749, .T. ) ;
#27948 = CARTESIAN_POINT ( 'NONE',  ( -14.72778340125292829, -21.32322296975913645, 58.46617885012764049 ) ) ;
#27949 = ORIENTED_EDGE ( 'NONE', *, *, #47664, .T. ) ;
#27950 = CARTESIAN_POINT ( 'NONE',  ( -12.15107414628315574, -10.20293217168262245, 67.68823922474383892 ) ) ;
#27951 = ADVANCED_FACE ( 'NONE', ( #458 ), #7365, .T. ) ;
#27952 = CARTESIAN_POINT ( 'NONE',  ( -12.23358631666068241, -10.11189219506639247, 64.31297738809925590 ) ) ;
#27953 = FACE_OUTER_BOUND ( 'NONE', #42267, .T. ) ;
#27954 = ORIENTED_EDGE ( 'NONE', *, *, #8083, .T. ) ;
#27955 = DIRECTION ( 'NONE',  ( -0.4439273849576907960, -0.8960627639203775363, -1.004702157338010031E-17 ) ) ;
#27956 = VECTOR ( 'NONE', #4069, 1000.000000000000000 ) ;
#27957 = CARTESIAN_POINT ( 'NONE',  ( -20.31413516131974717, -8.378470924821744603, 67.06632013881642251 ) ) ;
#27958 = ORIENTED_EDGE ( 'NONE', *, *, #17755, .T. ) ;
#27959 = ORIENTED_EDGE ( 'NONE', *, *, #22499, .T. ) ;
#27960 = EDGE_LOOP ( 'NONE', ( #24193, #1163 ) ) ;
#27961 = CARTESIAN_POINT ( 'NONE',  ( -17.42409385541299471, -14.80920654474435771, 49.52966884056655772 ) ) ;
#27963 = EDGE_CURVE ( 'NONE', #19332, #43983, #36764, .T. ) ;
#27962 = CARTESIAN_POINT ( 'NONE',  ( -12.86614516408948283, -8.916182316271401120, 67.57931555780623967 ) ) ;
#27964 = DIRECTION ( 'NONE',  ( 0.9687793358424819923, -0.2479245821708680464, 0.000000000000000000 ) ) ;
#27965 = CARTESIAN_POINT ( 'NONE',  ( -15.07409385759798859, -6.859212275519751323, 50.50378509014259265 ) ) ;
#27966 = CARTESIAN_POINT ( 'NONE',  ( -10.71275572639902940, -16.80316056253202817, 57.91590435120537705 ) ) ;
#27967 = ORIENTED_EDGE ( 'NONE', *, *, #4935, .T. ) ;
#27968 = EDGE_LOOP ( 'NONE', ( #47641, #34614, #45771, #46921, #9979 ) ) ;
#27969 = CARTESIAN_POINT ( 'NONE',  ( -21.09284385650551741, -7.406986770994973490, 48.81910596585309747 ) ) ;
#27970 = PRODUCT_RELATED_PRODUCT_CATEGORY ( 'part', '', ( #33845 ) ) ;
#27971 = CARTESIAN_POINT ( 'NONE',  ( -22.09234551867295693, -20.09219114410425178, 62.53439162497838311 ) ) ;
#27972 = CARTESIAN_POINT ( 'NONE',  ( -17.42409385541299471, -14.80920654474435771, 49.52966884056655772 ) ) ;
#27973 = DIRECTION ( 'NONE',  ( -0.1186632576870824130, 0.9929345553837299887, 6.051931679537041823E-08 ) ) ;
#27974 = CARTESIAN_POINT ( 'NONE',  ( -21.31784385650551883, -9.790100578890868377, 49.79778022625163203 ) ) ;
#27975 = ORIENTED_EDGE ( 'NONE', *, *, #40438, .F. ) ;
#27976 = DIRECTION ( 'NONE',  ( 1.205044182495138397E-05, 2.694341358818416019E-06, 0.9999999999237635384 ) ) ;
#27977 = LINE ( 'NONE', #31683, #34722 ) ;
#27978 = CYLINDRICAL_SURFACE ( 'NONE', #40952, 0.4000000000000006883 ) ;
#27979 =( BOUNDED_SURFACE ( )  B_SPLINE_SURFACE ( 3, 1, ( 
 ( #1632, #24299 ),
 ( #1379, #39303 ),
 ( #32163, #31916 ),
 ( #39781, #35832 ),
 ( #13425, #46932 ),
 ( #6047, #17113 ),
 ( #28475, #43498 ) ),
 .UNSPECIFIED., .T., .F., .F. ) 
 B_SPLINE_SURFACE_WITH_KNOTS ( ( 4, 3, 4 ),
 ( 2, 2 ),
 ( 0.000000000000000000, 0.5000000000000000000, 1.000000000000000000 ),
 ( 0.000000000000000000, 1.000000000000000000 ),
 .UNSPECIFIED. ) 
 GEOMETRIC_REPRESENTATION_ITEM ( )  RATIONAL_B_SPLINE_SURFACE ( (
 ( 1.000000000000000000, 1.000000000000000000),
 ( 0.3333333333333335369, 0.3333333333333330373),
 ( 0.3333333333333335369, 0.3333333333333330373),
 ( 1.000000000000000000, 1.000000000000000000),
 ( 0.3333333333333333703, 0.3333333333333333703),
 ( 0.3333333333333333703, 0.3333333333333333703),
 ( 1.000000000000000000, 1.000000000000000000) ) ) 
 REPRESENTATION_ITEM ( '' )  SURFACE ( )  );
#27980 = EDGE_CURVE ( 'NONE', #20878, #1905, #26783, .T. ) ;
#27981 = ORIENTED_EDGE ( 'NONE', *, *, #23191, .F. ) ;
#27982 = CARTESIAN_POINT ( 'NONE',  ( -12.82409385759799036, -9.359200813967568422, 50.49621490985803263 ) ) ;
#27983 = VECTOR ( 'NONE', #13607, 1000.000000000000227 ) ;
#27984 = CARTESIAN_POINT ( 'NONE',  ( -10.37599212182869124, -14.63324797960940771, 71.34254748307667171 ) ) ;
#27985 = CARTESIAN_POINT ( 'NONE',  ( -41.15852941833841783, -27.10920654474410796, 56.99999999999997868 ) ) ;
#27986 = CARTESIAN_POINT ( 'NONE',  ( -22.53655392111809164, -20.22829597721307948, 65.88917050827579658 ) ) ;
#27987 = ORIENTED_EDGE ( 'NONE', *, *, #20947, .F. ) ;
#27988 = DIRECTION ( 'NONE',  ( 2.866981220435666553E-17, -1.000000000000000000, -1.190614954331866791E-16 ) ) ;
#27989 = CARTESIAN_POINT ( 'NONE',  ( -24.45577199812615632, -12.20047074031916168, 53.49999999999994316 ) ) ;
#27990 = CARTESIAN_POINT ( 'NONE',  ( -20.11579277122780596, -7.862326722158320180, 73.89813526064125426 ) ) ;
#27991 = ORIENTED_EDGE ( 'NONE', *, *, #35831, .T. ) ;
#27992 = CARTESIAN_POINT ( 'NONE',  ( -17.13503149044196761, -7.764836982087094164, 70.77563787455143540 ) ) ;
#27993 =( BOUNDED_CURVE ( )  B_SPLINE_CURVE ( 3, ( #29096, #44153, #10401, #6695 ),
 .UNSPECIFIED., .F., .F. ) 
 B_SPLINE_CURVE_WITH_KNOTS ( ( 4, 4 ),
 ( 0.9074455897393649551, 1.000000000000000000 ),
 .UNSPECIFIED. ) 
 CURVE ( )  GEOMETRIC_REPRESENTATION_ITEM ( )  RATIONAL_B_SPLINE_CURVE ( ( 0.6983129098261113832, 0.7760317562607140784, 0.8765941196520102840, 1.000000000000000000 ) ) 
 REPRESENTATION_ITEM ( '' )  );
#27994 = VERTEX_POINT ( 'NONE', #9297 ) ;
#27995 = CARTESIAN_POINT ( 'NONE',  ( -23.42915847708036736, -11.11517115755410146, 73.64721174900437006 ) ) ;
#27996 = CYLINDRICAL_SURFACE ( 'NONE', #24101, 0.1500000000000061007 ) ;
#27997 = ORIENTED_EDGE ( 'NONE', *, *, #39444, .F. ) ;
#27998 = LINE ( 'NONE', #20134, #36023 ) ;
#27999 = CARTESIAN_POINT ( 'NONE',  ( -19.98813040044048606, -21.37641421727040125, 72.40478737316021807 ) ) ;
#28000 = CARTESIAN_POINT ( 'NONE',  ( -17.58103735145357760, -12.18847542802175532, 53.87877519908923318 ) ) ;
#28001 = B_SPLINE_CURVE_WITH_KNOTS ( 'NONE', 3,
 ( #35680, #28561, #43590, #42854, #1475, #1733, #16490, #27825, #42624, #43347 ),
 .UNSPECIFIED., .F., .F.,
 ( 4, 2, 2, 2, 4 ),
 ( 0.000000000000000000, 0.2500000000000000000, 0.5000000000000000000, 0.7500000000000000000, 1.000000000000000000 ),
 .UNSPECIFIED. ) ;
#28002 = ADVANCED_FACE ( 'NONE', ( #30979 ), #35380, .T. ) ;
#28003 = CARTESIAN_POINT ( 'NONE',  ( -21.51080377022508472, -17.10312989180209087, 49.52966884056655772 ) ) ;
#28004 = ORIENTED_EDGE ( 'NONE', *, *, #18650, .F. ) ;
#28005 = CARTESIAN_POINT ( 'NONE',  ( -9.993919958658839420, -14.26595478062693800, 64.58815064441371590 ) ) ;
#28006 = ADVANCED_FACE ( 'NONE', ( #31698 ), #46723, .T. ) ;
#28007 = CARTESIAN_POINT ( 'NONE',  ( -23.99022880263543200, -10.64948376341961378, 54.30803469517864102 ) ) ;
#28008 = CARTESIAN_POINT ( 'NONE',  ( -22.25881579015244682, -9.141043659704909174, 59.92182412794203117 ) ) ;
#28009 = ORIENTED_EDGE ( 'NONE', *, *, #22650, .T. ) ;
#28010 = CARTESIAN_POINT ( 'NONE',  ( -15.54840433177174397, -8.005034934413657766, 67.29574103338339341 ) ) ;
#28011 =( BOUNDED_CURVE ( )  B_SPLINE_CURVE ( 3, ( #46158, #19825, #23519, #12899 ),
 .UNSPECIFIED., .F., .F. ) 
 B_SPLINE_CURVE_WITH_KNOTS ( ( 4, 4 ),
 ( 0.5000000000000000000, 0.9074455897393680637 ),
 .UNSPECIFIED. ) 
 CURVE ( )  GEOMETRIC_REPRESENTATION_ITEM ( )  RATIONAL_B_SPLINE_CURVE ( ( 0.9999999999999972244, 0.4567392136813289705, 0.3561768502900310440, 0.6983129098261003920 ) ) 
 REPRESENTATION_ITEM ( '' )  );
#28012 = EDGE_CURVE ( 'NONE', #3121, #14597, #35618, .T. ) ;
#28013 = CARTESIAN_POINT ( 'NONE',  ( -24.73928442521073023, -16.22033272921623848, 62.78602803661277676 ) ) ;
#28014 = VERTEX_POINT ( 'NONE', #35136 ) ;
#28015 = VERTEX_POINT ( 'NONE', #937 ) ;
#28016 = CARTESIAN_POINT ( 'NONE',  ( -14.87212829970780703, -21.32751220717084806, 58.23906021010879641 ) ) ;
#28017 = CARTESIAN_POINT ( 'NONE',  ( -10.92563986671175691, -18.45389586190763964, 57.99369949602996854 ) ) ;
#28018 = CARTESIAN_POINT ( 'NONE',  ( -19.71159385650551599, -6.922745924619793101, 51.69366785382590024 ) ) ;
#28019 = DIRECTION ( 'NONE',  ( 0.000000000000000000, 1.000000000000000000, -0.000000000000000000 ) ) ;
#28020 = EDGE_CURVE ( 'NONE', #18062, #20335, #12495, .T. ) ;
#28021 = CARTESIAN_POINT ( 'NONE',  ( -12.37144311045842038, -19.65386551827485917, 58.03568442835949526 ) ) ;
#28022 = B_SPLINE_CURVE_WITH_KNOTS ( 'NONE', 1,
 ( #12708, #41789 ),
 .UNSPECIFIED., .F., .F.,
 ( 2, 2 ),
 ( 0.000000000000000000, 1.000000000000000000 ),
 .UNSPECIFIED. ) ;
#28023 = CARTESIAN_POINT ( 'NONE',  ( -13.88293259567353566, -20.90532631576516209, 68.45625136994867432 ) ) ;
#28024 = EDGE_CURVE ( 'NONE', #205, #12901, #27274, .T. ) ;
#28025 = CARTESIAN_POINT ( 'NONE',  ( -23.29918407416772297, -19.39037376486758646, 58.99915347576865088 ) ) ;
#28026 = AXIS2_PLACEMENT_3D ( 'NONE', #28353, #43616, #2233 ) ;
#28027 = ORIENTED_EDGE ( 'NONE', *, *, #26815, .F. ) ;
#28028 = ORIENTED_EDGE ( 'NONE', *, *, #22871, .F. ) ;
#28029 = CARTESIAN_POINT ( 'NONE',  ( -11.13352401182878459, -11.60862911821036292, 74.70272630447266238 ) ) ;
#28030 = B_SPLINE_CURVE_WITH_KNOTS ( 'NONE', 3,
 ( #20010, #16289, #5001, #34783, #46359, #8934, #45879, #26920, #15561, #1279 ),
 .UNSPECIFIED., .F., .F.,
 ( 4, 2, 2, 2, 4 ),
 ( 0.6272669072782502964, 0.7522669073001506668, 0.8772669073220509262, 1.002266907343951186, 1.127266907365851667 ),
 .UNSPECIFIED. ) ;
#28031 = CARTESIAN_POINT ( 'NONE',  ( -24.72409385541305582, -14.80920654474424225, 70.07647058823528141 ) ) ;
#28032 = CARTESIAN_POINT ( 'NONE',  ( -19.63995608841934626, -21.92282860479379991, 65.65141533869274326 ) ) ;
#28033 = CARTESIAN_POINT ( 'NONE',  ( -22.37742504188432235, -19.75764164967408831, 72.83327514797355207 ) ) ;
#28034 = CYLINDRICAL_SURFACE ( 'NONE', #37814, 1.999999999999999556 ) ;
#28035 = ORIENTED_EDGE ( 'NONE', *, *, #18402, .T. ) ;
#28036 = DIRECTION ( 'NONE',  ( 0.9687793358424821033, -0.2479245821708677133, 0.000000000000000000 ) ) ;
#28037 = CARTESIAN_POINT ( 'NONE',  ( -24.01628879148212548, -11.33852128837717999, 66.52240266552541925 ) ) ;
#28038 = CYLINDRICAL_SURFACE ( 'NONE', #13459, 0.1500000000000008549 ) ;
#28039 = CARTESIAN_POINT ( 'NONE',  ( -13.63659385541286717, -8.995762431863431274, 51.38120296130607301 ) ) ;
#28040 = ADVANCED_FACE ( 'NONE', ( #12021 ), #3276, .T. ) ;
#28041 = ORIENTED_EDGE ( 'NONE', *, *, #22728, .F. ) ;
#28042 = CARTESIAN_POINT ( 'NONE',  ( -10.12821362422299210, -13.30163807797161546, 74.87806422314912425 ) ) ;
#28043 = FACE_OUTER_BOUND ( 'NONE', #6865, .T. ) ;
#28044 = CARTESIAN_POINT ( 'NONE',  ( -17.77594409791816688, -7.367433943401969998, 60.26556080592736464 ) ) ;
#28045 = CARTESIAN_POINT ( 'NONE',  ( -18.60148803548772278, -7.908491065787107033, 73.85681094374102429 ) ) ;
#28046 = CARTESIAN_POINT ( 'NONE',  ( -11.57017261513264117, -10.87519553945718620, 57.62392099249677102 ) ) ;
#28047 = CARTESIAN_POINT ( 'NONE',  ( -11.10300703817161327, -10.86615712478015539, 57.39398594787093089 ) ) ;
#28048 = ORIENTED_EDGE ( 'NONE', *, *, #4235, .F. ) ;
#28049 = EDGE_CURVE ( 'NONE', #35496, #2258, #15586, .T. ) ;
#28050 = CARTESIAN_POINT ( 'NONE',  ( -19.04853579327176760, -7.948602568230340282, 63.71617106789811658 ) ) ;
#28051 = AXIS2_PLACEMENT_3D ( 'NONE', #45066, #7633, #26327 ) ;
#28052 = CIRCLE ( 'NONE', #35152, 2.404255319148937531 ) ;
#28053 = ORIENTED_EDGE ( 'NONE', *, *, #22106, .T. ) ;
#28054 = CARTESIAN_POINT ( 'NONE',  ( -10.01188548097954012, -14.05969102102910284, 61.11832497397694652 ) ) ;
#28055 = FACE_OUTER_BOUND ( 'NONE', #23620, .T. ) ;
#28056 = VERTEX_POINT ( 'NONE', #39324 ) ;
#28057 = CARTESIAN_POINT ( 'NONE',  ( -18.37786432726835883, -21.79469297182707521, 69.10042588711679912 ) ) ;
#28058 = CARTESIAN_POINT ( 'NONE',  ( -13.05029276218966672, -20.34859559109395377, 71.96220867596423432 ) ) ;
#28059 = B_SPLINE_CURVE_WITH_KNOTS ( 'NONE', 3,
 ( #7479, #3511, #25679, #33051, #18525, #11394, #48325, #48094, #14560, #29876 ),
 .UNSPECIFIED., .F., .F.,
 ( 4, 2, 2, 2, 4 ),
 ( 0.1272669073658321826, 0.2522669073463198464, 0.3772669073268074547, 0.5022669073072951740, 0.6272669072877827823 ),
 .UNSPECIFIED. ) ;
#28060 = EDGE_LOOP ( 'NONE', ( #17200, #34119, #9075, #11988, #18879 ) ) ;
#28061 = CARTESIAN_POINT ( 'NONE',  ( -11.95536650667902911, -10.43947391085179710, 71.26893134408621222 ) ) ;
#28062 = VECTOR ( 'NONE', #6554, 1000.000000000000227 ) ;
#28063 = DIRECTION ( 'NONE',  ( -3.071710424422018668E-17, 6.404604876783312462E-16, 1.000000000000000000 ) ) ;
#28064 = ORIENTED_EDGE ( 'NONE', *, *, #17372, .T. ) ;
#28065 = DIRECTION ( 'NONE',  ( -3.071710424422018668E-17, 6.404604876783312462E-16, 1.000000000000000000 ) ) ;
#28066 = CARTESIAN_POINT ( 'NONE',  ( -10.47425521701617157, -17.49314416303823450, 64.81234701634230078 ) ) ;
#28067 = EDGE_CURVE ( 'NONE', #37829, #19273, #12741, .T. ) ;
#28068 = CARTESIAN_POINT ( 'NONE',  ( -12.82020749880560651, -17.33244462614775827, 52.02966884056656482 ) ) ;
#28069 = CARTESIAN_POINT ( 'NONE',  ( -24.76682342852691221, -16.06919080767510621, 66.25663251748672167 ) ) ;
#28070 = ORIENTED_EDGE ( 'NONE', *, *, #27484, .F. ) ;
#28071 = ORIENTED_EDGE ( 'NONE', *, *, #5468, .F. ) ;
#28072 = ADVANCED_FACE ( 'NONE', ( #27757 ), #23838, .T. ) ;
#28073 = CARTESIAN_POINT ( 'NONE',  ( -23.77708670646326539, -18.70057811943135206, 72.87094101505380195 ) ) ;
#28074 = DIRECTION ( 'NONE',  ( 4.436160459547892897E-06, 7.761523768847967188E-06, -0.9999999999600396317 ) ) ;
#28075 = ORIENTED_EDGE ( 'NONE', *, *, #5890, .F. ) ;
#28076 = DIRECTION ( 'NONE',  ( 0.9687793358424822143, -0.2479245821708672415, 0.000000000000000000 ) ) ;
#28077 = DIRECTION ( 'NONE',  ( -2.866981220435666553E-17, 1.000000000000000000, 1.190614954331866791E-16 ) ) ;
#28078 = ADVANCED_FACE ( 'NONE', ( #16168 ), #8330, .T. ) ;
#28079 = CARTESIAN_POINT ( 'NONE',  ( -20.13659385759799036, -8.995762431863214559, 51.38120296130585274 ) ) ;
#28080 = CARTESIAN_POINT ( 'NONE',  ( -10.42752915138136238, -15.03043058157462042, 75.02452189207510003 ) ) ;
#28081 = CARTESIAN_POINT ( 'NONE',  ( -19.78614017500849087, -21.39864787494504839, 68.93482476778672208 ) ) ;
#28082 = CARTESIAN_POINT ( 'NONE',  ( -15.84272952059200712, -7.988518299429712144, 70.79917007911708993 ) ) ;
#28083 = ORIENTED_EDGE ( 'NONE', *, *, #44027, .F. ) ;
#28084 = DIRECTION ( 'NONE',  ( 0.4461977533475101065, 0.8949343913984054710, -2.476895096512112418E-17 ) ) ;
#28085 = CARTESIAN_POINT ( 'NONE',  ( -19.04853579327176760, -7.948602568230340282, 63.71617106789811658 ) ) ;
#28086 = CARTESIAN_POINT ( 'NONE',  ( -12.29360062986345525, -9.973804982380832129, 60.55918084114097866 ) ) ;
#28087 = CARTESIAN_POINT ( 'NONE',  ( -13.06825169942196752, -9.255684228991221119, 74.46356075877366720 ) ) ;
#28088 = CARTESIAN_POINT ( 'NONE',  ( -13.46392603942681276, -20.58285214721693634, 61.74476297758946686 ) ) ;
#28089 = EDGE_CURVE ( 'NONE', #2205, #19987, #8319, .T. ) ;
#28091 = ORIENTED_EDGE ( 'NONE', *, *, #27622, .F. ) ;
#28090 = EDGE_CURVE ( 'NONE', #33207, #36361, #33014, .T. ) ;
#28092 = AXIS2_PLACEMENT_3D ( 'NONE', #27961, #20592, #1130 ) ;
#28093 = EDGE_LOOP ( 'NONE', ( #39561, #17908, #32768, #12794, #42581 ) ) ;
#28094 = VECTOR ( 'NONE', #39620, 1000.000000000000227 ) ;
#28095 = B_SPLINE_CURVE_WITH_KNOTS ( 'NONE', 3,
 ( #2881, #44043, #3375, #37334, #37095, #14661, #28757, #14188, #3622, #40800 ),
 .UNSPECIFIED., .F., .F.,
 ( 4, 2, 2, 2, 4 ),
 ( 0.6272669072782597333, 0.7522669073001514439, 0.8772669073220431546, 1.002266907343934754, 1.127266907365826576 ),
 .UNSPECIFIED. ) ;
#28096 = ORIENTED_EDGE ( 'NONE', *, *, #34150, .F. ) ;
#28097 = ADVANCED_FACE ( 'NONE', ( #16897 ), #35854, .T. ) ;
#28098 = EDGE_CURVE ( 'NONE', #11365, #7957, #10895, .T. ) ;
#28099 = CARTESIAN_POINT ( 'NONE',  ( -24.87286266620955288, -14.66952948351439190, 62.96942391020206742 ) ) ;
#28100 = CARTESIAN_POINT ( 'NONE',  ( -18.94388778215946445, -7.924927710426770133, 66.90071813243744714 ) ) ;
#28101 = CARTESIAN_POINT ( 'NONE',  ( -21.80947544975385810, -9.353161466788067813, 63.19153755920122251 ) ) ;
#28102 = VECTOR ( 'NONE', #22, 999.9999999999998863 ) ;
#28103 = ORIENTED_EDGE ( 'NONE', *, *, #48459, .T. ) ;
#28104 = CARTESIAN_POINT ( 'NONE',  ( -21.95217610637629946, -9.395202297576263462, 66.80583047767832738 ) ) ;
#28105 = CARTESIAN_POINT ( 'NONE',  ( -12.54253407177667512, -19.82621502378690082, 65.16674886820000268 ) ) ;
#28106 = ORIENTED_EDGE ( 'NONE', *, *, #9613, .T. ) ;
#28107 = CARTESIAN_POINT ( 'NONE',  ( -19.30128557755455176, -21.60500301973953086, 58.81035253397666196 ) ) ;
#28108 = VERTEX_POINT ( 'NONE', #39566 ) ;
#28109 = CARTESIAN_POINT ( 'NONE',  ( -23.35504391816078495, -10.30071636613414832, 59.70179792000674723 ) ) ;
#28110 = B_SPLINE_CURVE_WITH_KNOTS ( 'NONE', 3,
 ( #41127, #45085, #11335, #268, #4199, #40877, #22921, #48501, #18457, #7162 ),
 .UNSPECIFIED., .F., .F.,
 ( 4, 2, 2, 2, 4 ),
 ( 0.000000000000000000, 0.2500000000000000000, 0.5000000000000000000, 0.7500000000000000000, 1.000000000000000000 ),
 .UNSPECIFIED. ) ;
#28111 = VERTEX_POINT ( 'NONE', #47204 ) ;
#28112 = CARTESIAN_POINT ( 'NONE',  ( -10.61357223164714902, -13.19155561173493219, 71.20828586568362084 ) ) ;
#28113 = ORIENTED_EDGE ( 'NONE', *, *, #37976, .T. ) ;
#28114 = DIRECTION ( 'NONE',  ( -1.066846703571655765E-06, 9.113387012630844478E-06, 0.9999999999579040066 ) ) ;
#28115 = CARTESIAN_POINT ( 'NONE',  ( -14.78754745127378634, -8.270772244812135909, 60.61996282000563241 ) ) ;
#28116 = DIRECTION ( 'NONE',  ( 1.078386539787844256E-05, -7.293043934967424929E-06, 0.9999999999152597852 ) ) ;
#28117 = EDGE_LOOP ( 'NONE', ( #10064, #48019, #4560, #13260, #35150, #18559, #22506, #30883, #38637, #24816 ) ) ;
#28118 = DIRECTION ( 'NONE',  ( 1.000000000000000000, -4.164305804376849172E-17, 1.614929280266638808E-16 ) ) ;
#28119 = EDGE_CURVE ( 'NONE', #19883, #12016, #21352, .T. ) ;
#28120 = CARTESIAN_POINT ( 'NONE',  ( -24.42310453963427008, -14.68514377117137570, 63.01296481370926017 ) ) ;
#28121 = APPLICATION_CONTEXT ( 'automotive_design' ) ;
#28122 = CARTESIAN_POINT ( 'NONE',  ( -17.72419722990865054, -21.80277058550420577, 58.40553378253839156 ) ) ;
#28123 = AXIS2_PLACEMENT_3D ( 'NONE', #41251, #44473, #14149 ) ;
#28124 =( BOUNDED_SURFACE ( )  B_SPLINE_SURFACE ( 3, 1, ( 
 ( #28275, #2162 ),
 ( #43303, #5145 ),
 ( #1434, #16447 ),
 ( #31482, #24597 ),
 ( #17163, #3372 ),
 ( #47953, #48188 ),
 ( #32909, #10292 ) ),
 .UNSPECIFIED., .T., .F., .F. ) 
 B_SPLINE_SURFACE_WITH_KNOTS ( ( 4, 3, 4 ),
 ( 2, 2 ),
 ( 0.000000000000000000, 0.5000000000000000000, 1.000000000000000000 ),
 ( 0.000000000000000000, 1.000000000000000000 ),
 .UNSPECIFIED. ) 
 GEOMETRIC_REPRESENTATION_ITEM ( )  RATIONAL_B_SPLINE_SURFACE ( (
 ( 1.000000000000000000, 1.000000000000000000),
 ( 0.3333333333333335369, 0.3333333333333330373),
 ( 0.3333333333333335369, 0.3333333333333330373),
 ( 1.000000000000000000, 1.000000000000000000),
 ( 0.3333333333333333703, 0.3333333333333333703),
 ( 0.3333333333333333703, 0.3333333333333333703),
 ( 1.000000000000000000, 1.000000000000000000) ) ) 
 REPRESENTATION_ITEM ( '' )  SURFACE ( )  );
#28125 = CARTESIAN_POINT ( 'NONE',  ( -13.74195172841370649, -8.854398236607520900, 57.19797722959653896 ) ) ;
#28126 = DIRECTION ( 'NONE',  ( -0.9687793358424822143, 0.2479245821708672415, 0.000000000000000000 ) ) ;
#28127 = CARTESIAN_POINT ( 'NONE',  ( -10.37818533259200748, -17.22973363664382873, 61.27247698181179913 ) ) ;
#28128 = ORIENTED_EDGE ( 'NONE', *, *, #15869, .F. ) ;
#28129 = CARTESIAN_POINT ( 'NONE',  ( -21.95523322170430092, -8.895446802377390938, 66.77654591769551473 ) ) ;
#28130 = CIRCLE ( 'NONE', #40740, 2.000000000000000444 ) ;
#28131 = VECTOR ( 'NONE', #21416, 1000.000000000000000 ) ;
#28132 = CYLINDRICAL_SURFACE ( 'NONE', #10864, 0.1499999999999994671 ) ;
#28133 = DIRECTION ( 'NONE',  ( -5.731567514496413899E-31, -1.020425574103664789E-16, -1.000000000000000000 ) ) ;
#28134 = CARTESIAN_POINT ( 'NONE',  ( -23.27284462870851911, -18.74605969774991010, 66.10917289053097079 ) ) ;
#28135 = CARTESIAN_POINT ( 'NONE',  ( -19.23866564181064831, -21.62168251543364050, 58.82507384655652771 ) ) ;
#28136 = CARTESIAN_POINT ( 'NONE',  ( -16.95534385650551812, -7.417179338643134834, 52.18511593390279302 ) ) ;
#28137 = ORIENTED_EDGE ( 'NONE', *, *, #23854, .T. ) ;
#28138 = EDGE_CURVE ( 'NONE', #38954, #17561, #34617, .T. ) ;
#28139 = CARTESIAN_POINT ( 'NONE',  ( -20.83411228044830210, -20.98307166581800587, 65.99942768993690834 ) ) ;
#28140 = LINE ( 'NONE', #5971, #7708 ) ;
#28141 = ORIENTED_EDGE ( 'NONE', *, *, #34037, .F. ) ;
#28142 = B_SPLINE_CURVE_WITH_KNOTS ( 'NONE', 3,
 ( #19005, #535, #19481, #45615, #3487, #3740, #18500, #33504, #48545, #29851 ),
 .UNSPECIFIED., .F., .F.,
 ( 4, 2, 2, 2, 4 ),
 ( 0.1272669073658269645, 0.2522669073463317813, 0.3772669073268366535, 0.5022669073073414703, 0.6272669072878462870 ),
 .UNSPECIFIED. ) ;
#28143 = DIRECTION ( 'NONE',  ( 0.6478992145799701285, -0.7617260713318518839, 1.927832152310587152E-08 ) ) ;
#28144 = FACE_OUTER_BOUND ( 'NONE', #9608, .T. ) ;
#28145 = CARTESIAN_POINT ( 'NONE',  ( -23.12431869989520550, -10.01221758024046338, 66.79828185159925624 ) ) ;
#28146 = AXIS2_PLACEMENT_3D ( 'NONE', #2507, #43888, #32312 ) ;
#28147 = CARTESIAN_POINT ( 'NONE',  ( -22.94085508618206859, -9.802298960702817254, 70.19673832247809742 ) ) ;
#28148 =( BOUNDED_CURVE ( )  B_SPLINE_CURVE ( 3, ( #40425, #47816, #48536, #3732 ),
 .UNSPECIFIED., .F., .F. ) 
 B_SPLINE_CURVE_WITH_KNOTS ( ( 4, 4 ),
 ( 0.5000000000000000000, 0.9074455897393666204 ),
 .UNSPECIFIED. ) 
 CURVE ( )  GEOMETRIC_REPRESENTATION_ITEM ( )  RATIONAL_B_SPLINE_CURVE ( ( 1.000000000000014655, 0.4567392136813281378, 0.3561768502900183875, 0.6983129098261015022 ) ) 
 REPRESENTATION_ITEM ( '' )  );
#28149 = EDGE_LOOP ( 'NONE', ( #11818, #46815, #37800, #38854, #21153 ) ) ;
#28150 = AXIS2_PLACEMENT_3D ( 'NONE', #21895, #3425, #36899 ) ;
#28151 = DIRECTION ( 'NONE',  ( 1.371992797150048625E-08, -1.272593384837864910E-06, 0.9999999999991900923 ) ) ;
#28152 = DIRECTION ( 'NONE',  ( 1.000000000000000000, 2.866981220435666553E-17, 0.000000000000000000 ) ) ;
#28153 = CARTESIAN_POINT ( 'NONE',  ( -14.87952233054990714, -7.807053693480528800, 57.01146488488941344 ) ) ;
#28154 = ORIENTED_EDGE ( 'NONE', *, *, #31379, .T. ) ;
#28155 = CARTESIAN_POINT ( 'NONE',  ( -11.31433821118811522, -10.42787716839952239, 53.76227901944321275 ) ) ;
#28156 = CARTESIAN_POINT ( 'NONE',  ( -24.41631212572655585, -17.38062150060373767, 69.60613961827247920 ) ) ;
#28157 = CARTESIAN_POINT ( 'NONE',  ( -19.92409385541305511, -14.80920654474410725, 79.00000000000000000 ) ) ;
#28158 = CARTESIAN_POINT ( 'NONE',  ( -24.10584592916820057, -12.56049825913868645, 73.24225570139947195 ) ) ;
#28159 = CARTESIAN_POINT ( 'NONE',  ( -10.71495554099518088, -12.81234323494808436, 64.56836111193433680 ) ) ;
#28160 =( BOUNDED_CURVE ( )  B_SPLINE_CURVE ( 3, ( #10319, #43330, #6615, #39618 ),
 .UNSPECIFIED., .F., .F. ) 
 B_SPLINE_CURVE_WITH_KNOTS ( ( 4, 4 ),
 ( 0.000000000000000000, 0.4074455897393627346 ),
 .UNSPECIFIED. ) 
 CURVE ( )  GEOMETRIC_REPRESENTATION_ITEM ( )  RATIONAL_B_SPLINE_CURVE ( ( 1.000000000000000000, 0.4567392136813397396, 0.3561768502900331534, 0.6983129098260801859 ) ) 
 REPRESENTATION_ITEM ( '' )  );
#28161 = VERTEX_POINT ( 'NONE', #5842 ) ;
#28162 = VERTEX_POINT ( 'NONE', #40298 ) ;
#28163 = CARTESIAN_POINT ( 'NONE',  ( -18.41784385541304303, -6.860780111191487229, 51.02154966934377001 ) ) ;
#28164 = ADVANCED_FACE ( 'NONE', ( #25281 ), #28493, .T. ) ;
#28165 = EDGE_CURVE ( 'NONE', #7346, #70, #13414, .T. ) ;
#28166 = CARTESIAN_POINT ( 'NONE',  ( -50.42409385541304800, -25.10920654474410441, 47.99999999999998579 ) ) ;
#28167 = VECTOR ( 'NONE', #47794, 1000.000000000000114 ) ;
#28168 = CYLINDRICAL_SURFACE ( 'NONE', #42605, 0.1500000000000050460 ) ;
#28169 = VECTOR ( 'NONE', #12819, 1000.000000000000000 ) ;
#28170 = AXIS2_PLACEMENT_3D ( 'NONE', #46182, #15886, #636 ) ;
#28171 = AXIS2_PLACEMENT_3D ( 'NONE', #36160, #28319, #25576 ) ;
#28172 = ADVANCED_FACE ( 'NONE', ( #29214 ), #10013, .T. ) ;
#28173 = ADVANCED_FACE ( 'NONE', ( #6072 ), #36098, .T. ) ;
#28174 = CARTESIAN_POINT ( 'NONE',  ( -24.44689184067228638, -14.18710713894228270, 69.93803194250308763 ) ) ;
#28175 = DIRECTION ( 'NONE',  ( -0.9950649908465211135, -0.09922531930717196080, 4.894557008102618136E-08 ) ) ;
#28176 = ORIENTED_EDGE ( 'NONE', *, *, #12366, .F. ) ;
#28177 = DIRECTION ( 'NONE',  ( -0.9974380310868018462, -0.07153582418399356824, 3.008056591778322057E-08 ) ) ;
#28178 = AXIS2_PLACEMENT_3D ( 'NONE', #23419, #16240, #42378 ) ;
#28179 = CARTESIAN_POINT ( 'NONE',  ( -24.23980054858686728, -17.81742536025289070, 62.66699277536263679 ) ) ;
#28180 = VERTEX_POINT ( 'NONE', #2853 ) ;
#28181 = CARTESIAN_POINT ( 'NONE',  ( -22.45050777529662511, -19.68108125846770307, 69.36521271289056756 ) ) ;
#28182 = CARTESIAN_POINT ( 'NONE',  ( -16.39156059917436181, -21.78318494029796781, 62.05568132351888266 ) ) ;
#28183 = ORIENTED_EDGE ( 'NONE', *, *, #34707, .F. ) ;
#28184 = DIRECTION ( 'NONE',  ( 1.224646799147353207E-16, 1.000000000000000000, -1.912410701131276611E-32 ) ) ;
#28185 = CARTESIAN_POINT ( 'NONE',  ( -11.42622260759249286, -18.51434353338492400, 61.57710833179551457 ) ) ;
#28186 = ORIENTED_EDGE ( 'NONE', *, *, #42578, .T. ) ;
#28187 = CARTESIAN_POINT ( 'NONE',  ( -17.70776945889202736, -22.25388964270624825, 58.52058054029878065 ) ) ;
#28188 = EDGE_CURVE ( 'NONE', #9986, #26867, #43171, .T. ) ;
#28189 = DIRECTION ( 'NONE',  ( 0.9687793358424819923, -0.2479245821708678243, 0.000000000000000000 ) ) ;
#28190 = CARTESIAN_POINT ( 'NONE',  ( -24.40658499505739698, -15.78250870199476630, 69.83307488408829045 ) ) ;
#28191 = DIRECTION ( 'NONE',  ( 3.413470714839332458E-33, -1.190614954331866791E-16, 1.000000000000000000 ) ) ;
#28192 = VERTEX_POINT ( 'NONE', #36813 ) ;
#28193 = CARTESIAN_POINT ( 'NONE',  ( -22.00117057250496444, -9.443090202341716477, 63.60642510345682155 ) ) ;
#28194 = CARTESIAN_POINT ( 'NONE',  ( -22.14090652532222236, -20.04928072148792495, 62.51967078134249078 ) ) ;
#28195 = DIRECTION ( 'NONE',  ( 0.5589780652556124441, -0.8291824422665291516, 7.938832475108296738E-08 ) ) ;
#28196 = CARTESIAN_POINT ( 'NONE',  ( -12.45907596150898300, -19.82553632194446180, 58.08249573729000304 ) ) ;
#28197 = CARTESIAN_POINT ( 'NONE',  ( -20.18941521006531303, -7.891347330600439136, 73.83601268700121523 ) ) ;
#28198 = CARTESIAN_POINT ( 'NONE',  ( -14.36817892824948473, -8.455618309860652104, 67.54503025475186462 ) ) ;
#28199 = B_SPLINE_CURVE_WITH_KNOTS ( 'NONE', 3,
 ( #43321, #46996, #13242, #9342, #24842, #32697, #2665, #9593, #32232, #47248 ),
 .UNSPECIFIED., .F., .F.,
 ( 4, 2, 2, 2, 4 ),
 ( 0.6272669072976907456, 0.7522669073147264518, 0.8772669073317622690, 1.002266907348797975, 1.127266907365833681 ),
 .UNSPECIFIED. ) ;
#28200 = CARTESIAN_POINT ( 'NONE',  ( -13.11946129443726861, -9.225960368241006293, 67.37942785707225823 ) ) ;
#28201 = VERTEX_POINT ( 'NONE', #24567 ) ;
#28202 = CARTESIAN_POINT ( 'NONE',  ( -13.91686280105865947, -8.236299372188803147, 74.31459218752463869 ) ) ;
#28203 = VECTOR ( 'NONE', #40320, 1000.000000000000000 ) ;
#28204 = PLANE ( 'NONE',  #47076 ) ;
#28205 = ORIENTED_EDGE ( 'NONE', *, *, #35013, .T. ) ;
#28206 = DIRECTION ( 'NONE',  ( 1.000000000000000000, 0.000000000000000000, -8.260587980841940012E-17 ) ) ;
#28207 = CIRCLE ( 'NONE', #13238, 3.951441697420975618 ) ;
#28208 = AXIS2_PLACEMENT_3D ( 'NONE', #24523, #16850, #36049 ) ;
#28209 = ORIENTED_EDGE ( 'NONE', *, *, #11390, .F. ) ;
#28210 = ORIENTED_EDGE ( 'NONE', *, *, #40941, .T. ) ;
#28211 = ORIENTED_EDGE ( 'NONE', *, *, #17229, .T. ) ;
#28212 = CARTESIAN_POINT ( 'NONE',  ( -14.07761608144266674, -20.95746532167037302, 71.92607703845176559 ) ) ;
#28213 = AXIS2_PLACEMENT_3D ( 'NONE', #32654, #25509, #43755 ) ;
#28214 = CARTESIAN_POINT ( 'NONE',  ( -23.76770236311157802, -11.84941793196945881, 59.78235735876457824 ) ) ;
#28215 = CARTESIAN_POINT ( 'NONE',  ( -14.98927377128267047, -8.246306944878837086, 57.14999999999994884 ) ) ;
#28216 = DIRECTION ( 'NONE',  ( -1.000000000000000000, 0.000000000000000000, 0.000000000000000000 ) ) ;
#28217 = ORIENTED_EDGE ( 'NONE', *, *, #19658, .T. ) ;
#28218 = VERTEX_POINT ( 'NONE', #31937 ) ;
#28219 = CARTESIAN_POINT ( 'NONE',  ( -21.26159385650551314, -9.295667164867525756, 49.30633214617472504 ) ) ;
#28220 = ADVANCED_FACE ( 'NONE', ( #46951 ), #13197, .T. ) ;
#28221 = CARTESIAN_POINT ( 'NONE',  ( -21.53994948931798703, -21.01915008201228474, 72.78092378945153484 ) ) ;
#28222 = CARTESIAN_POINT ( 'NONE',  ( -20.66696855643225561, -21.06909979829504209, 58.94475164909854925 ) ) ;
#28223 = DIRECTION ( 'NONE',  ( 2.866981220435666553E-17, -1.000000000000000000, -1.190614954331866791E-16 ) ) ;
#28224 = CARTESIAN_POINT ( 'NONE',  ( -13.29909385650551812, -8.114302828567740988, 52.18300498402516041 ) ) ;
#28226 = ORIENTED_EDGE ( 'NONE', *, *, #12473, .T. ) ;
#28225 = EDGE_CURVE ( 'NONE', #43774, #11839, #25209, .T. ) ;
#28227 = CARTESIAN_POINT ( 'NONE',  ( -10.37462439815953275, -14.89569326811688832, 74.94778901494476031 ) ) ;
#28228 = FACE_OUTER_BOUND ( 'NONE', #449, .T. ) ;
#28229 = EDGE_CURVE ( 'NONE', #23858, #16276, #32605, .T. ) ;
#28230 = AXIS2_PLACEMENT_3D ( 'NONE', #37181, #43891, #6926 ) ;
#28232 = CARTESIAN_POINT ( 'NONE',  ( -24.43499015649444317, -15.57872826220114781, 69.41818628325123086 ) ) ;
#28231 = B_SPLINE_CURVE_WITH_KNOTS ( 'NONE', 1,
 ( #23673, #15765 ),
 .UNSPECIFIED., .F., .F.,
 ( 2, 2 ),
 ( 0.000000000000000000, 1.000000000000000000 ),
 .UNSPECIFIED. ) ;
#28233 =( BOUNDED_SURFACE ( )  B_SPLINE_SURFACE ( 3, 1, ( 
 ( #18229, #29330 ),
 ( #6680, #10391 ),
 ( #35979, #44138 ),
 ( #48041, #2969 ),
 ( #2260, #25627 ),
 ( #14508, #17982 ),
 ( #25397, #21225 ) ),
 .UNSPECIFIED., .T., .F., .F. ) 
 B_SPLINE_SURFACE_WITH_KNOTS ( ( 4, 3, 4 ),
 ( 2, 2 ),
 ( 0.000000000000000000, 0.5000000000000000000, 1.000000000000000000 ),
 ( 0.000000000000000000, 1.000000000000000000 ),
 .UNSPECIFIED. ) 
 GEOMETRIC_REPRESENTATION_ITEM ( )  RATIONAL_B_SPLINE_SURFACE ( (
 ( 1.000000000000000000, 1.000000000000000000),
 ( 0.3333333333333335369, 0.3333333333333330373),
 ( 0.3333333333333335369, 0.3333333333333330373),
 ( 1.000000000000000000, 1.000000000000000000),
 ( 0.3333333333333333703, 0.3333333333333333703),
 ( 0.3333333333333333703, 0.3333333333333333703),
 ( 1.000000000000000000, 1.000000000000000000) ) ) 
 REPRESENTATION_ITEM ( '' )  SURFACE ( )  );
#28234 = EDGE_CURVE ( 'NONE', #34362, #21018, #7055, .T. ) ;
#28235 = ORIENTED_EDGE ( 'NONE', *, *, #48552, .T. ) ;
#28236 = CARTESIAN_POINT ( 'NONE',  ( -6.424093855413058662, -6.359206544744109735, 52.99999999999998579 ) ) ;
#28237 = CIRCLE ( 'NONE', #25111, 1.999999999999999112 ) ;
#28238 = VECTOR ( 'NONE', #31410, 1000.000000000000227 ) ;
#28239 = CARTESIAN_POINT ( 'NONE',  ( -10.69985271022639317, -16.93744915505940085, 61.57231810286263141 ) ) ;
#28240 = CARTESIAN_POINT ( 'NONE',  ( -11.01006245036516162, -12.00545227084238320, 74.57342739614527716 ) ) ;
#28241 = CARTESIAN_POINT ( 'NONE',  ( -9.424093855413055110, -25.10920654474410441, 56.99999999999997868 ) ) ;
#28242 = EDGE_CURVE ( 'NONE', #26610, #39233, #27562, .T. ) ;
#28243 = ORIENTED_EDGE ( 'NONE', *, *, #1067, .T. ) ;
#28244 = VECTOR ( 'NONE', #16371, 1000.000000000000000 ) ;
#28245 = CARTESIAN_POINT ( 'NONE',  ( -19.44376822123183146, -7.638105259791415413, 60.07597700946195829 ) ) ;
#28246 = CARTESIAN_POINT ( 'NONE',  ( -13.92409385541305511, -25.10920654474410441, 80.49999999999998579 ) ) ;
#28247 = LINE ( 'NONE', #2132, #47273 ) ;
#28248 = EDGE_LOOP ( 'NONE', ( #24359, #30117, #10951, #23610 ) ) ;
#28249 = DIRECTION ( 'NONE',  ( 0.9466432954593471116, 0.3222832157619555660, 8.771047036255756069E-09 ) ) ;
#28250 = EDGE_LOOP ( 'NONE', ( #22988, #12642, #29078, #44304, #12940 ) ) ;
#28251 = CARTESIAN_POINT ( 'NONE',  ( -11.76596577686094847, -10.68774762964470604, 74.45387372083885680 ) ) ;
#28252 = CARTESIAN_POINT ( 'NONE',  ( -10.37382936219775154, -14.83089353207902050, 74.81251018390587149 ) ) ;
#28253 = ORIENTED_EDGE ( 'NONE', *, *, #41950, .T. ) ;
#28254 = CYLINDRICAL_SURFACE ( 'NONE', #27390, 0.1500000000000079881 ) ;
#28255 = CARTESIAN_POINT ( 'NONE',  ( -20.04849592361258104, -21.35284569240296548, 72.69006679631317525 ) ) ;
#28256 = FACE_OUTER_BOUND ( 'NONE', #26464, .T. ) ;
#28257 = CARTESIAN_POINT ( 'NONE',  ( -17.42409385541299471, -14.80920654474435771, 49.52966884056655772 ) ) ;
#28258 = VERTEX_POINT ( 'NONE', #44986 ) ;
#28259 = CARTESIAN_POINT ( 'NONE',  ( -10.95917937052863245, -17.62195967018737264, 71.58190244267143498 ) ) ;
#28260 = UNCERTAINTY_MEASURE_WITH_UNIT (LENGTH_MEASURE( 1.000000000000000082E-05 ), #8127, 'distance_accuracy_value', 'NONE');
#28261 = DIRECTION ( 'NONE',  ( 6.023555219429074381E-06, -1.003033500007733605E-05, 0.9999999999315545285 ) ) ;
#28262 = CARTESIAN_POINT ( 'NONE',  ( -23.79376783276477525, -17.83917320997471023, 62.56540969546114894 ) ) ;
#28263 = EDGE_LOOP ( 'NONE', ( #4963, #48442, #25969, #22082, #15296 ) ) ;
#28264 = CARTESIAN_POINT ( 'NONE',  ( -15.93879930885703011, -7.917138641544859468, 67.15479422225766371 ) ) ;
#28265 = DIRECTION ( 'NONE',  ( 0.9939059412784551073, 0.1102314832132140626, 5.576311685107536405E-08 ) ) ;
#28266 = EDGE_LOOP ( 'NONE', ( #28362, #13655, #43295, #1035, #2055 ) ) ;
#28267 = ORIENTED_EDGE ( 'NONE', *, *, #7660, .T. ) ;
#28268 = CARTESIAN_POINT ( 'NONE',  ( -23.77487038158592014, -11.74745262826995607, 62.96690348473899235 ) ) ;
#28269 = DIRECTION ( 'NONE',  ( 3.413470714839332458E-33, -1.190614954331866791E-16, 1.000000000000000000 ) ) ;
#28270 = CARTESIAN_POINT ( 'NONE',  ( -17.82409385541305724, -14.80920654474411080, 47.99999999999997868 ) ) ;
#28271 = CARTESIAN_POINT ( 'NONE',  ( -18.08034385650551812, -6.424090610841176385, 49.80797279389977916 ) ) ;
#28272 = CYLINDRICAL_SURFACE ( 'NONE', #10972, 0.1500000000000015488 ) ;
#28273 = CARTESIAN_POINT ( 'NONE',  ( -24.46479344033866710, -14.44719916248949154, 66.33292729247949637 ) ) ;
#28274 = EDGE_CURVE ( 'NONE', #29708, #30119, #13317, .T. ) ;
#28275 = CARTESIAN_POINT ( 'NONE',  ( -23.48344415125163565, -18.41350569598871090, 73.04896097104848707 ) ) ;
#28276 = LINE ( 'NONE', #40550, #5092 ) ;
#28277 = AXIS2_PLACEMENT_3D ( 'NONE', #24880, #5451, #5697 ) ;
#28278 = VECTOR ( 'NONE', #19355, 1000.000000000000114 ) ;
#28279 = CARTESIAN_POINT ( 'NONE',  ( -16.70524046451162548, -22.22456740133032227, 68.87373416885567678 ) ) ;
#28280 = ORIENTED_EDGE ( 'NONE', *, *, #14251, .T. ) ;
#28281 = EDGE_LOOP ( 'NONE', ( #44703, #47107 ) ) ;
#28282 = CARTESIAN_POINT ( 'NONE',  ( -11.06793303470118950, -10.92167721944563397, 60.86541164553911187 ) ) ;
#28283 = EDGE_CURVE ( 'NONE', #39949, #5705, #19961, .T. ) ;
#28284 = DIRECTION ( 'NONE',  ( 1.000000000000000000, 0.000000000000000000, 0.000000000000000000 ) ) ;
#28285 = CARTESIAN_POINT ( 'NONE',  ( -12.17409406592225629, -14.80771982110106855, 49.52966884056655772 ) ) ;
#28286 = CARTESIAN_POINT ( 'NONE',  ( -11.41368471857665590, -18.49404720395463642, 61.27710860172267360 ) ) ;
#28287 = AXIS2_PLACEMENT_3D ( 'NONE', #13399, #47407, #36052 ) ;
#28288 = DIRECTION ( 'NONE',  ( -0.000000000000000000, -1.000000000000000000, 0.000000000000000000 ) ) ;
#28289 = CARTESIAN_POINT ( 'NONE',  ( -20.47136568995129480, -10.23054578351413468, 53.49899999999994549 ) ) ;
#28290 =( BOUNDED_SURFACE ( )  B_SPLINE_SURFACE ( 3, 1, ( 
 ( #28887, #14554 ),
 ( #14083, #21516 ),
 ( #10191, #37225 ),
 ( #29376, #25205 ),
 ( #40224, #10433 ),
 ( #29617, #6495 ),
 ( #28653, #36497 ) ),
 .UNSPECIFIED., .T., .F., .F. ) 
 B_SPLINE_SURFACE_WITH_KNOTS ( ( 4, 3, 4 ),
 ( 2, 2 ),
 ( 0.000000000000000000, 0.5000000000000000000, 1.000000000000000000 ),
 ( 0.000000000000000000, 1.000000000000000000 ),
 .UNSPECIFIED. ) 
 GEOMETRIC_REPRESENTATION_ITEM ( )  RATIONAL_B_SPLINE_SURFACE ( (
 ( 1.000000000000000000, 1.000000000000000000),
 ( 0.3333333333333335369, 0.3333333333333330373),
 ( 0.3333333333333335369, 0.3333333333333330373),
 ( 1.000000000000000000, 1.000000000000000000),
 ( 0.3333333333333333703, 0.3333333333333333703),
 ( 0.3333333333333333703, 0.3333333333333333703),
 ( 1.000000000000000000, 1.000000000000000000) ) ) 
 REPRESENTATION_ITEM ( '' )  SURFACE ( )  );
#28291 = EDGE_LOOP ( 'NONE', ( #14409, #22469, #32940, #47930, #3336 ) ) ;
#28292 = CARTESIAN_POINT ( 'NONE',  ( -19.79646526366146375, -21.45124607735644062, 72.81967355032548994 ) ) ;
#28293 = DIRECTION ( 'NONE',  ( 1.224646799147352961E-16, 1.000000000000000000, -5.292884291094200710E-16 ) ) ;
#28294 = EDGE_CURVE ( 'NONE', #13051, #15441, #40772, .T. ) ;
#28295 = B_SPLINE_CURVE_WITH_KNOTS ( 'NONE', 3,
 ( #46214, #27254, #23321, #38317, #38570, #8801, #23818, #204, #38819, #20106 ),
 .UNSPECIFIED., .F., .F.,
 ( 4, 2, 2, 2, 4 ),
 ( 0.000000000000000000, 0.2500000000000000000, 0.5000000000000000000, 0.7500000000000000000, 1.000000000000000000 ),
 .UNSPECIFIED. ) ;
#28296 = CARTESIAN_POINT ( 'NONE',  ( -14.73594855369633905, -7.860282982240396343, 60.50651534380390473 ) ) ;
#28297 = CARTESIAN_POINT ( 'NONE',  ( -13.80534385541286113, -7.595227055684621753, 51.75156210489625863 ) ) ;
#28298 = EDGE_CURVE ( 'NONE', #12632, #42290, #41507, .T. ) ;
#28299 = ORIENTED_EDGE ( 'NONE', *, *, #16767, .T. ) ;
#28300 =( BOUNDED_CURVE ( )  B_SPLINE_CURVE ( 3, ( #15344, #361, #44942, #26942 ),
 .UNSPECIFIED., .F., .F. ) 
 B_SPLINE_CURVE_WITH_KNOTS ( ( 4, 4 ),
 ( 0.4074455897393673420, 0.5000000000000000000 ),
 .UNSPECIFIED. ) 
 CURVE ( )  GEOMETRIC_REPRESENTATION_ITEM ( )  RATIONAL_B_SPLINE_CURVE ( ( 0.6983129098260978385, 0.7760317562607030872, 0.8765941196520039558, 1.000000000000001110 ) ) 
 REPRESENTATION_ITEM ( '' )  );
#28301 = CARTESIAN_POINT ( 'NONE',  ( -11.21695167451617792, -18.92928555840075688, 64.79061121450172323 ) ) ;
#28302 = EDGE_CURVE ( 'NONE', #35582, #11018, #30046, .T. ) ;
#28303 = LINE ( 'NONE', #10550, #36918 ) ;
#28304 = CARTESIAN_POINT ( 'NONE',  ( -16.71219879347879100, -22.22520166962337740, 68.81065243885818461 ) ) ;
#28305 = TOROIDAL_SURFACE ( 'NONE', #25912, 1.500000000000008660, 0.5000000000000000000 ) ;
#28306 = CARTESIAN_POINT ( 'NONE',  ( -10.53536195276627829, -13.30851587854854401, 74.69289754060230280 ) ) ;
#28307 = CARTESIAN_POINT ( 'NONE',  ( -17.39742543611924575, -7.759256981132185871, 67.32039592192056432 ) ) ;
#28308 = EDGE_CURVE ( 'NONE', #6954, #4804, #30273, .T. ) ;
#28309 = CARTESIAN_POINT ( 'NONE',  ( -22.66784385759799392, -9.357632978295830739, 49.97845033065683396 ) ) ;
#28310 = CARTESIAN_POINT ( 'NONE',  ( -18.92057629138644970, -7.919864069981281673, 67.05071783789199458 ) ) ;
#28311 = EDGE_LOOP ( 'NONE', ( #25337, #10572, #23407, #33039, #23839, #45914, #39865, #3542 ) ) ;
#28312 = CARTESIAN_POINT ( 'NONE',  ( -13.01616685277437568, -9.306763517318225709, 70.86397465682092900 ) ) ;
#28313 = VECTOR ( 'NONE', #43730, 1000.000000000000227 ) ;
#28314 = ORIENTED_EDGE ( 'NONE', *, *, #5933, .F. ) ;
#28315 = CARTESIAN_POINT ( 'NONE',  ( -15.01784385759799179, -6.860780111191481900, 51.02154966934377001 ) ) ;
#28316 = B_SPLINE_CURVE_WITH_KNOTS ( 'NONE', 3,
 ( #14805, #14557, #13846, #10665, #7229, #40691, #40944, #29618, #36499, #36274 ),
 .UNSPECIFIED., .F., .F.,
 ( 4, 2, 2, 2, 4 ),
 ( 0.1272669073658274363, 0.2522669073463031930, 0.3772669073267790329, 0.5022669073072547619, 0.6272669072877306018 ),
 .UNSPECIFIED. ) ;
#28317 = DIRECTION ( 'NONE',  ( 0.000000000000000000, 0.000000000000000000, 1.000000000000000000 ) ) ;
#28318 = ORIENTED_EDGE ( 'NONE', *, *, #47660, .T. ) ;
#28319 = DIRECTION ( 'NONE',  ( 0.6323592902076723421, 0.7746752403995150749, -4.984538757074893987E-08 ) ) ;
#28320 = CARTESIAN_POINT ( 'NONE',  ( -14.00534385650551705, -8.801233750844183135, 48.81488406609782515 ) ) ;
#28321 = ORIENTED_EDGE ( 'NONE', *, *, #34090, .F. ) ;
#28322 = CARTESIAN_POINT ( 'NONE',  ( -12.01398192529223685, -10.36526672924184389, 71.19723003267655770 ) ) ;
#28323 = VECTOR ( 'NONE', #25191, 1000.000000000000000 ) ;
#28324 = CARTESIAN_POINT ( 'NONE',  ( -19.79948111938147548, -8.167596747518278022, 73.92916665838981771 ) ) ;
#28325 = CARTESIAN_POINT ( 'NONE',  ( -10.88209246082447912, -17.29963176008448400, 64.92739380462948873 ) ) ;
#28326 = ORIENTED_EDGE ( 'NONE', *, *, #30506, .F. ) ;
#28327 = CARTESIAN_POINT ( 'NONE',  ( -23.86889929688984324, -17.54148027364508877, 62.48863461348566517 ) ) ;
#28328 = DIRECTION ( 'NONE',  ( -0.4639960340712762088, 0.8858372764600319638, 1.164945627098518506E-17 ) ) ;
#28329 = DIRECTION ( 'NONE',  ( -3.071710424422018668E-17, 6.404604876783312462E-16, 1.000000000000000000 ) ) ;
#28330 = DIRECTION ( 'NONE',  ( 0.000000000000000000, 0.9999954153791273948, 0.003028072113819836077 ) ) ;
#28331 = ORIENTED_EDGE ( 'NONE', *, *, #23650, .T. ) ;
#28332 = ORIENTED_EDGE ( 'NONE', *, *, #46106, .T. ) ;
#28333 = CARTESIAN_POINT ( 'NONE',  ( -11.68335550665270794, -18.81469308649876737, 68.21689631955439381 ) ) ;
#28334 = CARTESIAN_POINT ( 'NONE',  ( -24.31977367176101268, -16.01319989648291653, 62.78431746014856429 ) ) ;
#28335 = EDGE_LOOP ( 'NONE', ( #44118, #16169 ) ) ;
#28336 = CARTESIAN_POINT ( 'NONE',  ( -24.33438867869370981, -15.92703613221075543, 66.36324874061841683 ) ) ;
#28337 = CARTESIAN_POINT ( 'NONE',  ( -17.26784385759799179, -9.357632978295830739, 49.97845033065684106 ) ) ;
#28338 = CARTESIAN_POINT ( 'NONE',  ( -23.83107790926975511, -11.00715885964709173, 73.50159964070205376 ) ) ;
#28339 = EDGE_CURVE ( 'NONE', #45073, #46946, #3587, .T. ) ;
#28340 = DIRECTION ( 'NONE',  ( -3.071710424422018668E-17, 6.404604876783312462E-16, 1.000000000000000000 ) ) ;
#28341 = DIRECTION ( 'NONE',  ( 0.000000000000000000, 0.000000000000000000, 1.000000000000000000 ) ) ;
#28342 = ORIENTED_EDGE ( 'NONE', *, *, #26105, .T. ) ;
#28343 = DIRECTION ( 'NONE',  ( -2.866981220435666553E-17, 1.000000000000000000, 1.190614954331866791E-16 ) ) ;
#28344 = CARTESIAN_POINT ( 'NONE',  ( -10.42874009550524761, -15.68648592809493358, 61.33229246353490538 ) ) ;
#28345 = AXIS2_PLACEMENT_3D ( 'NONE', #20246, #24190, #16049 ) ;
#28346 = CARTESIAN_POINT ( 'NONE',  ( -24.47432067347917695, -14.77756146504815327, 59.52828185648635184 ) ) ;
#28347 = DIRECTION ( 'NONE',  ( 0.2479245821708711550, 0.9687793358424812151, 0.000000000000000000 ) ) ;
#28348 = ADVANCED_FACE ( 'NONE', ( #34108, #398 ), #26744, .F. ) ;
#28349 = VECTOR ( 'NONE', #1292, 1000.000000000000114 ) ;
#28350 = VERTEX_POINT ( 'NONE', #10734 ) ;
#28351 = VERTEX_POINT ( 'NONE', #12199 ) ;
#28352 = EDGE_LOOP ( 'NONE', ( #22067, #37419, #31999, #42938, #10728 ) ) ;
#28353 = CARTESIAN_POINT ( 'NONE',  ( -17.42409385541299471, -14.80920654474435771, 49.52966884056655772 ) ) ;
#28354 = SURFACE_STYLE_USAGE ( .BOTH. , #28822 ) ;
#28355 = EDGE_CURVE ( 'NONE', #1165, #31902, #40203, .T. ) ;
#28356 = CARTESIAN_POINT ( 'NONE',  ( -15.35027035934970918, -7.653577032698213323, 74.26481056556292515 ) ) ;
#28357 = AXIS2_PLACEMENT_3D ( 'NONE', #7362, #26799, #45042 ) ;
#28358 = ORIENTED_EDGE ( 'NONE', *, *, #22104, .F. ) ;
#28359 = DIRECTION ( 'NONE',  ( -0.2479245821708774278, -0.9687793358424795498, 0.000000000000000000 ) ) ;
#28360 = EDGE_CURVE ( 'NONE', #23803, #12455, #34842, .T. ) ;
#28361 = LINE ( 'NONE', #17253, #22538 ) ;
#28362 = ORIENTED_EDGE ( 'NONE', *, *, #43199, .F. ) ;
#28363 = CARTESIAN_POINT ( 'NONE',  ( -13.26872317195175199, -21.05283485551296607, 53.49999999999994316 ) ) ;
#28364 = ADVANCED_FACE ( 'NONE', ( #20318 ), #5871, .T. ) ;
#28365 = CARTESIAN_POINT ( 'NONE',  ( -12.96549398033168288, -9.412670339977610823, 70.84925319149679979 ) ) ;
#28366 = ORIENTED_EDGE ( 'NONE', *, *, #29572, .F. ) ;
#28367 = DIRECTION ( 'NONE',  ( 0.9979768094191903138, 0.06357898915123821881, 0.000000000000000000 ) ) ;
#28368 = VERTEX_POINT ( 'NONE', #45714 ) ;
#28369 = CARTESIAN_POINT ( 'NONE',  ( -17.52853272358826686, -7.759682304905023642, 63.83584969886392457 ) ) ;
#28370 = ORIENTED_EDGE ( 'NONE', *, *, #28090, .T. ) ;
#28371 = CARTESIAN_POINT ( 'NONE',  ( -15.73993337224566247, -7.955115359200574332, 63.82577855974437853 ) ) ;
#28372 = CARTESIAN_POINT ( 'NONE',  ( -18.28034385759798752, -9.360768649639306105, 51.01397948905922419 ) ) ;
#28373 = CARTESIAN_POINT ( 'NONE',  ( -19.23866243364646422, -21.62168334911581269, 58.52507384657483414 ) ) ;
#28374 = VERTEX_POINT ( 'NONE', #42001 ) ;
#28375 = CYLINDRICAL_SURFACE ( 'NONE', #41968, 1.999999999999999112 ) ;
#28376 = DIRECTION ( 'NONE',  ( 0.000000000000000000, 0.000000000000000000, -1.000000000000000000 ) ) ;
#28377 = CARTESIAN_POINT ( 'NONE',  ( -50.42609385541305755, -14.80920654474413745, 60.91764705882351905 ) ) ;
#28378 = CIRCLE ( 'NONE', #7147, 1.900000000000000133 ) ;
#28379 = ADVANCED_FACE ( 'NONE', ( #1342 ), #38276, .T. ) ;
#28380 = CARTESIAN_POINT ( 'NONE',  ( -14.83720200468841810, -10.88702015217558206, 52.02966884056656482 ) ) ;
#28381 = CARTESIAN_POINT ( 'NONE',  ( -22.48964968825576705, -9.905448439006629968, 73.76689030015370463 ) ) ;
#28382 = LINE ( 'NONE', #1788, #27424 ) ;
#28383 = VERTEX_POINT ( 'NONE', #9002 ) ;
#28384 = AXIS2_PLACEMENT_3D ( 'NONE', #48380, #8031, #41487 ) ;
#28385 = CARTESIAN_POINT ( 'NONE',  ( -17.51532316199698158, -7.809739782127767427, 63.83591710975426992 ) ) ;
#28386 = ADVANCED_FACE ( 'NONE', ( #9243 ), #4333, .T. ) ;
#28387 = FACE_OUTER_BOUND ( 'NONE', #42046, .T. ) ;
#28388 = DIRECTION ( 'NONE',  ( 0.9687793358424821033, -0.2479245821708677133, 0.000000000000000000 ) ) ;
#28389 = CARTESIAN_POINT ( 'NONE',  ( -13.41658284876181995, -21.09041002232991957, 61.62990919978891924 ) ) ;
#28390 = CARTESIAN_POINT ( 'NONE',  ( -10.99582178678916833, -11.91441492378913658, 74.85840195586327184 ) ) ;
#28391 = EDGE_CURVE ( 'NONE', #9477, #43598, #29019, .T. ) ;
#28392 = CARTESIAN_POINT ( 'NONE',  ( -24.28474004986992796, -16.19955753861012582, 62.89328727869452962 ) ) ;
#28393 = ORIENTED_EDGE ( 'NONE', *, *, #13193, .T. ) ;
#28394 = CARTESIAN_POINT ( 'NONE',  ( -22.67088471252091963, -10.17541515747705461, 66.61470292127093273 ) ) ;
#28395 = CARTESIAN_POINT ( 'NONE',  ( -24.83263366448169762, -15.59490076022755112, 73.18799035805197661 ) ) ;
#28396 = ORIENTED_EDGE ( 'NONE', *, *, #32444, .F. ) ;
#28397 = DIRECTION ( 'NONE',  ( 2.866981220435666553E-17, -1.000000000000000000, -2.395284034871317367E-16 ) ) ;
#28398 = AXIS2_PLACEMENT_3D ( 'NONE', #5881, #13487, #24354 ) ;
#28399 = CARTESIAN_POINT ( 'NONE',  ( -22.72409385759798894, -9.359200813967568422, 50.49621490985803263 ) ) ;
#28400 = DIRECTION ( 'NONE',  ( -5.731567514496413899E-31, -1.020425574103664789E-16, -1.000000000000000000 ) ) ;
#28401 = ORIENTED_EDGE ( 'NONE', *, *, #40291, .T. ) ;
#28402 = CARTESIAN_POINT ( 'NONE',  ( -23.76058108042893480, -11.83148235802054415, 63.18048099588689581 ) ) ;
#28403 = CARTESIAN_POINT ( 'NONE',  ( -42.81012326717776517, -14.80920654474412679, 59.91176470588234793 ) ) ;
#28404 = LINE ( 'NONE', #10418, #28323 ) ;
#28405 = ORIENTED_EDGE ( 'NONE', *, *, #5712, .T. ) ;
#28406 = VECTOR ( 'NONE', #26734, 1000.000000000000227 ) ;
#28407 = DIRECTION ( 'NONE',  ( 0.9687793358424821033, -0.2479245821708679909, 0.000000000000000000 ) ) ;
#28408 = DIRECTION ( 'NONE',  ( 3.549360974554993999E-17, -6.371834667797928663E-18, -1.000000000000000000 ) ) ;
#28409 = CARTESIAN_POINT ( 'NONE',  ( -10.40385083531699273, -12.31531819518022353, 57.52131499152729788 ) ) ;
#28410 = CARTESIAN_POINT ( 'NONE',  ( -21.04010759901128225, -20.80440105208702661, 69.28280143620438025 ) ) ;
#28411 = CARTESIAN_POINT ( 'NONE',  ( -20.47136568995129480, -10.23054578351413468, 54.07175714974879099 ) ) ;
#28412 = CARTESIAN_POINT ( 'NONE',  ( -46.29409385541305255, -13.24559821555319239, 69.99777223794899328 ) ) ;
#28413 = VERTEX_POINT ( 'NONE', #20073 ) ;
#28414 = VERTEX_POINT ( 'NONE', #27704 ) ;
#28415 = CARTESIAN_POINT ( 'NONE',  ( -18.58659385541304232, -7.222650657624104298, 49.61879703869476543 ) ) ;
#28416 = MECHANICAL_DESIGN_GEOMETRIC_PRESENTATION_REPRESENTATION (  '', ( #4064 ), #29992 ) ;
#28417 = CARTESIAN_POINT ( 'NONE',  ( -13.49267557974227394, -8.956801037788498121, 60.45422421514565059 ) ) ;
#28418 = VECTOR ( 'NONE', #37410, 1000.000000000000000 ) ;
#28419 = EDGE_CURVE ( 'NONE', #12756, #25645, #47250, .T. ) ;
#28420 = CARTESIAN_POINT ( 'NONE',  ( -14.20477006803791475, -8.593354865760924000, 71.01492291173906324 ) ) ;
#28421 = CARTESIAN_POINT ( 'NONE',  ( -14.02541561442408913, -20.92883260698763692, 68.52913103262484640 ) ) ;
#28422 = EDGE_LOOP ( 'NONE', ( #37158, #44314 ) ) ;
#28423 = CARTESIAN_POINT ( 'NONE',  ( -11.02842221325288996, -10.98838527758271155, 60.78611644236347189 ) ) ;
#28424 = VECTOR ( 'NONE', #3696, 1000.000000000000000 ) ;
#28425 = CARTESIAN_POINT ( 'NONE',  ( -24.05420634179087358, -17.20676946999824608, 69.69867738674849988 ) ) ;
#28426 =( BOUNDED_CURVE ( )  B_SPLINE_CURVE ( 3, ( #24762, #43967, #2812, #36057 ),
 .UNSPECIFIED., .F., .F. ) 
 B_SPLINE_CURVE_WITH_KNOTS ( ( 4, 4 ),
 ( 4.712388980384691450, 4.921828490624010399 ),
 .UNSPECIFIED. ) 
 CURVE ( )  GEOMETRIC_REPRESENTATION_ITEM ( )  RATIONAL_B_SPLINE_CURVE ( ( 1.000000000000000000, 0.9963479302455156006, 0.9963479302455156006, 1.000000000000000000 ) ) 
 REPRESENTATION_ITEM ( '' )  );
#28427 = ORIENTED_EDGE ( 'NONE', *, *, #27739, .T. ) ;
#28428 = B_SPLINE_CURVE_WITH_KNOTS ( 'NONE', 1,
 ( #44216, #43965 ),
 .UNSPECIFIED., .F., .F.,
 ( 2, 2 ),
 ( 0.000000000000000000, 1.000000000000000000 ),
 .UNSPECIFIED. ) ;
#28429 = CARTESIAN_POINT ( 'NONE',  ( -17.99994007944887286, -22.23708576427155137, 62.01389424133448358 ) ) ;
#28430 = LINE ( 'NONE', #5544, #6265 ) ;
#28431 = EDGE_LOOP ( 'NONE', ( #12514, #2589 ) ) ;
#28432 = FACE_OUTER_BOUND ( 'NONE', #43146, .T. ) ;
#28433 = CARTESIAN_POINT ( 'NONE',  ( -14.93633297159279216, -21.40954675051312250, 58.37437924742020101 ) ) ;
#28434 = VERTEX_POINT ( 'NONE', #42735 ) ;
#28435 = DIRECTION ( 'NONE',  ( -1.000000000000000000, 4.164305804376849172E-17, -1.614929280266638808E-16 ) ) ;
#28436 = AXIS2_PLACEMENT_3D ( 'NONE', #4625, #20376, #46721 ) ;
#28437 = LINE ( 'NONE', #28672, #9272 ) ;
#28438 = B_SPLINE_CURVE_WITH_KNOTS ( 'NONE', 3,
 ( #2572, #24748, #25225, #21041, #9960, #24980, #40249, #6266, #6514, #36290 ),
 .UNSPECIFIED., .F., .F.,
 ( 4, 2, 2, 2, 4 ),
 ( 0.000000000000000000, 0.2500000000000000000, 0.5000000000000000000, 0.7500000000000000000, 1.000000000000000000 ),
 .UNSPECIFIED. ) ;
#28439 =( BOUNDED_CURVE ( )  B_SPLINE_CURVE ( 3, ( #13908, #14145, #25740, #28950 ),
 .UNSPECIFIED., .F., .F. ) 
 B_SPLINE_CURVE_WITH_KNOTS ( ( 4, 4 ),
 ( 0.9074455897393647330, 1.000000000000000000 ),
 .UNSPECIFIED. ) 
 CURVE ( )  GEOMETRIC_REPRESENTATION_ITEM ( )  RATIONAL_B_SPLINE_CURVE ( ( 0.6983129098260816292, 0.7760317562606884323, 0.8765941196519945189, 1.000000000000000000 ) ) 
 REPRESENTATION_ITEM ( '' )  );
#28440 = CARTESIAN_POINT ( 'NONE',  ( -23.23616409499837943, -18.79948708312782557, 65.82389430043846801 ) ) ;
#28441 = LINE ( 'NONE', #24749, #29196 ) ;
#28442 = ORIENTED_EDGE ( 'NONE', *, *, #19637, .F. ) ;
#28443 = CARTESIAN_POINT ( 'NONE',  ( -22.04378365035703879, -20.13510231884741231, 62.24911246861644543 ) ) ;
#28444 =( BOUNDED_CURVE ( )  B_SPLINE_CURVE ( 3, ( #43930, #2060, #43193, #1820 ),
 .UNSPECIFIED., .F., .F. ) 
 B_SPLINE_CURVE_WITH_KNOTS ( ( 4, 4 ),
 ( 0.9074455897393670645, 1.000000000000000000 ),
 .UNSPECIFIED. ) 
 CURVE ( )  GEOMETRIC_REPRESENTATION_ITEM ( )  RATIONAL_B_SPLINE_CURVE ( ( 0.6983129098260988377, 0.7760317562607031983, 0.8765941196520036227, 1.000000000000000000 ) ) 
 REPRESENTATION_ITEM ( '' )  );
#28445 = LINE ( 'NONE', #9964, #30239 ) ;
#28446 = EDGE_CURVE ( 'NONE', #11860, #11979, #856, .T. ) ;
#28447 = CARTESIAN_POINT ( 'NONE',  ( -15.53817126359833445, -8.015982722819853024, 74.08545464501875699 ) ) ;
#28448 = AXIS2_PLACEMENT_3D ( 'NONE', #9996, #46938, #32170 ) ;
#28449 = ADVANCED_FACE ( 'NONE', ( #38782 ), #14019, .T. ) ;
#28450 = ADVANCED_FACE ( 'NONE', ( #36044 ), #24517, .F. ) ;
#28451 = CARTESIAN_POINT ( 'NONE',  ( -20.20088676517873694, -8.325823464045813083, 74.13585170226248522 ) ) ;
#28452 = CARTESIAN_POINT ( 'NONE',  ( -11.47771132772901659, -11.11285210769868748, 60.86812947373131522 ) ) ;
#28453 = VECTOR ( 'NONE', #28143, 1000.000000000000114 ) ;
#28454 = CARTESIAN_POINT ( 'NONE',  ( -17.81160558974998764, -14.71003671187600936, 49.52966884056655772 ) ) ;
#28455 = EDGE_LOOP ( 'NONE', ( #30676, #41222, #33998, #21859, #21008 ) ) ;
#28456 = CARTESIAN_POINT ( 'NONE',  ( -16.65185932245351452, -21.81708442718849383, 65.51092266128213737 ) ) ;
#28457 = CARTESIAN_POINT ( 'NONE',  ( -14.24639973016467742, -8.070891362069774644, 67.45963869169959537 ) ) ;
#28458 = LINE ( 'NONE', #43481, #22774 ) ;
#28459 = EDGE_LOOP ( 'NONE', ( #35606, #4383, #14077, #9866 ) ) ;
#28460 = CARTESIAN_POINT ( 'NONE',  ( -13.57571756020798581, -20.65642803140422856, 61.51646323935151628 ) ) ;
#28461 =( BOUNDED_CURVE ( )  B_SPLINE_CURVE ( 3, ( #868, #18404, #7107, #48210 ),
 .UNSPECIFIED., .F., .F. ) 
 B_SPLINE_CURVE_WITH_KNOTS ( ( 4, 4 ),
 ( 0.9074455897393649551, 1.000000000000000000 ),
 .UNSPECIFIED. ) 
 CURVE ( )  GEOMETRIC_REPRESENTATION_ITEM ( )  RATIONAL_B_SPLINE_CURVE ( ( 0.6983129098260953960, 0.7760317562607003117, 0.8765941196520018464, 1.000000000000000000 ) ) 
 REPRESENTATION_ITEM ( '' )  );
#28462 = VERTEX_POINT ( 'NONE', #13392 ) ;
#28463 = ORIENTED_EDGE ( 'NONE', *, *, #29300, .T. ) ;
#28464 = ORIENTED_EDGE ( 'NONE', *, *, #11328, .F. ) ;
#28465 = CARTESIAN_POINT ( 'NONE',  ( -18.75169300116608184, -7.478281097746903860, 70.50921473615289869 ) ) ;
#28466 = DIRECTION ( 'NONE',  ( 2.181982678098338148E-16, 0.000000000000000000, -1.000000000000000000 ) ) ;
#28467 = CARTESIAN_POINT ( 'NONE',  ( -16.00300465971815811, -7.954912822689343521, 63.68513404597024419 ) ) ;
#28468 = CARTESIAN_POINT ( 'NONE',  ( -15.39536932222403287, -19.92137602241599836, 54.07175714974879099 ) ) ;
#28469 = CARTESIAN_POINT ( 'NONE',  ( -17.02409385541305653, -14.80920654474410725, 52.21286476528345588 ) ) ;
#28470 = EDGE_LOOP ( 'NONE', ( #22074, #32608, #40385, #37652 ) ) ;
#28471 = ORIENTED_EDGE ( 'NONE', *, *, #18905, .T. ) ;
#28472 = CARTESIAN_POINT ( 'NONE',  ( -19.29284385650551670, -7.406986770994973490, 48.81910596585309747 ) ) ;
#28473 = B_SPLINE_CURVE_WITH_KNOTS ( 'NONE', 3,
 ( #46944, #28954, #28240, #9287, #12957, #16657, #24311, #39317, #43269, #9538 ),
 .UNSPECIFIED., .F., .F.,
 ( 4, 2, 2, 2, 4 ),
 ( 0.000000000000000000, 0.2500000000000000000, 0.5000000000000000000, 0.7500000000000000000, 1.000000000000000000 ),
 .UNSPECIFIED. ) ;
#28474 = EDGE_CURVE ( 'NONE', #15704, #30331, #19085, .T. ) ;
#28475 = CARTESIAN_POINT ( 'NONE',  ( -20.89788161767221197, -20.94431024770144489, 62.39999296070408974 ) ) ;
#28476 = CARTESIAN_POINT ( 'NONE',  ( -23.19494587819374942, -18.77118419879135303, 66.12389430422854275 ) ) ;
#28477 = CARTESIAN_POINT ( 'NONE',  ( -17.88659385650551670, -9.302874398569244363, 51.68646062012417985 ) ) ;
#28478 = ORIENTED_EDGE ( 'NONE', *, *, #30081, .F. ) ;
#28479 = FACE_OUTER_BOUND ( 'NONE', #27916, .T. ) ;
#28480 = AXIS2_PLACEMENT_3D ( 'NONE', #23027, #7765, #29916 ) ;
#28481 = EDGE_CURVE ( 'NONE', #31312, #29256, #40150, .T. ) ;
#28482 = CARTESIAN_POINT ( 'NONE',  ( -9.985306297970870659, -8.645400713382203506, 54.50428052266513390 ) ) ;
#28483 = ORIENTED_EDGE ( 'NONE', *, *, #24891, .T. ) ;
#28484 = DIRECTION ( 'NONE',  ( 0.6264825908887947659, -0.7794354131762692983, 3.858680029754496854E-08 ) ) ;
#28485 = CARTESIAN_POINT ( 'NONE',  ( -17.79084088774826000, -7.768752266068900347, 60.08060768310445354 ) ) ;
#28486 = CARTESIAN_POINT ( 'NONE',  ( -11.33476804054750531, -19.10151225439055978, 68.40184904730287485 ) ) ;
#28487 = CARTESIAN_POINT ( 'NONE',  ( -21.99229891970641404, -20.18939897536854389, 65.84854503242263490 ) ) ;
#28488 = ORIENTED_EDGE ( 'NONE', *, *, #47661, .T. ) ;
#28489 = CARTESIAN_POINT ( 'NONE',  ( -19.36518065869528726, -8.031383756764064685, 59.97565108339750850 ) ) ;
#28490 = CARTESIAN_POINT ( 'NONE',  ( -22.66414149941106260, -10.08832384041532926, 66.42693508874704378 ) ) ;
#28491 = DIRECTION ( 'NONE',  ( -3.071710424422018668E-17, 6.404604876783312462E-16, 1.000000000000000000 ) ) ;
#28492 = EDGE_LOOP ( 'NONE', ( #15163, #42038 ) ) ;
#28493 = CYLINDRICAL_SURFACE ( 'NONE', #30738, 0.4000000000000010214 ) ;
#28494 = ORIENTED_EDGE ( 'NONE', *, *, #43538, .T. ) ;
#28495 = CARTESIAN_POINT ( 'NONE',  ( -13.29979614553676370, -21.01354653661592664, 61.77292273241334186 ) ) ;
#28496 = CARTESIAN_POINT ( 'NONE',  ( -10.37210014130659275, -14.68995570394611505, 75.21267707208666309 ) ) ;
#28497 = B_SPLINE_CURVE_WITH_KNOTS ( 'NONE', 3,
 ( #33159, #21854, #36849, #25793, #33396, #19875, #8307, #916, #27253, #46212 ),
 .UNSPECIFIED., .F., .F.,
 ( 4, 2, 2, 2, 4 ),
 ( 0.6272669072877905538, 0.7522669073073057211, 0.8772669073268208884, 1.002266907346335945, 1.127266907365851223 ),
 .UNSPECIFIED. ) ;
#28498 = ORIENTED_EDGE ( 'NONE', *, *, #32406, .F. ) ;
#28499 = ADVANCED_FACE ( 'NONE', ( #43218 ), #39272, .T. ) ;
#28500 = CARTESIAN_POINT ( 'NONE',  ( -11.01460970429776332, -11.87269385784942344, 74.56399918325968201 ) ) ;
#28501 = CARTESIAN_POINT ( 'NONE',  ( -10.39147815561416621, -17.41829018061022438, 53.49999999999995026 ) ) ;
#28502 = CARTESIAN_POINT ( 'NONE',  ( -24.48759320265496342, -17.17788619462897159, 72.92690118282537526 ) ) ;
#28503 = LINE ( 'NONE', #40307, #7811 ) ;
#28504 = ORIENTED_EDGE ( 'NONE', *, *, #27323, .T. ) ;
#28505 = CARTESIAN_POINT ( 'NONE',  ( -22.01903163361388494, -9.527854677399155037, 59.73787834519894346 ) ) ;
#28506 = CARTESIAN_POINT ( 'NONE',  ( -24.20884313412962285, -11.73171478914054155, 59.59740407230526671 ) ) ;
#28507 = DIRECTION ( 'NONE',  ( 0.9687793358424821033, -0.2479245821708679909, 0.000000000000000000 ) ) ;
#28508 = ORIENTED_EDGE ( 'NONE', *, *, #16294, .F. ) ;
#28509 = CARTESIAN_POINT ( 'NONE',  ( -11.17855889551124982, -18.87086522978130532, 64.86211687253867808 ) ) ;
#28510 = EDGE_CURVE ( 'NONE', #36768, #19883, #5795, .T. ) ;
#28511 = EDGE_CURVE ( 'NONE', #21615, #26298, #6708, .T. ) ;
#28512 = CARTESIAN_POINT ( 'NONE',  ( -19.55442184481404766, -21.52995072282663358, 65.47958309245051112 ) ) ;
#28513 = ORIENTED_EDGE ( 'NONE', *, *, #33873, .F. ) ;
#28514 = VERTEX_POINT ( 'NONE', #29333 ) ;
#28515 = ADVANCED_FACE ( 'NONE', ( #18473 ), #1847, .T. ) ;
#28516 = CARTESIAN_POINT ( 'NONE',  ( -14.05371270701021302, -21.00138147690670820, 71.92607703580544865 ) ) ;
#28517 = DIRECTION ( 'NONE',  ( -3.071710424422018668E-17, 6.404604876783312462E-16, 1.000000000000000000 ) ) ;
#28518 = CARTESIAN_POINT ( 'NONE',  ( -10.70296955259081351, -11.59513340129999648, 71.27356289404251299 ) ) ;
#28519 = ADVANCED_BREP_SHAPE_REPRESENTATION ( '', ( #31806, #29031 ), #10942 ) ;
#28520 = CARTESIAN_POINT ( 'NONE',  ( -17.06784385650551528, -6.428312510596451368, 51.20221977374900035 ) ) ;
#28521 = EDGE_CURVE ( 'NONE', #30462, #4687, #14510, .T. ) ;
#28522 = CARTESIAN_POINT ( 'NONE',  ( -23.47191072790384325, -19.15987225631625179, 62.53123744227819003 ) ) ;
#28523 = CARTESIAN_POINT ( 'NONE',  ( -19.45760789423921366, -7.641931476291664360, 60.10059647935476335 ) ) ;
#28524 = CARTESIAN_POINT ( 'NONE',  ( -14.94536180354596411, -8.261047468840590824, 60.43069275610791635 ) ) ;
#28525 = CARTESIAN_POINT ( 'NONE',  ( -12.19280364807469752, -20.11379078549368771, 65.00641491777591341 ) ) ;
#28526 = CARTESIAN_POINT ( 'NONE',  ( -16.75922336650640787, -22.22948809395919056, 68.89549426778991403 ) ) ;
#28527 = VERTEX_POINT ( 'NONE', #29827 ) ;
#28528 = EDGE_LOOP ( 'NONE', ( #45292, #10428, #27118, #33965, #37263 ) ) ;
#28529 = DIRECTION ( 'NONE',  ( 1.000000000000000000, 2.866981220435666553E-17, 0.000000000000000000 ) ) ;
#28530 = EDGE_CURVE ( 'NONE', #26257, #20160, #18232, .T. ) ;
#28531 = CARTESIAN_POINT ( 'NONE',  ( -18.31357888663955080, -21.80286911112441217, 69.11514702303101387 ) ) ;
#28532 = CARTESIAN_POINT ( 'NONE',  ( -50.42609385541305755, -14.80920654474416942, 63.93529411764704662 ) ) ;
#28533 =( BOUNDED_CURVE ( )  B_SPLINE_CURVE ( 3, ( #43872, #6182, #14263, #32525 ),
 .UNSPECIFIED., .F., .F. ) 
 B_SPLINE_CURVE_WITH_KNOTS ( ( 4, 4 ),
 ( 0.4074455897393690629, 0.5000000000000000000 ),
 .UNSPECIFIED. ) 
 CURVE ( )  GEOMETRIC_REPRESENTATION_ITEM ( )  RATIONAL_B_SPLINE_CURVE ( ( 0.6983129098261053880, 0.7760317562607058628, 0.8765941196520032896, 0.9999999999999953371 ) ) 
 REPRESENTATION_ITEM ( '' )  );
#28534 = FACE_OUTER_BOUND ( 'NONE', #12635, .T. ) ;
#28535 = B_SPLINE_CURVE_WITH_KNOTS ( 'NONE', 1,
 ( #26253, #10514 ),
 .UNSPECIFIED., .F., .F.,
 ( 2, 2 ),
 ( 0.000000000000000000, 1.000000000000000000 ),
 .UNSPECIFIED. ) ;
#28536 = CARTESIAN_POINT ( 'NONE',  ( -21.56784385650551528, -6.428312510596450480, 51.20221977374900035 ) ) ;
#28537 = VERTEX_POINT ( 'NONE', #44855 ) ;
#28538 = FACE_OUTER_BOUND ( 'NONE', #31955, .T. ) ;
#28539 = FACE_OUTER_BOUND ( 'NONE', #13256, .T. ) ;
#28540 = CARTESIAN_POINT ( 'NONE',  ( -14.53996353315453405, -7.939311612974331744, 60.43341030124493329 ) ) ;
#28541 = CARTESIAN_POINT ( 'NONE',  ( -10.02210521578421520, -15.65432817399831045, 61.29434977362033976 ) ) ;
#28542 = VERTEX_POINT ( 'NONE', #48279 ) ;
#28543 = DIRECTION ( 'NONE',  ( 9.009792911740839922E-08, -1.813722297350279449E-06, 0.9999999999983510968 ) ) ;
#28544 = CARTESIAN_POINT ( 'NONE',  ( -10.71238150236930053, -12.63946889494751957, 57.32857335981114488 ) ) ;
#28545 = CARTESIAN_POINT ( 'NONE',  ( -15.63470697856566005, -7.577119469675131391, 70.77136384377372735 ) ) ;
#28546 = CARTESIAN_POINT ( 'NONE',  ( -23.49747408472488885, -11.32843530181038538, 69.89210718181772108 ) ) ;
#28547 = EDGE_CURVE ( 'NONE', #16476, #29955, #32314, .T. ) ;
#28548 = DIRECTION ( 'NONE',  ( 0.3224496555704359779, 0.8691421305882571779, -0.3749909018349807388 ) ) ;
#28549 = ORIENTED_EDGE ( 'NONE', *, *, #9134, .T. ) ;
#28550 = CARTESIAN_POINT ( 'NONE',  ( 18.57590614458695200, 1.644564126066233145, 49.26952947973238395 ) ) ;
#28551 = ORIENTED_EDGE ( 'NONE', *, *, #2640, .F. ) ;
#28552 = CYLINDRICAL_SURFACE ( 'NONE', #34402, 0.1500000000000023259 ) ;
#28553 = CARTESIAN_POINT ( 'NONE',  ( -11.32087020534491018, -19.08159367390965855, 68.41678398564933161 ) ) ;
#28554 = B_SPLINE_CURVE_WITH_KNOTS ( 'NONE', 3,
 ( #47986, #33932, #14954, #40580, #7612, #37614, #14694, #22136, #37120, #22369 ),
 .UNSPECIFIED., .F., .F.,
 ( 4, 2, 2, 2, 4 ),
 ( 0.000000000000000000, 0.2500000000000000000, 0.5000000000000000000, 0.7500000000000000000, 1.000000000000000000 ),
 .UNSPECIFIED. ) ;
#28555 = EDGE_LOOP ( 'NONE', ( #47956, #46256, #8945, #22741 ) ) ;
#28556 = ADVANCED_FACE ( 'NONE', ( #22193 ), #47996, .T. ) ;
#28557 = CARTESIAN_POINT ( 'NONE',  ( -18.36938558548794376, -21.74637715204813304, 72.51340886358296700 ) ) ;
#28558 = CARTESIAN_POINT ( 'NONE',  ( -15.13034385650551528, -9.794322478646142471, 51.19202720610083190 ) ) ;
#28559 = EDGE_LOOP ( 'NONE', ( #45471, #5079 ) ) ;
#28560 = PLANE ( 'NONE',  #11079 ) ;
#28561 = CARTESIAN_POINT ( 'NONE',  ( -24.07098339466274339, -12.61366525430951313, 73.24225587970839513 ) ) ;
#28562 = CARTESIAN_POINT ( 'NONE',  ( -10.93709114749119493, -17.43956697397788602, 64.81842637974052934 ) ) ;
#28563 = ORIENTED_EDGE ( 'NONE', *, *, #3535, .F. ) ;
#28564 = DIRECTION ( 'NONE',  ( 5.255974126583346196E-06, -1.684062807769209861E-06, -0.9999999999847694054 ) ) ;
#28565 = DIRECTION ( 'NONE',  ( 0.4461977533473618363, -0.8949343913984794119, 4.927189484408733560E-16 ) ) ;
#28566 = CARTESIAN_POINT ( 'NONE',  ( -10.66022861425853563, -12.82094205862782310, 64.56836097215892778 ) ) ;
#28567 = FACE_OUTER_BOUND ( 'NONE', #11396, .T. ) ;
#28568 = CIRCLE ( 'NONE', #11279, 4.686499999999998778 ) ;
#28569 = ORIENTED_EDGE ( 'NONE', *, *, #46979, .T. ) ;
#28570 = ORIENTED_EDGE ( 'NONE', *, *, #46151, .F. ) ;
#28571 = EDGE_CURVE ( 'NONE', #31006, #17131, #29636, .T. ) ;
#28572 = DIRECTION ( 'NONE',  ( 0.9979768094191903138, 0.06357898915123796901, 0.000000000000000000 ) ) ;
#28573 = CARTESIAN_POINT ( 'NONE',  ( -24.28168432700398682, -13.15745033048042067, 66.60246978931142792 ) ) ;
#28574 = VERTEX_POINT ( 'NONE', #32 ) ;
#28575 = CARTESIAN_POINT ( 'NONE',  ( -17.63870566664756723, -7.812497183136798640, 60.18946821813101877 ) ) ;
#28576 = CARTESIAN_POINT ( 'NONE',  ( -19.46159385759798965, -7.228003583438117552, 51.38655588711986155 ) ) ;
#28577 = EDGE_CURVE ( 'NONE', #10912, #14795, #15263, .T. ) ;
#28578 = CARTESIAN_POINT ( 'NONE',  ( -26.42409385541305511, -6.859206544744110623, 63.99999999999998579 ) ) ;
#28579 =( BOUNDED_CURVE ( )  B_SPLINE_CURVE ( 2, ( #17360, #2351, #3067, #32402, #40995, #43982, #48368, #32854, #47422 ),
 .UNSPECIFIED., .F., .F. ) 
 B_SPLINE_CURVE_WITH_KNOTS ( ( 3, 2, 2, 2, 3 ),
 ( 0.04166666666666656027, 0.05208333333333329401, 0.06250000000000002776, 0.07291666666666676844, 0.08333333333333348136 ),
 .UNSPECIFIED. ) 
 CURVE ( )  GEOMETRIC_REPRESENTATION_ITEM ( )  RATIONAL_B_SPLINE_CURVE ( ( 1.000000000000000666, 0.9238795325112859613, 1.000000000000000000, 0.9238795325112867385, 1.000000000000000000, 0.9238795325112867385, 1.000000000000000000, 0.9238795325112856283, 1.000000000000001110 ) ) 
 REPRESENTATION_ITEM ( '' )  );
#28580 = FACE_OUTER_BOUND ( 'NONE', #10778, .T. ) ;
#28581 = DIRECTION ( 'NONE',  ( 1.224646799147353207E-16, 1.000000000000000000, -1.912410701131276611E-32 ) ) ;
#28582 = ORIENTED_EDGE ( 'NONE', *, *, #33737, .T. ) ;
#28583 = CARTESIAN_POINT ( 'NONE',  ( -20.88147674714181079, -8.209942860146695054, 60.02620543942160225 ) ) ;
#28584 = CARTESIAN_POINT ( 'NONE',  ( -22.88419684932020459, -10.42887832691348926, 63.37185995611467604 ) ) ;
#28585 = DIRECTION ( 'NONE',  ( -0.9477661110324759886, 0.3189661404888856633, -2.738326504218743831E-08 ) ) ;
#28586 = CYLINDRICAL_SURFACE ( 'NONE', #48117, 4.686499999999997002 ) ;
#28587 = ADVANCED_FACE ( 'NONE', ( #15997 ), #7921, .T. ) ;
#28588 =( BOUNDED_CURVE ( )  B_SPLINE_CURVE ( 3, ( #48379, #14139, #3329, #18331 ),
 .UNSPECIFIED., .F., .F. ) 
 B_SPLINE_CURVE_WITH_KNOTS ( ( 4, 4 ),
 ( 0.4074455897393634562, 0.5000000000000000000 ),
 .UNSPECIFIED. ) 
 CURVE ( )  GEOMETRIC_REPRESENTATION_ITEM ( )  RATIONAL_B_SPLINE_CURVE ( ( 0.6983129098260888457, 0.7760317562607014219, 0.8765941196520070644, 1.000000000000010880 ) ) 
 REPRESENTATION_ITEM ( '' )  );
#28589 = EDGE_LOOP ( 'NONE', ( #43879, #17135, #23308, #34724, #19508 ) ) ;
#28590 = ORIENTED_EDGE ( 'NONE', *, *, #12402, .F. ) ;
#28591 = PRODUCT_RELATED_PRODUCT_CATEGORY ( 'part', '', ( #45689 ) ) ;
#28592 = LINE ( 'NONE', #35479, #20931 ) ;
#28593 = LINE ( 'NONE', #41357, #40985 ) ;
#28594 = CARTESIAN_POINT ( 'NONE',  ( -23.88504970037045894, -11.09961929988695317, 70.03064220926479777 ) ) ;
#28595 = EDGE_LOOP ( 'NONE', ( #38122, #23948, #28331, #24908, #27431 ) ) ;
#28596 = DIRECTION ( 'NONE',  ( -3.071710424422018668E-17, 6.404604876783312462E-16, 1.000000000000000000 ) ) ;
#28597 = CARTESIAN_POINT ( 'NONE',  ( -21.33694788700791278, -9.004934622526002741, 73.60128753634342047 ) ) ;
#28598 = AXIS2_PLACEMENT_3D ( 'NONE', #41937, #19278, #15564 ) ;
#28599 = ORIENTED_EDGE ( 'NONE', *, *, #37736, .T. ) ;
#28600 = CARTESIAN_POINT ( 'NONE',  ( -10.99655682251556144, -18.57624055219563175, 57.99209882808910521 ) ) ;
#28601 = CARTESIAN_POINT ( 'NONE',  ( -20.25191534917340874, -8.350868906188830820, 70.26572394742477456 ) ) ;
#28602 = CARTESIAN_POINT ( 'NONE',  ( -21.96131106250977538, -8.900057530352752266, 66.78433116505721046 ) ) ;
#28603 = EDGE_CURVE ( 'NONE', #26904, #9441, #19083, .T. ) ;
#28604 = ORIENTED_EDGE ( 'NONE', *, *, #4646, .T. ) ;
#28605 = CARTESIAN_POINT ( 'NONE',  ( -42.54541738482483026, -14.80920654474410547, 62.02941176470587692 ) ) ;
#28606 = VERTEX_POINT ( 'NONE', #38406 ) ;
#28607 = CARTESIAN_POINT ( 'NONE',  ( -15.95864454847012581, -7.504678945485328434, 63.71365074502104875 ) ) ;
#28608 = FACE_OUTER_BOUND ( 'NONE', #29694, .T. ) ;
#28609 = ORIENTED_EDGE ( 'NONE', *, *, #45906, .F. ) ;
#28610 = CARTESIAN_POINT ( 'NONE',  ( -24.14381533474600161, -18.02640322225578373, 59.14345041050133034 ) ) ;
#28611 = CARTESIAN_POINT ( 'NONE',  ( -20.18007907243378796, -21.73087789737553166, 72.54332250421934702 ) ) ;
#28612 = PLANE ( 'NONE',  #13174 ) ;
#28613 = CARTESIAN_POINT ( 'NONE',  ( -13.66248663715553846, -8.905660726476867239, 57.26967804941948970 ) ) ;
#28614 = CARTESIAN_POINT ( 'NONE',  ( -18.68070144837527735, -7.415226739706411330, 53.49999999999994316 ) ) ;
#28615 = DIRECTION ( 'NONE',  ( -4.267285103686820140E-17, 1.935130192142698731E-16, 1.000000000000000000 ) ) ;
#28616 = ORIENTED_EDGE ( 'NONE', *, *, #38727, .F. ) ;
#28617 = DIRECTION ( 'NONE',  ( -3.071710424422018668E-17, 6.404604876783312462E-16, 1.000000000000000000 ) ) ;
#28618 = CARTESIAN_POINT ( 'NONE',  ( -11.97490362423377164, -10.33561459433851404, 67.78424783647008667 ) ) ;
#28619 = CARTESIAN_POINT ( 'NONE',  ( -24.86646048052525515, -14.46934500410477753, 66.36105466539692088 ) ) ;
#28620 = FACE_OUTER_BOUND ( 'NONE', #44382, .T. ) ;
#28621 = CARTESIAN_POINT ( 'NONE',  ( -14.11399872369470998, -20.97726832089501059, 71.92607667771569879 ) ) ;
#28622 = CARTESIAN_POINT ( 'NONE',  ( -13.13034385650551883, -9.794322478646142471, 51.19202720610083190 ) ) ;
#28623 = ORIENTED_EDGE ( 'NONE', *, *, #29153, .T. ) ;
#28624 = EDGE_LOOP ( 'NONE', ( #31639, #8420, #1994, #6038, #31169 ) ) ;
#28625 = EDGE_CURVE ( 'NONE', #16073, #7976, #20505, .T. ) ;
#28626 = CARTESIAN_POINT ( 'NONE',  ( -21.66599004997299360, -9.178097848147587001, 66.96149970124221795 ) ) ;
#28627 = DIRECTION ( 'NONE',  ( -4.115385489419834812E-17, -0.9999954153791273948, -0.003028072113822188795 ) ) ;
#28628 = ORIENTED_EDGE ( 'NONE', *, *, #26894, .T. ) ;
#28629 = CARTESIAN_POINT ( 'NONE',  ( -23.48622163778175675, -11.20987317961282237, 73.36753114030383927 ) ) ;
#28631 = CARTESIAN_POINT ( 'NONE',  ( -20.98629261354270170, -17.87291272402722697, 49.52966884056655772 ) ) ;
#28630 = CARTESIAN_POINT ( 'NONE',  ( -10.62449938266763638, -13.14622274244411315, 67.84718309729213104 ) ) ;
#28632 = CARTESIAN_POINT ( 'NONE',  ( -17.97823402885549271, -22.23862238050489992, 62.06810083693206792 ) ) ;
#28633 = CARTESIAN_POINT ( 'NONE',  ( -12.18719842096713180, -10.08886484896570934, 64.04386393395434141 ) ) ;
#28634 = ADVANCED_FACE ( 'NONE', ( #26366 ), #4694, .T. ) ;
#28635 = CARTESIAN_POINT ( 'NONE',  ( -6.424093855413058662, -6.859206544744110623, 54.49999999999999289 ) ) ;
#28636 = EDGE_LOOP ( 'NONE', ( #1871, #10438 ) ) ;
#28637 = DIRECTION ( 'NONE',  ( -2.866981220435666553E-17, 1.000000000000000000, 1.190614954331866791E-16 ) ) ;
#28638 = DIRECTION ( 'NONE',  ( 2.161108583753623267E-06, 4.147204431722191678E-06, 0.9999999999890650804 ) ) ;
#28639 = ADVANCED_FACE ( 'NONE', ( #7674 ), #3718, .F. ) ;
#28640 = CARTESIAN_POINT ( 'NONE',  ( -33.52409385541305653, -25.10920654474410441, 48.79999999999998295 ) ) ;
#28641 = VERTEX_POINT ( 'NONE', #37680 ) ;
#28642 = AXIS2_PLACEMENT_3D ( 'NONE', #6753, #14828, #3533 ) ;
#28643 = CARTESIAN_POINT ( 'NONE',  ( -17.72419709140651278, -21.80277058947482516, 58.70553378253836030 ) ) ;
#28644 = EDGE_CURVE ( 'NONE', #37610, #566, #30762, .T. ) ;
#28645 = PLANE ( 'NONE',  #12244 ) ;
#28646 = CARTESIAN_POINT ( 'NONE',  ( -24.16627971075339332, -12.73851560842801867, 66.18757903754330130 ) ) ;
#28647 = DIRECTION ( 'NONE',  ( 2.866981220435666553E-17, -1.000000000000000000, -1.190614954331866791E-16 ) ) ;
#28648 = CARTESIAN_POINT ( 'NONE',  ( -11.54449245800164903, -11.00967784149594308, 57.49286716219851456 ) ) ;
#28649 = ORIENTED_EDGE ( 'NONE', *, *, #37769, .T. ) ;
#28650 = VERTEX_POINT ( 'NONE', #45338 ) ;
#28651 = CARTESIAN_POINT ( 'NONE',  ( -19.20534385541304090, -7.595227055684746986, 51.75156210489594599 ) ) ;
#28652 = CARTESIAN_POINT ( 'NONE',  ( -8.258083856565255232, -9.811588921218147519, 54.49999999999995026 ) ) ;
#28653 = CARTESIAN_POINT ( 'NONE',  ( -11.97490362423377164, -10.33561459433851404, 67.78424783647008667 ) ) ;
#28654 = EDGE_CURVE ( 'NONE', #39949, #42734, #30811, .T. ) ;
#28655 = EDGE_CURVE ( 'NONE', #24440, #43669, #4977, .T. ) ;
#28656 = CARTESIAN_POINT ( 'NONE',  ( -14.27319502748954783, -8.558459675072437989, 70.72957628730870283 ) ) ;
#28657 = CARTESIAN_POINT ( 'NONE',  ( -50.42609385541305755, -14.90920654474414775, 61.02352941176469869 ) ) ;
#28658 = ORIENTED_EDGE ( 'NONE', *, *, #13969, .T. ) ;
#28659 = CARTESIAN_POINT ( 'NONE',  ( -14.48548941065489970, -8.400516866317895293, 67.27447142263336843 ) ) ;
#28660 = CARTESIAN_POINT ( 'NONE',  ( -21.12749503816145591, -21.27438112535048376, 62.22816062766979428 ) ) ;
#28661 = ORIENTED_EDGE ( 'NONE', *, *, #28710, .T. ) ;
#28662 = DIRECTION ( 'NONE',  ( 0.1539336739619741601, 0.9880811829098680166, 6.607022902453645889E-08 ) ) ;
#28663 = EDGE_CURVE ( 'NONE', #41284, #24527, #27903, .T. ) ;
#28664 = LINE ( 'NONE', #42953, #4679 ) ;
#28665 = CIRCLE ( 'NONE', #22367, 2.000000000000001776 ) ;
#28666 = VERTEX_POINT ( 'NONE', #20191 ) ;
#28667 = CARTESIAN_POINT ( 'NONE',  ( -14.38502091232239621, -11.22596901536237013, 49.52966884056655772 ) ) ;
#28668 = CARTESIAN_POINT ( 'NONE',  ( -12.26902398874117495, -19.54473763108856943, 58.22682373989366766 ) ) ;
#28669 = ORIENTED_EDGE ( 'NONE', *, *, #24132, .F. ) ;
#28670 = CARTESIAN_POINT ( 'NONE',  ( -13.93897074462874919, -20.93787812888889377, 68.74153005185598886 ) ) ;
#28671 = CIRCLE ( 'NONE', #37284, 0.5000000000000004441 ) ;
#28672 = CARTESIAN_POINT ( 'NONE',  ( -22.41668094288463919, -16.43295965837073780, 50.77966884056655772 ) ) ;
#28673 = DIRECTION ( 'NONE',  ( -3.071710424422018668E-17, 6.404604876783312462E-16, 1.000000000000000000 ) ) ;
#28674 = CARTESIAN_POINT ( 'NONE',  ( -24.69675289721077505, -13.19280437224551505, 59.48455129494911375 ) ) ;
#28675 = ORIENTED_EDGE ( 'NONE', *, *, #17632, .F. ) ;
#28676 = DIRECTION ( 'NONE',  ( -0.8547111024021492032, -0.5191039697695418731, -7.472447831848563370E-08 ) ) ;
#28677 = CARTESIAN_POINT ( 'NONE',  ( -19.74200936563729769, -21.46758226568296024, 68.94954551542706156 ) ) ;
#28678 = DIRECTION ( 'NONE',  ( 1.000000000000000000, 0.000000000000000000, 0.000000000000000000 ) ) ;
#28679 = FACE_OUTER_BOUND ( 'NONE', #29895, .T. ) ;
#28680 = CARTESIAN_POINT ( 'NONE',  ( -23.19948571119275726, -18.85291137746749968, 65.83861571032234394 ) ) ;
#28681 = ORIENTED_EDGE ( 'NONE', *, *, #16145, .T. ) ;
#28682 = CARTESIAN_POINT ( 'NONE',  ( -23.57909424710215518, -11.36400449684228775, 73.45373529196413642 ) ) ;
#28683 = CARTESIAN_POINT ( 'NONE',  ( -18.53289088300742193, -21.77150771217549874, 72.58510914717624019 ) ) ;
#28684 = CARTESIAN_POINT ( 'NONE',  ( -13.29033951192469587, -20.46027514905393119, 58.23577251623645878 ) ) ;
#28685 = VERTEX_POINT ( 'NONE', #32005 ) ;
#28686 = CARTESIAN_POINT ( 'NONE',  ( -12.27729936708703384, -9.991218733798060470, 60.70918086709614414 ) ) ;
#28687 = ADVANCED_FACE ( 'NONE', ( #8883 ), #27339, .T. ) ;
#28688 = VERTEX_POINT ( 'NONE', #24385 ) ;
#28689 = ORIENTED_EDGE ( 'NONE', *, *, #41055, .F. ) ;
#28690 = VERTEX_POINT ( 'NONE', #2202 ) ;
#28691 = ADVANCED_FACE ( 'NONE', ( #27824 ), #27291, .T. ) ;
#28692 = DIRECTION ( 'NONE',  ( -0.3478314405900309048, -0.9375570856950864451, 0.000000000000000000 ) ) ;
#28693 = DIRECTION ( 'NONE',  ( 1.000000000000000000, -4.164305804376849172E-17, 1.614929280266638808E-16 ) ) ;
#28694 = DIRECTION ( 'NONE',  ( 1.000000000000000000, 2.866981220435666553E-17, 0.000000000000000000 ) ) ;
#28695 = CARTESIAN_POINT ( 'NONE',  ( -12.63116919492461854, -9.104687665260810192, 70.96270001146038453 ) ) ;
#28696 = ORIENTED_EDGE ( 'NONE', *, *, #26794, .F. ) ;
#28697 = ORIENTED_EDGE ( 'NONE', *, *, #26662, .F. ) ;
#28698 = AXIS2_PLACEMENT_3D ( 'NONE', #44891, #37455, #34753 ) ;
#28699 = CARTESIAN_POINT ( 'NONE',  ( -17.54909385650551812, -8.104110260919579645, 48.81699501597546487 ) ) ;
#28700 = AXIS2_PLACEMENT_3D ( 'NONE', #38832, #27027, #12734 ) ;
#28701 = CARTESIAN_POINT ( 'NONE',  ( -24.87414375265050026, -14.81611830904748395, 59.43574407478276100 ) ) ;
#28702 = CARTESIAN_POINT ( 'NONE',  ( -24.07500963186500798, -16.99236413854744399, 73.16870702396911952 ) ) ;
#28703 =( BOUNDED_CURVE ( )  B_SPLINE_CURVE ( 3, ( #18748, #11368, #14779, #25901 ),
 .UNSPECIFIED., .F., .F. ) 
 B_SPLINE_CURVE_WITH_KNOTS ( ( 4, 4 ),
 ( 0.5000000000000000000, 0.9074455897393651771 ),
 .UNSPECIFIED. ) 
 CURVE ( )  GEOMETRIC_REPRESENTATION_ITEM ( )  RATIONAL_B_SPLINE_CURVE ( ( 0.9999999999999938938, 0.4567392136813211989, 0.3561768502900304334, 0.6983129098261150469 ) ) 
 REPRESENTATION_ITEM ( '' )  );
#28705 = EDGE_CURVE ( 'NONE', #16629, #29740, #35762, .T. ) ;
#28704 = CARTESIAN_POINT ( 'NONE',  ( -17.26784385650551457, -6.428312510596451368, 51.20221977374900035 ) ) ;
#28706 = EDGE_CURVE ( 'NONE', #10157, #3333, #7467, .T. ) ;
#28707 = VERTEX_POINT ( 'NONE', #43344 ) ;
#28708 = EDGE_CURVE ( 'NONE', #6216, #42831, #31275, .T. ) ;
#28709 = EDGE_CURVE ( 'NONE', #3895, #2100, #15769, .T. ) ;
#28710 = EDGE_CURVE ( 'NONE', #6805, #43621, #7758, .T. ) ;
#28711 = FACE_OUTER_BOUND ( 'NONE', #48174, .T. ) ;
#28712 = DIRECTION ( 'NONE',  ( -3.413470714839332458E-33, 1.190614954331866791E-16, -1.000000000000000000 ) ) ;
#28713 = ORIENTED_EDGE ( 'NONE', *, *, #1013, .F. ) ;
#28714 =( BOUNDED_SURFACE ( )  B_SPLINE_SURFACE ( 3, 1, ( 
 ( #4558, #19580 ),
 ( #29687, #44722 ),
 ( #3519, #22001 ),
 ( #33058, #36743 ),
 ( #48101, #14567 ),
 ( #25939, #14332 ),
 ( #29390, #44422 ) ),
 .UNSPECIFIED., .T., .F., .F. ) 
 B_SPLINE_SURFACE_WITH_KNOTS ( ( 4, 3, 4 ),
 ( 2, 2 ),
 ( 0.000000000000000000, 0.5000000000000000000, 1.000000000000000000 ),
 ( 0.000000000000000000, 1.000000000000000000 ),
 .UNSPECIFIED. ) 
 GEOMETRIC_REPRESENTATION_ITEM ( )  RATIONAL_B_SPLINE_SURFACE ( (
 ( 1.000000000000000000, 1.000000000000000000),
 ( 0.3333333333333335369, 0.3333333333333330373),
 ( 0.3333333333333335369, 0.3333333333333330373),
 ( 1.000000000000000000, 1.000000000000000000),
 ( 0.3333333333333333703, 0.3333333333333333703),
 ( 0.3333333333333333703, 0.3333333333333333703),
 ( 1.000000000000000000, 1.000000000000000000) ) ) 
 REPRESENTATION_ITEM ( '' )  SURFACE ( )  );
#28715 = CARTESIAN_POINT ( 'NONE',  ( -12.67665486305926237, -12.56770637434968307, 50.77966884056655772 ) ) ;
#28716 =( BOUNDED_SURFACE ( )  B_SPLINE_SURFACE ( 3, 1, ( 
 ( #4802, #39501 ),
 ( #35308, #8984 ),
 ( #46159, #27442 ),
 ( #20785, #19826 ),
 ( #34824, #24007 ),
 ( #39009, #20561 ),
 ( #1584, #16593 ) ),
 .UNSPECIFIED., .T., .F., .F. ) 
 B_SPLINE_SURFACE_WITH_KNOTS ( ( 4, 3, 4 ),
 ( 2, 2 ),
 ( 0.000000000000000000, 0.5000000000000000000, 1.000000000000000000 ),
 ( 0.000000000000000000, 1.000000000000000000 ),
 .UNSPECIFIED. ) 
 GEOMETRIC_REPRESENTATION_ITEM ( )  RATIONAL_B_SPLINE_SURFACE ( (
 ( 1.000000000000000000, 1.000000000000000000),
 ( 0.3333333333333335369, 0.3333333333333330373),
 ( 0.3333333333333335369, 0.3333333333333330373),
 ( 1.000000000000000000, 1.000000000000000000),
 ( 0.3333333333333333703, 0.3333333333333333703),
 ( 0.3333333333333333703, 0.3333333333333333703),
 ( 1.000000000000000000, 1.000000000000000000) ) ) 
 REPRESENTATION_ITEM ( '' )  SURFACE ( )  );
#28717 = ORIENTED_EDGE ( 'NONE', *, *, #5059, .T. ) ;
#28718 = LINE ( 'NONE', #10496, #33921 ) ;
#28719 = DIRECTION ( 'NONE',  ( 0.000000000000000000, 0.000000000000000000, 1.000000000000000000 ) ) ;
#28720 = FACE_OUTER_BOUND ( 'NONE', #15692, .T. ) ;
#28721 = ORIENTED_EDGE ( 'NONE', *, *, #47908, .F. ) ;
#28722 = CARTESIAN_POINT ( 'NONE',  ( -20.83700022493355775, -19.12221826660256951, 53.49899999999994549 ) ) ;
#28723 = CARTESIAN_POINT ( 'NONE',  ( -16.95534385541304445, -8.623186033802570094, 49.24843789510465797 ) ) ;
#28724 = DIRECTION ( 'NONE',  ( 1.061592182633803142E-06, 3.103086874681752273E-06, -0.9999999999946220797 ) ) ;
#28725 = ORIENTED_EDGE ( 'NONE', *, *, #5717, .F. ) ;
#28726 = CARTESIAN_POINT ( 'NONE',  ( -20.68076794159699006, -21.00564031164944012, 58.94475149674252634 ) ) ;
#28728 =( BOUNDED_CURVE ( )  B_SPLINE_CURVE ( 3, ( #44663, #10923, #18790, #7244 ),
 .UNSPECIFIED., .F., .F. ) 
 B_SPLINE_CURVE_WITH_KNOTS ( ( 4, 4 ),
 ( 0.000000000000000000, 0.4074455897393655657 ),
 .UNSPECIFIED. ) 
 CURVE ( )  GEOMETRIC_REPRESENTATION_ITEM ( )  RATIONAL_B_SPLINE_CURVE ( ( 1.000000000000000000, 0.4567392136813335224, 0.3561768502900308775, 0.6983129098260920653 ) ) 
 REPRESENTATION_ITEM ( '' )  );
#28727 = CARTESIAN_POINT ( 'NONE',  ( -24.44689184067228638, -14.18710713894228093, 69.93803194250310185 ) ) ;
#28729 = ORIENTED_EDGE ( 'NONE', *, *, #18725, .T. ) ;
#28730 = CIRCLE ( 'NONE', #14518, 0.3999999999999975797 ) ;
#28731 = CARTESIAN_POINT ( 'NONE',  ( -24.72409385541305582, -14.90920654474420104, 66.05294117647058272 ) ) ;
#28732 = CARTESIAN_POINT ( 'NONE',  ( -9.975073501874963000, -14.93475060744560245, 74.84132960708070925 ) ) ;
#28733 = VERTEX_POINT ( 'NONE', #13032 ) ;
#28734 = DIRECTION ( 'NONE',  ( -3.071710424422018668E-17, 6.404604876783312462E-16, 1.000000000000000000 ) ) ;
#28736 = EDGE_CURVE ( 'NONE', #33229, #1420, #3414, .T. ) ;
#28735 = DIRECTION ( 'NONE',  ( -0.8083598999316398137, -0.5886886037477750966, -6.671815824719443556E-08 ) ) ;
#28737 = AXIS2_PLACEMENT_3D ( 'NONE', #31412, #17351, #17099 ) ;
#28738 = CARTESIAN_POINT ( 'NONE',  ( -16.66933960180709917, -7.791706125978248743, 74.11585391104840426 ) ) ;
#28739 = DIRECTION ( 'NONE',  ( 0.000000000000000000, 0.000000000000000000, 1.000000000000000000 ) ) ;
#28740 = ORIENTED_EDGE ( 'NONE', *, *, #38303, .T. ) ;
#28741 = CARTESIAN_POINT ( 'NONE',  ( -22.07364850117675914, -9.574309989343213090, 59.91098251635671801 ) ) ;
#28742 = CARTESIAN_POINT ( 'NONE',  ( -11.09714801257800865, -11.68115280588511773, 64.30448977214732054 ) ) ;
#28743 = CARTESIAN_POINT ( 'NONE',  ( -41.55245041649903470, -14.90920654474425433, 69.97314751131220589 ) ) ;
#28744 = ORIENTED_EDGE ( 'NONE', *, *, #31582, .T. ) ;
#28745 = CARTESIAN_POINT ( 'NONE',  ( -11.19061673737954088, -18.88921303226083737, 64.84732837536805050 ) ) ;
#28746 = CARTESIAN_POINT ( 'NONE',  ( -24.77723895724858494, -16.00713575449774595, 66.24820309305337673 ) ) ;
#28747 = ORIENTED_EDGE ( 'NONE', *, *, #7460, .F. ) ;
#28748 = VERTEX_POINT ( 'NONE', #32945 ) ;
#28749 = CARTESIAN_POINT ( 'NONE',  ( -20.46382095854371030, -21.17433842136345490, 58.94475249639827297 ) ) ;
#28750 = CARTESIAN_POINT ( 'NONE',  ( -13.85276489020729507, -20.89200646248024995, 72.22607902822389292 ) ) ;
#28751 = CARTESIAN_POINT ( 'NONE',  ( -10.02945380498330508, -15.71617353208280221, 61.23063189029311104 ) ) ;
#28752 = B_SPLINE_CURVE_WITH_KNOTS ( 'NONE', 1,
 ( #17293, #48068 ),
 .UNSPECIFIED., .F., .F.,
 ( 2, 2 ),
 ( 0.000000000000000000, 1.000000000000000000 ),
 .UNSPECIFIED. ) ;
#28753 = CARTESIAN_POINT ( 'NONE',  ( -13.11945872550529835, -9.225962324091906197, 67.67942785705487552 ) ) ;
#28754 = DIRECTION ( 'NONE',  ( -1.590463988637600692E-07, 3.579926724016472968E-07, -0.9999999999999232836 ) ) ;
#28755 = CARTESIAN_POINT ( 'NONE',  ( -14.80624636014071172, -8.317144122717282428, 60.61996281969079803 ) ) ;
#28756 = CARTESIAN_POINT ( 'NONE',  ( -13.04354001453261525, -9.349206015805425096, 67.60616047355428293 ) ) ;
#28757 = CARTESIAN_POINT ( 'NONE',  ( -14.77871938317573353, -21.77373431923335190, 61.73576822224330130 ) ) ;
#28758 = CARTESIAN_POINT ( 'NONE',  ( -24.72409385541305582, -14.80920654474411613, 58.00588235294116402 ) ) ;
#28759 = ORIENTED_EDGE ( 'NONE', *, *, #9071, .F. ) ;
#28760 = VERTEX_POINT ( 'NONE', #36885 ) ;
#28761 = CARTESIAN_POINT ( 'NONE',  ( -13.38575581802539993, -9.030060914960570173, 60.72478133471773276 ) ) ;
#28762 = CARTESIAN_POINT ( 'NONE',  ( -23.07453839662878181, -9.953611553617093932, 66.66369493676361913 ) ) ;
#28763 = CARTESIAN_POINT ( 'NONE',  ( -16.01712585257974908, -7.950755256560901429, 67.21177652078760900 ) ) ;
#28764 = CYLINDRICAL_SURFACE ( 'NONE', #4409, 1.250000000000001110 ) ;
#28765 = CYLINDRICAL_SURFACE ( 'NONE', #80, 5.249999999999998224 ) ;
#28766 = CARTESIAN_POINT ( 'NONE',  ( -20.94909385650551670, -8.104110260919577868, 48.81699501597546487 ) ) ;
#28767 = AXIS2_PLACEMENT_3D ( 'NONE', #47767, #2941, #47539 ) ;
#28768 = EDGE_LOOP ( 'NONE', ( #37346, #25286, #22722, #11758, #47632 ) ) ;
#28769 = EDGE_CURVE ( 'NONE', #30155, #10544, #2451, .T. ) ;
#28770 = EDGE_CURVE ( 'NONE', #35620, #44349, #28378, .T. ) ;
#28771 = CARTESIAN_POINT ( 'NONE',  ( -14.97035482569482312, -21.41873484682592377, 61.92128389535452015 ) ) ;
#28772 = FILL_AREA_STYLE_COLOUR ( '', #13482 ) ;
#28773 = CARTESIAN_POINT ( 'NONE',  ( -16.45566506110110438, -21.79267588865899086, 62.04095995016087528 ) ) ;
#28774 = CARTESIAN_POINT ( 'NONE',  ( -10.53876648713876740, -16.36073154998923229, 68.13334680848100788 ) ) ;
#28775 = ORIENTED_EDGE ( 'NONE', *, *, #7, .T. ) ;
#28776 = EDGE_CURVE ( 'NONE', #12811, #12076, #36635, .T. ) ;
#28777 = ADVANCED_FACE ( 'NONE', ( #43831 ), #28560, .T. ) ;
#28778 = CARTESIAN_POINT ( 'NONE',  ( -41.30129973776600139, -14.80920654474425291, 71.98235294117645822 ) ) ;
#28779 = CARTESIAN_POINT ( 'NONE',  ( -19.98473524480838748, -8.236797504970272854, 70.45920369457601851 ) ) ;
#28780 = FACE_OUTER_BOUND ( 'NONE', #38735, .T. ) ;
#28781 = DIRECTION ( 'NONE',  ( 7.110378527815250859E-06, 9.728165319648377852E-06, -0.9999999999274026274 ) ) ;
#28782 = EDGE_LOOP ( 'NONE', ( #14664, #27475 ) ) ;
#28783 = CARTESIAN_POINT ( 'NONE',  ( -20.98579777188748707, -20.83533835786949950, 65.58453944793343737 ) ) ;
#28784 = EDGE_LOOP ( 'NONE', ( #35657, #40264 ) ) ;
#28785 = CYLINDRICAL_SURFACE ( 'NONE', #21837, 1.999999999999994893 ) ;
#28786 = CARTESIAN_POINT ( 'NONE',  ( -19.23357275453091830, -7.582241477678771879, 63.62427554819404207 ) ) ;
#28787 = EDGE_LOOP ( 'NONE', ( #41181, #9452, #43438, #28280, #47765 ) ) ;
#28788 = CARTESIAN_POINT ( 'NONE',  ( -18.46282339125754746, -21.73182043318683299, 72.58510983671801853 ) ) ;
#28789 = EDGE_CURVE ( 'NONE', #44272, #19285, #38588, .T. ) ;
#28790 = CARTESIAN_POINT ( 'NONE',  ( -14.45534385650551989, -7.417179338643134834, 52.18511593390279302 ) ) ;
#28791 = ORIENTED_EDGE ( 'NONE', *, *, #4562, .T. ) ;
#28792 = CARTESIAN_POINT ( 'NONE',  ( -14.21171452256333012, -10.65672306833167937, 50.77966884056655772 ) ) ;
#28793 = DIRECTION ( 'NONE',  ( 1.000000000000000000, 2.866981220435666553E-17, 0.000000000000000000 ) ) ;
#28794 = CARTESIAN_POINT ( 'NONE',  ( -21.62392673332162119, -8.655692864502302797, 73.77941542331133462 ) ) ;
#28795 = ORIENTED_EDGE ( 'NONE', *, *, #40561, .F. ) ;
#28796 = CARTESIAN_POINT ( 'NONE',  ( -13.34712228287558844, -20.56097989973784834, 58.05209898279497338 ) ) ;
#28797 = CIRCLE ( 'NONE', #41371, 2.500000000000002220 ) ;
#28798 = DIRECTION ( 'NONE',  ( -3.071710424422018668E-17, 6.404604876783312462E-16, 1.000000000000000000 ) ) ;
#28799 = AXIS2_PLACEMENT_3D ( 'NONE', #44287, #47489, #6839 ) ;
#28800 = B_SPLINE_CURVE_WITH_KNOTS ( 'NONE', 3,
 ( #12039, #27055, #42079, #27539, #19418, #4178, #26825, #15461, #12274, #31235 ),
 .UNSPECIFIED., .F., .F.,
 ( 4, 2, 2, 2, 4 ),
 ( 0.6272669072783476629, 0.7522669073002239415, 0.8772669073221003311, 1.002266907343976721, 1.127266907365852999 ),
 .UNSPECIFIED. ) ;
#28801 = DIRECTION ( 'NONE',  ( -0.1571515419521612722, 0.9875744999047173511, -7.433889655140016607E-08 ) ) ;
#28802 = FACE_OUTER_BOUND ( 'NONE', #47519, .T. ) ;
#28803 = ORIENTED_EDGE ( 'NONE', *, *, #46637, .T. ) ;
#28804 = ORIENTED_EDGE ( 'NONE', *, *, #34501, .T. ) ;
#28805 = CARTESIAN_POINT ( 'NONE',  ( -11.76184414918852106, -18.92500367160094044, 68.44362863376011319 ) ) ;
#28806 = CARTESIAN_POINT ( 'NONE',  ( -10.97862690519434459, -18.54530816898288492, 57.95714592071885107 ) ) ;
#28807 = VERTEX_POINT ( 'NONE', #2917 ) ;
#28808 = CARTESIAN_POINT ( 'NONE',  ( -20.71686288416324118, -8.126370072314889725, 63.51110291890488213 ) ) ;
#28809 =( BOUNDED_CURVE ( )  B_SPLINE_CURVE ( 3, ( #8142, #8624, #27803, #23886 ),
 .UNSPECIFIED., .F., .F. ) 
 B_SPLINE_CURVE_WITH_KNOTS ( ( 4, 4 ),
 ( 0.4074455897393700621, 0.5000000000000000000 ),
 .UNSPECIFIED. ) 
 CURVE ( )  GEOMETRIC_REPRESENTATION_ITEM ( )  RATIONAL_B_SPLINE_CURVE ( ( 0.6983129098261103840, 0.7760317562607019770, 0.8765941196519950740, 0.9999999999999821254 ) ) 
 REPRESENTATION_ITEM ( '' )  );
#28810 = CARTESIAN_POINT ( 'NONE',  ( -19.34909385759798894, -8.112991634885936776, 51.74999426922421719 ) ) ;
#28811 = CARTESIAN_POINT ( 'NONE',  ( -24.15165104652898620, -11.60707627830156952, 63.13873557927141889 ) ) ;
#28812 = DIRECTION ( 'NONE',  ( 1.000000000000000000, 1.669677910507523057E-21, 6.493791346278465266E-22 ) ) ;
#28813 = CARTESIAN_POINT ( 'NONE',  ( -23.70015292207183322, -18.82353835121273988, 69.47867366044893345 ) ) ;
#28814 = ORIENTED_EDGE ( 'NONE', *, *, #2508, .F. ) ;
#28815 = DIRECTION ( 'NONE',  ( -3.549360974551883545E-17, 6.371834667872732552E-18, 1.000000000000000000 ) ) ;
#28816 = FACE_OUTER_BOUND ( 'NONE', #37474, .T. ) ;
#28817 = LINE ( 'NONE', #40152, #34764 ) ;
#28818 = ORIENTED_EDGE ( 'NONE', *, *, #13541, .F. ) ;
#28819 = ORIENTED_EDGE ( 'NONE', *, *, #2373, .F. ) ;
#28820 = EDGE_CURVE ( 'NONE', #6217, #37990, #7337, .T. ) ;
#28821 = CARTESIAN_POINT ( 'NONE',  ( -10.86332161679245445, -12.36740429957887955, 57.61240734327432733 ) ) ;
#28822 = SURFACE_SIDE_STYLE ('',( #35714 ) ) ;
#28823 = DIRECTION ( 'NONE',  ( 0.000000000000000000, 0.000000000000000000, 1.000000000000000000 ) ) ;
#28824 = VERTEX_POINT ( 'NONE', #22143 ) ;
#28825 = DIRECTION ( 'NONE',  ( -0.9789991564298998750, -0.2038642972899922245, 4.410747590293501250E-08 ) ) ;
#28826 = EDGE_CURVE ( 'NONE', #30092, #21727, #36163, .T. ) ;
#28827 = CARTESIAN_POINT ( 'NONE',  ( -23.17409385650551457, -9.792211528768504536, 50.49490371617623197 ) ) ;
#28828 = ORIENTED_EDGE ( 'NONE', *, *, #41668, .T. ) ;
#28829 = EDGE_CURVE ( 'NONE', #27130, #383, #44923, .T. ) ;
#28830 = CARTESIAN_POINT ( 'NONE',  ( -20.72450927900464634, -21.03929139025762751, 58.93003081252663833 ) ) ;
#28831 = AXIS2_PLACEMENT_3D ( 'NONE', #18881, #8069, #26513 ) ;
#28832 = EDGE_CURVE ( 'NONE', #260, #15899, #9073, .T. ) ;
#28833 = DIRECTION ( 'NONE',  ( -2.209513405570979834E-06, 7.769005115158032304E-07, 0.9999999999972571940 ) ) ;
#28834 = ORIENTED_EDGE ( 'NONE', *, *, #11587, .T. ) ;
#28835 = CARTESIAN_POINT ( 'NONE',  ( -24.15708772167537077, -12.88964773349922410, 69.84413305346230061 ) ) ;
#28836 = ORIENTED_EDGE ( 'NONE', *, *, #42975, .T. ) ;
#28837 = B_SPLINE_CURVE_WITH_KNOTS ( 'NONE', 3,
 ( #34623, #24287, #909, #8534, #39536, #39294, #23564, #35589, #13166, #42519 ),
 .UNSPECIFIED., .F., .F.,
 ( 4, 2, 2, 2, 4 ),
 ( 0.1272669073658421190, 0.2522669073463229550, 0.3772669073268037909, 0.5022669073072846269, 0.6272669072877654628 ),
 .UNSPECIFIED. ) ;
#28838 = CARTESIAN_POINT ( 'NONE',  ( -26.22630854578367021, -13.51651355179587632, 53.49999999999995026 ) ) ;
#28839 = CARTESIAN_POINT ( 'NONE',  ( -22.29619887594318328, -17.36118473213641167, 54.07175714974878389 ) ) ;
#28840 = CARTESIAN_POINT ( 'NONE',  ( -19.22579309969192707, -21.57336792462666253, 58.52507384993226225 ) ) ;
#28841 = EDGE_LOOP ( 'NONE', ( #40527, #6751, #33492, #38674 ) ) ;
#28842 = CARTESIAN_POINT ( 'NONE',  ( -21.19385221619855386, -22.41842420181545847, 54.38277594638586976 ) ) ;
#28843 = CARTESIAN_POINT ( 'NONE',  ( -10.57136597998982985, -13.11950654315977793, 64.42403173677416817 ) ) ;
#28844 = CARTESIAN_POINT ( 'NONE',  ( -17.72634082312590920, -21.85272461445201486, 58.40553378267872375 ) ) ;
#28845 =( BOUNDED_SURFACE ( )  B_SPLINE_SURFACE ( 3, 1, ( 
 ( #26146, #18997 ),
 ( #21713, #22446 ),
 ( #37437, #33752 ),
 ( #40424, #34001 ),
 ( #15276, #15032 ),
 ( #25895, #14296 ),
 ( #30094, #45117 ) ),
 .UNSPECIFIED., .T., .F., .F. ) 
 B_SPLINE_SURFACE_WITH_KNOTS ( ( 4, 3, 4 ),
 ( 2, 2 ),
 ( 0.000000000000000000, 0.5000000000000000000, 1.000000000000000000 ),
 ( 0.000000000000000000, 1.000000000000000000 ),
 .UNSPECIFIED. ) 
 GEOMETRIC_REPRESENTATION_ITEM ( )  RATIONAL_B_SPLINE_SURFACE ( (
 ( 1.000000000000000000, 1.000000000000000000),
 ( 0.3333333333333335369, 0.3333333333333330373),
 ( 0.3333333333333335369, 0.3333333333333330373),
 ( 1.000000000000000000, 1.000000000000000000),
 ( 0.3333333333333333703, 0.3333333333333333703),
 ( 0.3333333333333333703, 0.3333333333333333703),
 ( 1.000000000000000000, 1.000000000000000000) ) ) 
 REPRESENTATION_ITEM ( '' )  SURFACE ( )  );
#28846 = CARTESIAN_POINT ( 'NONE',  ( -15.47121567594983738, -8.035039782910647688, 74.37985637822782792 ) ) ;
#28847 = CARTESIAN_POINT ( 'NONE',  ( -10.45529275995371066, -15.48619407273052495, 61.22716148030291805 ) ) ;
#28848 = CARTESIAN_POINT ( 'NONE',  ( -23.00381842360518547, -10.58230771189866104, 59.90203429537245228 ) ) ;
#28849 = ORIENTED_EDGE ( 'NONE', *, *, #32974, .T. ) ;
#28850 = CARTESIAN_POINT ( 'NONE',  ( -23.49605051889219709, -11.22618518380361152, 73.37665428612797314 ) ) ;
#28851 = CARTESIAN_POINT ( 'NONE',  ( -12.23165125622869631, -10.02867215863997608, 67.64329750964374455 ) ) ;
#28852 = DIRECTION ( 'NONE',  ( -3.071710424422018668E-17, 6.404604876783312462E-16, 1.000000000000000000 ) ) ;
#28853 = DIRECTION ( 'NONE',  ( -3.071710424422018668E-17, 6.404604876783312462E-16, 1.000000000000000000 ) ) ;
#28854 = CARTESIAN_POINT ( 'NONE',  ( -11.46043946983621709, -11.04924301243271678, 57.35903212150709152 ) ) ;
#28855 = CARTESIAN_POINT ( 'NONE',  ( -13.41159385650551528, -6.922745924619793101, 51.69366785382590024 ) ) ;
#28856 = ORIENTED_EDGE ( 'NONE', *, *, #42286, .F. ) ;
#28857 = ORIENTED_EDGE ( 'NONE', *, *, #30849, .T. ) ;
#28858 = CARTESIAN_POINT ( 'NONE',  ( -21.18836735823073525, -20.77369112572868914, 65.46965119999302374 ) ) ;
#28859 = CARTESIAN_POINT ( 'NONE',  ( -24.39416267077224987, -15.91966209353573802, 73.14736799148198543 ) ) ;
#28860 = ORIENTED_EDGE ( 'NONE', *, *, #34986, .F. ) ;
#28861 = CARTESIAN_POINT ( 'NONE',  ( -9.975583786612773451, -14.65598763567812313, 71.44287367974872893 ) ) ;
#28863 = CARTESIAN_POINT ( 'NONE',  ( -12.50766613833179974, -19.86205114983803810, 64.86674886870797252 ) ) ;
#28862 = CARTESIAN_POINT ( 'NONE',  ( -10.62433447910814976, -13.14689714368311257, 67.92935478332734078 ) ) ;
#28864 = CARTESIAN_POINT ( 'NONE',  ( -14.48970220490235228, -8.453945278547838171, 63.98082128453373940 ) ) ;
#28865 = CARTESIAN_POINT ( 'NONE',  ( -10.61357223164714902, -13.19155561173493219, 71.20828586568362084 ) ) ;
#28866 = CARTESIAN_POINT ( 'NONE',  ( -22.22492895683646807, -9.112220634607178127, 59.76525293062090327 ) ) ;
#28867 = CARTESIAN_POINT ( 'NONE',  ( -11.45752044641470668, -19.27057170535650954, 71.87181270239314301 ) ) ;
#28868 = LINE ( 'NONE', #47824, #33776 ) ;
#28869 = DIRECTION ( 'NONE',  ( -1.224646799147353207E-16, -1.000000000000000000, 1.912410701131276611E-32 ) ) ;
#28870 =( BOUNDED_CURVE ( )  B_SPLINE_CURVE ( 3, ( #27260, #20360, #2364, #47433 ),
 .UNSPECIFIED., .F., .F. ) 
 B_SPLINE_CURVE_WITH_KNOTS ( ( 4, 4 ),
 ( 0.4074455897393655657, 0.5000000000000000000 ),
 .UNSPECIFIED. ) 
 CURVE ( )  GEOMETRIC_REPRESENTATION_ITEM ( )  RATIONAL_B_SPLINE_CURVE ( ( 0.6983129098260923984, 0.7760317562606950936, 0.8765941196519969614, 0.9999999999999960032 ) ) 
 REPRESENTATION_ITEM ( '' )  );
#28871 = VECTOR ( 'NONE', #12106, 1000.000000000000000 ) ;
#28872 = CARTESIAN_POINT ( 'NONE',  ( -21.97169192525862869, -15.94174089086207147, 49.52966884056655772 ) ) ;
#28873 = CARTESIAN_POINT ( 'NONE',  ( 9.825906144586950219, -6.109215713985405749, 50.50605614422795497 ) ) ;
#28874 = VERTEX_POINT ( 'NONE', #10568 ) ;
#28875 = CARTESIAN_POINT ( 'NONE',  ( -20.75354924259569245, -21.52967727414722532, 53.49999999999994316 ) ) ;
#28876 = CARTESIAN_POINT ( 'NONE',  ( -11.54877110944083896, -18.61454263387444286, 61.38596758451725321 ) ) ;
#28877 = AXIS2_PLACEMENT_3D ( 'NONE', #39443, #2724, #28833 ) ;
#28878 = CARTESIAN_POINT ( 'NONE',  ( -21.01334446694451685, -11.79580940901521835, 49.52966884056655772 ) ) ;
#28879 = CARTESIAN_POINT ( 'NONE',  ( -24.63461978062257174, -12.93251252767717929, 66.48902111634848211 ) ) ;
#28880 = ADVANCED_FACE ( 'NONE', ( #3171 ), #25579, .T. ) ;
#28881 = CARTESIAN_POINT ( 'NONE',  ( -13.85547199604887503, -20.83131545695484732, 65.21302117645285534 ) ) ;
#28882 = CARTESIAN_POINT ( 'NONE',  ( -19.30271930833434979, -8.014115225907463724, 60.11092997145157568 ) ) ;
#28883 = ORIENTED_EDGE ( 'NONE', *, *, #19866, .T. ) ;
#28884 = VERTEX_POINT ( 'NONE', #40585 ) ;
#28885 = CARTESIAN_POINT ( 'NONE',  ( -17.74284385541304232, -7.587656875400192291, 49.25157356644813689 ) ) ;
#28886 = CARTESIAN_POINT ( 'NONE',  ( -24.72409385541305582, -14.90920654474417972, 64.04117647058822627 ) ) ;
#28887 = CARTESIAN_POINT ( 'NONE',  ( -11.97490362423377164, -10.33561459433851404, 67.78424783647008667 ) ) ;
#28888 = B_SPLINE_CURVE_WITH_KNOTS ( 'NONE', 3,
 ( #33132, #17143, #3109, #24578, #47459, #2142, #43528, #48171, #25293, #10022 ),
 .UNSPECIFIED., .F., .F.,
 ( 4, 2, 2, 2, 4 ),
 ( 0.1272669073658118100, 0.2522669073462989742, 0.3772669073267861939, 0.5022669073072734136, 0.6272669072877605778 ),
 .UNSPECIFIED. ) ;
#28889 = CARTESIAN_POINT ( 'NONE',  ( -15.41078985079695940, -7.636351814344855882, 74.27323974507916660 ) ) ;
#28890 = EDGE_LOOP ( 'NONE', ( #12229, #33904, #40998, #33673, #8695, #2024, #41089, #1964, #47627, #47779, #44555, #9032, #42606, #45746, #27641, #37167, #7877, #17841, #22418, #11893, #35319, #12329, #3156, #4123, #9557, #15411, #3668, #13524, #22748, #10958, #29325, #2098, #35936 ) ) ;
#28891 = ADVANCED_FACE ( 'NONE', ( #6870 ), #6389, .F. ) ;
#28892 = CARTESIAN_POINT ( 'NONE',  ( -19.30031737610338993, -22.01920738531545396, 58.70320165633192033 ) ) ;
#28893 = LINE ( 'NONE', #48096, #46935 ) ;
#28894 = ADVANCED_FACE ( 'NONE', ( #44546 ), #10801, .T. ) ;
#28895 = ORIENTED_EDGE ( 'NONE', *, *, #30139, .T. ) ;
#28896 = LINE ( 'NONE', #39988, #45414 ) ;
#28897 = CARTESIAN_POINT ( 'NONE',  ( -14.84927081153347039, -21.37251255130113137, 61.65072491673618771 ) ) ;
#28898 = AXIS2_PLACEMENT_3D ( 'NONE', #17892, #40555, #36373 ) ;
#28899 = VERTEX_POINT ( 'NONE', #47516 ) ;
#28900 = EDGE_CURVE ( 'NONE', #3266, #24111, #13749, .T. ) ;
#28901 = CARTESIAN_POINT ( 'NONE',  ( -23.75972628784533569, -10.79550978475970346, 47.99999999999994316 ) ) ;
#28902 = CARTESIAN_POINT ( 'NONE',  ( -19.04042241193164386, -7.536568769452434147, 67.01576393362593365 ) ) ;
#28903 = CARTESIAN_POINT ( 'NONE',  ( -26.42409385541305511, -6.859206544744110623, 52.99999999999997158 ) ) ;
#28904 = ORIENTED_EDGE ( 'NONE', *, *, #36858, .F. ) ;
#28905 = CARTESIAN_POINT ( 'NONE',  ( -20.14548719510382924, -7.874031717564547783, 73.92085388793562117 ) ) ;
#28906 = CARTESIAN_POINT ( 'NONE',  ( -24.82750207115152463, -13.97654542584719373, 73.30766806548945169 ) ) ;
#28907 = CIRCLE ( 'NONE', #36749, 4.686499999999998778 ) ;
#28908 = EDGE_CURVE ( 'NONE', #19604, #32745, #17692, .T. ) ;
#28909 = LINE ( 'NONE', #36516, #39985 ) ;
#28910 = CARTESIAN_POINT ( 'NONE',  ( -22.27985548098255109, -20.46033401586769429, 58.87787560672637710 ) ) ;
#28911 = EDGE_LOOP ( 'NONE', ( #41464, #3623, #39175, #4010, #46922 ) ) ;
#28912 = CARTESIAN_POINT ( 'NONE',  ( -22.43638724005049667, -20.32197157274265820, 62.34783858214098728 ) ) ;
#28913 = AXIS2_PLACEMENT_3D ( 'NONE', #3048, #18061, #33072 ) ;
#28914 = CARTESIAN_POINT ( 'NONE',  ( -11.35825037048775066, -11.21643016533577075, 60.67885780704620657 ) ) ;
#28915 = CARTESIAN_POINT ( 'NONE',  ( -15.49416032233947504, -8.028509233753512220, 74.07985659018983426 ) ) ;
#28916 = CARTESIAN_POINT ( 'NONE',  ( -17.11594671439511828, -7.315539529225058679, 54.27966884056655061 ) ) ;
#28917 = CARTESIAN_POINT ( 'NONE',  ( -21.73659385650551812, -6.915538690918074494, 49.31353937987644542 ) ) ;
#28918 = CARTESIAN_POINT ( 'NONE',  ( -16.78341102624552050, -22.23169286577646986, 68.88055947109249644 ) ) ;
#28919 = CARTESIAN_POINT ( 'NONE',  ( -24.30112618867181240, -13.25578303422174997, 59.64795780745660636 ) ) ;
#28920 = ORIENTED_EDGE ( 'NONE', *, *, #6952, .F. ) ;
#28921 = CARTESIAN_POINT ( 'NONE',  ( -10.67753361921853461, -12.94244927161164505, 64.49509439877509465 ) ) ;
#28922 = LINE ( 'NONE', #43231, #43936 ) ;
#28923 = DIRECTION ( 'NONE',  ( -5.731567514496413899E-31, -1.020425574103664789E-16, -1.000000000000000000 ) ) ;
#28924 = ORIENTED_EDGE ( 'NONE', *, *, #1912, .F. ) ;
#28925 = CARTESIAN_POINT ( 'NONE',  ( -17.00410685006708178, -7.771727545396207582, 73.96018273221115180 ) ) ;
#28926 = ORIENTED_EDGE ( 'NONE', *, *, #24588, .T. ) ;
#28927 = VERTEX_POINT ( 'NONE', #30022 ) ;
#28928 = ORIENTED_EDGE ( 'NONE', *, *, #46385, .T. ) ;
#28929 = CARTESIAN_POINT ( 'NONE',  ( -14.04312670088115134, -20.93869291823072132, 72.22607738042698600 ) ) ;
#28930 = AXIS2_PLACEMENT_3D ( 'NONE', #2371, #6314, #28719 ) ;
#28931 = LINE ( 'NONE', #25251, #42097 ) ;
#28932 = EDGE_CURVE ( 'NONE', #2764, #21586, #3835, .T. ) ;
#28933 = CARTESIAN_POINT ( 'NONE',  ( -13.71283467540607504, -11.09584481999758232, 50.77966884056655772 ) ) ;
#28934 = CARTESIAN_POINT ( 'NONE',  ( -12.68532353738824803, -9.060482037740600347, 71.03420644255490402 ) ) ;
#28935 = AXIS2_PLACEMENT_3D ( 'NONE', #38048, #38786, #31653 ) ;
#28936 = AXIS2_PLACEMENT_3D ( 'NONE', #4214, #45336, #22939 ) ;
#28937 = ORIENTED_EDGE ( 'NONE', *, *, #11817, .F. ) ;
#28938 = ORIENTED_EDGE ( 'NONE', *, *, #4246, .T. ) ;
#28939 = CARTESIAN_POINT ( 'NONE',  ( -19.57409385650551670, -9.792211528768504536, 50.49490371617623197 ) ) ;
#28940 = DIRECTION ( 'NONE',  ( 0.000000000000000000, 0.000000000000000000, 1.000000000000000000 ) ) ;
#28941 = AXIS2_PLACEMENT_3D ( 'NONE', #21951, #44374, #6933 ) ;
#28942 = CARTESIAN_POINT ( 'NONE',  ( -11.34764044004908534, -18.38430194568898912, 58.10154788514100943 ) ) ;
#28943 = CARTESIAN_POINT ( 'NONE',  ( -19.85534385650552025, -7.417179338643134834, 52.18511593390279302 ) ) ;
#28944 = ADVANCED_FACE ( 'NONE', ( #45289 ), #30518, .T. ) ;
#28945 = CIRCLE ( 'NONE', #20192, 4.686499999999999666 ) ;
#28946 = ORIENTED_EDGE ( 'NONE', *, *, #19430, .F. ) ;
#28947 = CARTESIAN_POINT ( 'NONE',  ( -23.92465930214516234, -12.07130710318904221, 59.57415707955740203 ) ) ;
#28948 = CARTESIAN_POINT ( 'NONE',  ( -24.36028583763659583, -16.11466138999042030, 69.67740616536292464 ) ) ;
#28949 = ORIENTED_EDGE ( 'NONE', *, *, #42408, .F. ) ;
#28950 = CARTESIAN_POINT ( 'NONE',  ( -17.04413539470110095, -21.84925844046378174, 72.45071136019464575 ) ) ;
#28951 = ORIENTED_EDGE ( 'NONE', *, *, #1620, .T. ) ;
#28952 = EDGE_CURVE ( 'NONE', #42513, #22563, #708, .T. ) ;
#28953 = CARTESIAN_POINT ( 'NONE',  ( -14.63112947634313521, -8.332108846598762497, 67.35155072858903225 ) ) ;
#28954 = CARTESIAN_POINT ( 'NONE',  ( -11.02440266205174524, -11.97271778485252192, 74.55840233405203321 ) ) ;
#28955 = CARTESIAN_POINT ( 'NONE',  ( -13.57213406898786978, -20.71828813759911014, 58.04649799015020761 ) ) ;
#28956 = ORIENTED_EDGE ( 'NONE', *, *, #6881, .F. ) ;
#28957 = AXIS2_PLACEMENT_3D ( 'NONE', #38046, #27705, #12200 ) ;
#28958 = CARTESIAN_POINT ( 'NONE',  ( -19.24025795797341942, -7.996846695050864540, 60.24620885950562865 ) ) ;
#28959 = EDGE_CURVE ( 'NONE', #17956, #32730, #39518, .T. ) ;
#28960 = VECTOR ( 'NONE', #40431, 1000.000000000000000 ) ;
#28961 = CARTESIAN_POINT ( 'NONE',  ( -23.17061082369141900, -10.06671700699632233, 66.72837583070179335 ) ) ;
#28962 = CARTESIAN_POINT ( 'NONE',  ( -23.40706900507760224, -18.44293855997280929, 73.06368236814604700 ) ) ;
#28963 = VERTEX_POINT ( 'NONE', #41090 ) ;
#28964 = CARTESIAN_POINT ( 'NONE',  ( -21.52726120556258849, -9.076273861542912158, 70.28132538914752558 ) ) ;
#28965 = AXIS2_PLACEMENT_3D ( 'NONE', #23069, #48415, #11001 ) ;
#28966 = ORIENTED_EDGE ( 'NONE', *, *, #14348, .F. ) ;
#28967 = CARTESIAN_POINT ( 'NONE',  ( -14.90123591195245112, -21.39555782113924209, 65.52085318447059592 ) ) ;
#28968 = B_SPLINE_CURVE_WITH_KNOTS ( 'NONE', 3,
 ( #2318, #24508, #39508, #17566, #32373, #5787, #35560, #39014, #39993, #20794 ),
 .UNSPECIFIED., .F., .F.,
 ( 4, 2, 2, 2, 4 ),
 ( 0.000000000000000000, 0.2500000000000000000, 0.5000000000000000000, 0.7500000000000000000, 1.000000000000000000 ),
 .UNSPECIFIED. ) ;
#28969 = ORIENTED_EDGE ( 'NONE', *, *, #43874, .F. ) ;
#28970 = DIRECTION ( 'NONE',  ( -3.071710424422018668E-17, 6.404604876783312462E-16, 1.000000000000000000 ) ) ;
#28971 = CARTESIAN_POINT ( 'NONE',  ( -13.65110163016468015, -21.23324793748626504, 68.57129851394472553 ) ) ;
#28972 = CARTESIAN_POINT ( 'NONE',  ( -10.39241571269986331, -17.41794234916963191, 53.49999999999994316 ) ) ;
#28973 = CARTESIAN_POINT ( 'NONE',  ( -22.63008543824757979, -10.12971389395683097, 70.01178520543939499 ) ) ;
#28974 = ORIENTED_EDGE ( 'NONE', *, *, #10263, .F. ) ;
#28975 = CARTESIAN_POINT ( 'NONE',  ( -10.37497030826117417, -14.69804335084345759, 71.32782692816427073 ) ) ;
#28976 = AXIS2_PLACEMENT_3D ( 'NONE', #14823, #25461, #34047 ) ;
#28977 = CARTESIAN_POINT ( 'NONE',  ( -23.80338573481879294, -11.80731802715296119, 59.76763678108634537 ) ) ;
#28979 = EDGE_CURVE ( 'NONE', #6635, #24347, #29160, .T. ) ;
#28978 = CARTESIAN_POINT ( 'NONE',  ( -23.34421923326152992, -18.54457442964731584, 69.57906566121042147 ) ) ;
#28980 = ORIENTED_EDGE ( 'NONE', *, *, #10175, .F. ) ;
#28981 = CARTESIAN_POINT ( 'NONE',  ( -17.42409385541299471, -14.80920654474435771, 49.52966884056655772 ) ) ;
#28982 = EDGE_CURVE ( 'NONE', #34596, #37312, #33425, .T. ) ;
#28983 = CARTESIAN_POINT ( 'NONE',  ( -10.98557804775572144, -17.68114217416224321, 71.71718193507115302 ) ) ;
#28984 = EDGE_CURVE ( 'NONE', #33229, #30155, #8107, .T. ) ;
#28985 = EDGE_CURVE ( 'NONE', #26173, #38482, #33096, .T. ) ;
#28986 = ORIENTED_EDGE ( 'NONE', *, *, #34795, .T. ) ;
#28987 = ORIENTED_EDGE ( 'NONE', *, *, #32860, .T. ) ;
#28988 = CARTESIAN_POINT ( 'NONE',  ( -13.85546777306732480, -20.89347761745142407, 72.01787893532731744 ) ) ;
#28989 = CARTESIAN_POINT ( 'NONE',  ( -10.02101610845663870, -15.64516224647144149, 61.16072161825523068 ) ) ;
#28990 = CARTESIAN_POINT ( 'NONE',  ( -24.18470913683765389, -12.80901137141652768, 69.78715111652664405 ) ) ;
#28991 = CARTESIAN_POINT ( 'NONE',  ( -12.74836358285320159, -20.08597126951521261, 71.82125749157572159 ) ) ;
#28992 =( BOUNDED_CURVE ( )  B_SPLINE_CURVE ( 3, ( #17662, #39841, #21136, #10298 ),
 .UNSPECIFIED., .F., .F. ) 
 B_SPLINE_CURVE_WITH_KNOTS ( ( 4, 4 ),
 ( 0.000000000000000000, 0.4074455897393665649 ),
 .UNSPECIFIED. ) 
 CURVE ( )  GEOMETRIC_REPRESENTATION_ITEM ( )  RATIONAL_B_SPLINE_CURVE ( ( 1.000000000000000000, 0.4567392136813214210, 0.3561768502900264366, 0.6983129098261150469 ) ) 
 REPRESENTATION_ITEM ( '' )  );
#28993 = CARTESIAN_POINT ( 'NONE',  ( -35.32409385541306079, -8.109206544744111511, 50.49999999999998579 ) ) ;
#28994 = CARTESIAN_POINT ( 'NONE',  ( -12.35277413765887999, -20.26681541663451114, 68.45162113748973809 ) ) ;
#28995 = CARTESIAN_POINT ( 'NONE',  ( -22.74914502862361587, -19.44157078561079999, 72.79967855327656423 ) ) ;
#28996 = ORIENTED_EDGE ( 'NONE', *, *, #13844, .F. ) ;
#28997 = ORIENTED_EDGE ( 'NONE', *, *, #28603, .F. ) ;
#28998 = FACE_OUTER_BOUND ( 'NONE', #18294, .T. ) ;
#28999 = PLANE ( 'NONE',  #24416 ) ;
#29000 = VECTOR ( 'NONE', #11594, 1000.000000000000000 ) ;
#29001 = CARTESIAN_POINT ( 'NONE',  ( -14.97035482569482312, -21.41873484682592377, 61.92128389535452015 ) ) ;
#29002 = CARTESIAN_POINT ( 'NONE',  ( -10.38181936765313473, -14.47839093401252875, 67.85800130414834541 ) ) ;
#29003 = CARTESIAN_POINT ( 'NONE',  ( -12.74138925215518015, -14.62063335304397427, 49.52966884056655772 ) ) ;
#29004 = VECTOR ( 'NONE', #36190, 1000.000000000000000 ) ;
#29005 = CARTESIAN_POINT ( 'NONE',  ( -18.24909385650551741, -8.104110260919579645, 48.81699501597546487 ) ) ;
#29006 =( BOUNDED_SURFACE ( )  B_SPLINE_SURFACE ( 3, 1, ( 
 ( #19130, #33901 ),
 ( #22098, #30230 ),
 ( #3373, #4131 ),
 ( #25785, #45491 ),
 ( #194, #40799 ),
 ( #3621, #18381 ),
 ( #18622, #48676 ) ),
 .UNSPECIFIED., .T., .F., .F. ) 
 B_SPLINE_SURFACE_WITH_KNOTS ( ( 4, 3, 4 ),
 ( 2, 2 ),
 ( 0.000000000000000000, 0.5000000000000000000, 1.000000000000000000 ),
 ( 0.000000000000000000, 1.000000000000000000 ),
 .UNSPECIFIED. ) 
 GEOMETRIC_REPRESENTATION_ITEM ( )  RATIONAL_B_SPLINE_SURFACE ( (
 ( 1.000000000000000000, 1.000000000000000000),
 ( 0.3333333333333335369, 0.3333333333333330373),
 ( 0.3333333333333335369, 0.3333333333333330373),
 ( 1.000000000000000000, 1.000000000000000000),
 ( 0.3333333333333333703, 0.3333333333333333703),
 ( 0.3333333333333333703, 0.3333333333333333703),
 ( 1.000000000000000000, 1.000000000000000000) ) ) 
 REPRESENTATION_ITEM ( '' )  SURFACE ( )  );
#29007 = AXIS2_PLACEMENT_3D ( 'NONE', #5440, #13038, #9624 ) ;
#29008 = ORIENTED_EDGE ( 'NONE', *, *, #15308, .T. ) ;
#29009 = CARTESIAN_POINT ( 'NONE',  ( -21.13535303541994281, -18.52256826949110291, 52.02966884056656482 ) ) ;
#29010 = DIRECTION ( 'NONE',  ( -2.515467001362780054E-08, -7.569581535656660169E-10, 0.9999999999999996669 ) ) ;
#29011 = CARTESIAN_POINT ( 'NONE',  ( -17.42409385541299471, -14.80920654474435594, 52.02966884056656482 ) ) ;
#29012 = CARTESIAN_POINT ( 'NONE',  ( -19.30128557755455532, -21.60500301973953086, 58.81035253397666196 ) ) ;
#29013 = VERTEX_POINT ( 'NONE', #38348 ) ;
#29014 =( BOUNDED_SURFACE ( )  B_SPLINE_SURFACE ( 3, 1, ( 
 ( #36451, #35973 ),
 ( #2729, #17737 ),
 ( #32766, #33981 ),
 ( #25874, #25623 ),
 ( #30321, #278 ),
 ( #18469, #41137 ),
 ( #33230, #22673 ) ),
 .UNSPECIFIED., .T., .F., .F. ) 
 B_SPLINE_SURFACE_WITH_KNOTS ( ( 4, 3, 4 ),
 ( 2, 2 ),
 ( 0.000000000000000000, 0.5000000000000000000, 1.000000000000000000 ),
 ( 0.000000000000000000, 1.000000000000000000 ),
 .UNSPECIFIED. ) 
 GEOMETRIC_REPRESENTATION_ITEM ( )  RATIONAL_B_SPLINE_SURFACE ( (
 ( 1.000000000000000000, 1.000000000000000000),
 ( 0.3333333333333335369, 0.3333333333333330373),
 ( 0.3333333333333335369, 0.3333333333333330373),
 ( 1.000000000000000000, 1.000000000000000000),
 ( 0.3333333333333333703, 0.3333333333333333703),
 ( 0.3333333333333333703, 0.3333333333333333703),
 ( 1.000000000000000000, 1.000000000000000000) ) ) 
 REPRESENTATION_ITEM ( '' )  SURFACE ( )  );
#29015 = ADVANCED_FACE ( 'NONE', ( #34175 ), #23353, .T. ) ;
#29016 = CARTESIAN_POINT ( 'NONE',  ( -13.53844544295976249, -20.69534049476535031, 65.40117765236396963 ) ) ;
#29017 = CARTESIAN_POINT ( 'NONE',  ( 18.82590614458706924, 1.903197776136028807, 48.78032500931639959 ) ) ;
#29018 = DIRECTION ( 'NONE',  ( 1.000000000000000000, -4.164305804376849172E-17, 1.614929280266638808E-16 ) ) ;
#29019 = B_SPLINE_CURVE_WITH_KNOTS ( 'NONE', 3,
 ( #42493, #4566, #30687, #19588, #34597, #12436, #46428, #881, #12683, #24025 ),
 .UNSPECIFIED., .F., .F.,
 ( 4, 2, 2, 2, 4 ),
 ( 0.6272669072877820051, 0.7522669073072913992, 0.8772669073268006823, 1.002266907346310187, 1.127266907365819470 ),
 .UNSPECIFIED. ) ;
#29020 = CARTESIAN_POINT ( 'NONE',  ( -16.13263948075386978, -7.878200451182638453, 63.68483172840383588 ) ) ;
#29021 = VERTEX_POINT ( 'NONE', #18419 ) ;
#29022 = CARTESIAN_POINT ( 'NONE',  ( -19.08517061958907490, -7.953970113302217371, 60.16912824253490299 ) ) ;
#29023 = ORIENTED_EDGE ( 'NONE', *, *, #31906, .F. ) ;
#29024 = CARTESIAN_POINT ( 'NONE',  ( -24.87269970749685299, -14.66254690463778942, 62.90634777101153219 ) ) ;
#29025 = ORIENTED_EDGE ( 'NONE', *, *, #37152, .T. ) ;
#29026 = CARTESIAN_POINT ( 'NONE',  ( -24.72409385541305582, -14.90920654474425255, 71.08235294117645253 ) ) ;
#29027 = CARTESIAN_POINT ( 'NONE',  ( -15.07409385650551670, -9.792211528768504536, 50.49490371617623197 ) ) ;
#29028 = AXIS2_PLACEMENT_3D ( 'NONE', #2753, #20997, #1801 ) ;
#29029 = ORIENTED_EDGE ( 'NONE', *, *, #46433, .F. ) ;
#29030 = DIRECTION ( 'NONE',  ( 0.000000000000000000, 1.000000000000000000, 0.000000000000000000 ) ) ;
#29031 = AXIS2_PLACEMENT_3D ( 'NONE', #29301, #44568, #33698 ) ;
#29032 = DIRECTION ( 'NONE',  ( -0.9524241471993249997, 0.3047743298226213149, 0.0009228828802126874372 ) ) ;
#29033 = CARTESIAN_POINT ( 'NONE',  ( -21.55883939963115026, -8.611815437115641458, 73.78624134823098757 ) ) ;
#29034 = EDGE_LOOP ( 'NONE', ( #10284, #3522, #4991, #44318 ) ) ;
#29035 = CARTESIAN_POINT ( 'NONE',  ( -19.23707162763026801, -10.47461692831664060, 49.52966884056655772 ) ) ;
#29036 = VECTOR ( 'NONE', #39880, 1000.000000000000000 ) ;
#29037 = AXIS2_PLACEMENT_3D ( 'NONE', #16791, #28133, #43158 ) ;
#29038 = ADVANCED_FACE ( 'NONE', ( #11301 ), #48465, .F. ) ;
#29039 = CARTESIAN_POINT ( 'NONE',  ( -17.15293984484763712, -7.364064364366409876, 70.53389935397558475 ) ) ;
#29040 = CARTESIAN_POINT ( 'NONE',  ( -24.05420634179087358, -17.20676946999824608, 69.69867738674849988 ) ) ;
#29041 = CARTESIAN_POINT ( 'NONE',  ( -23.42631727757699878, -10.39480074052133141, 59.78858809748042091 ) ) ;
#29042 = EDGE_CURVE ( 'NONE', #36353, #8191, #41330, .T. ) ;
#29043 = EDGE_CURVE ( 'NONE', #22189, #21219, #12472, .T. ) ;
#29044 = ORIENTED_EDGE ( 'NONE', *, *, #13609, .F. ) ;
#29045 = ORIENTED_EDGE ( 'NONE', *, *, #5745, .T. ) ;
#29046 = CARTESIAN_POINT ( 'NONE',  ( -21.23484681875272884, -20.74088929683185611, 69.33978048267414351 ) ) ;
#29047 = ORIENTED_EDGE ( 'NONE', *, *, #19226, .F. ) ;
#29048 = CARTESIAN_POINT ( 'NONE',  ( -20.69509153224808173, -8.115601224564374050, 63.49616927690831858 ) ) ;
#29049 = VECTOR ( 'NONE', #29781, 1000.000000000000000 ) ;
#29050 = CARTESIAN_POINT ( 'NONE',  ( -16.42409385759798823, -9.359200813967568422, 50.49621490985803263 ) ) ;
#29051 = CARTESIAN_POINT ( 'NONE',  ( -23.71751471349159601, -11.63122711669449316, 63.23746208799618529 ) ) ;
#29052 = CARTESIAN_POINT ( 'NONE',  ( -14.34827028450108344, -21.16170790896200060, 72.08174668229233362 ) ) ;
#29053 = CARTESIAN_POINT ( 'NONE',  ( -20.54969731993802995, -8.046573202280342230, 66.98115280391161264 ) ) ;
#29054 = CARTESIAN_POINT ( 'NONE',  ( 10.57590614458695377, -0.1092432217106413528, 50.52422457691089619 ) ) ;
#29055 = ORIENTED_EDGE ( 'NONE', *, *, #40762, .F. ) ;
#29056 = ADVANCED_FACE ( 'NONE', ( #27285 ), #10897, .T. ) ;
#29057 = CARTESIAN_POINT ( 'NONE',  ( -27.42409385541305511, -25.10920654474410441, 45.99999999999998579 ) ) ;
#29058 = DIRECTION ( 'NONE',  ( 0.2189141945955467017, -0.9757441136919982050, 0.000000000000000000 ) ) ;
#29059 = DIRECTION ( 'NONE',  ( 1.000000000000000000, 2.866981220435666553E-17, 0.000000000000000000 ) ) ;
#29060 = ORIENTED_EDGE ( 'NONE', *, *, #7011, .T. ) ;
#29061 = ORIENTED_EDGE ( 'NONE', *, *, #38238, .T. ) ;
#29062 = B_SPLINE_CURVE_WITH_KNOTS ( 'NONE', 1,
 ( #39068, #34157 ),
 .UNSPECIFIED., .F., .F.,
 ( 2, 2 ),
 ( 0.000000000000000000, 1.000000000000000000 ),
 .UNSPECIFIED. ) ;
#29063 = ADVANCED_FACE ( 'NONE', ( #31708 ), #16432, .T. ) ;
#29064 = CARTESIAN_POINT ( 'NONE',  ( -17.66159697976433307, -21.85550285805611637, 58.42025434932890704 ) ) ;
#29065 = CARTESIAN_POINT ( 'NONE',  ( -23.66688185712976633, -11.64243612726180643, 62.96720739904996833 ) ) ;
#29066 = CIRCLE ( 'NONE', #19662, 1.049999999999998934 ) ;
#29067 = CARTESIAN_POINT ( 'NONE',  ( -23.91639008814848211, -11.15506099060319123, 69.99236505904349315 ) ) ;
#29068 = DIRECTION ( 'NONE',  ( 0.000000000000000000, -0.9999954153791273948, -0.003028072113819838245 ) ) ;
#29069 = ORIENTED_EDGE ( 'NONE', *, *, #21141, .T. ) ;
#29070 = VECTOR ( 'NONE', #39105, 1000.000000000000000 ) ;
#29071 = LINE ( 'NONE', #44350, #19558 ) ;
#29072 = CARTESIAN_POINT ( 'NONE',  ( -11.40126873537406205, -11.24191379345135999, 60.97885781058090515 ) ) ;
#29073 = ADVANCED_FACE ( 'NONE', ( #1669 ), #9558, .T. ) ;
#29074 = EDGE_LOOP ( 'NONE', ( #39200, #13013, #33381, #37374, #14503 ) ) ;
#29075 = LINE ( 'NONE', #7662, #27635 ) ;
#29076 = CARTESIAN_POINT ( 'NONE',  ( -17.78490012859682423, -21.80118270052165741, 62.10365751430077808 ) ) ;
#29077 = FACE_OUTER_BOUND ( 'NONE', #39633, .T. ) ;
#29078 = ORIENTED_EDGE ( 'NONE', *, *, #8427, .T. ) ;
#29079 = CARTESIAN_POINT ( 'NONE',  ( -11.97490362423377164, -10.33561459433851404, 67.78424783647008667 ) ) ;
#29080 = VERTEX_POINT ( 'NONE', #16674 ) ;
#29081 = CARTESIAN_POINT ( 'NONE',  ( -24.31823774515246939, -17.63313259158020685, 66.05861911469568781 ) ) ;
#29082 = CARTESIAN_POINT ( 'NONE',  ( -13.52830415862076308, -20.68508020484520671, 61.51646354542308615 ) ) ;
#29083 = FACE_BOUND ( 'NONE', #24569, .T. ) ;
#29084 = VERTEX_POINT ( 'NONE', #46500 ) ;
#29085 = CARTESIAN_POINT ( 'NONE',  ( -21.40357752720559503, -21.10733023442637446, 69.15426546848676992 ) ) ;
#29086 = CARTESIAN_POINT ( 'NONE',  ( -10.72572792941078212, -12.60087465324735945, 64.68324854050578665 ) ) ;
#29087 = CARTESIAN_POINT ( 'NONE',  ( -22.89284385650552167, -7.406986770994972602, 48.81910596585309747 ) ) ;
#29088 = CARTESIAN_POINT ( 'NONE',  ( -10.80019681701181966, -17.07282933688417970, 57.79646546703656895 ) ) ;
#29089 = DIRECTION ( 'NONE',  ( 0.05957303659011964347, 0.9982239494779874267, -2.515684304544914870E-08 ) ) ;
#29090 = DIRECTION ( 'NONE',  ( -5.408674110437222193E-06, 4.460197095916123975E-06, 0.9999999999754265456 ) ) ;
#29091 = ORIENTED_EDGE ( 'NONE', *, *, #30482, .T. ) ;
#29092 = CARTESIAN_POINT ( 'NONE',  ( -24.87143190479848798, -14.60822328784750646, 62.81958198222076106 ) ) ;
#29093 = CARTESIAN_POINT ( 'NONE',  ( -20.50783493979771421, -8.027295371342848540, 66.96599508560271374 ) ) ;
#29094 = CARTESIAN_POINT ( 'NONE',  ( -16.17583575424048092, -10.27959207348368764, 49.52966884056655772 ) ) ;
#29095 = DIRECTION ( 'NONE',  ( -3.071710424422018668E-17, 6.404604876783312462E-16, 1.000000000000000000 ) ) ;
#29096 = CARTESIAN_POINT ( 'NONE',  ( -24.27033112822875438, -13.12649005559073423, 63.13264177271825872 ) ) ;
#29097 = ADVANCED_FACE ( 'NONE', ( #31464 ), #947, .T. ) ;
#29098 = ORIENTED_EDGE ( 'NONE', *, *, #29192, .T. ) ;
#29099 = ORIENTED_EDGE ( 'NONE', *, *, #2359, .T. ) ;
#29100 = AXIS2_PLACEMENT_3D ( 'NONE', #2194, #3160, #29506 ) ;
#29101 = CARTESIAN_POINT ( 'NONE',  ( -22.70900583301066433, -10.21894050583236968, 66.55684684265230544 ) ) ;
#29102 = DIRECTION ( 'NONE',  ( 0.000000000000000000, 1.000000000000000000, 0.000000000000000000 ) ) ;
#29103 = ORIENTED_EDGE ( 'NONE', *, *, #38698, .T. ) ;
#29105 = CARTESIAN_POINT ( 'NONE',  ( -11.40127056704611519, -11.24191079892443135, 60.67885781060143557 ) ) ;
#29104 = CARTESIAN_POINT ( 'NONE',  ( -19.28288283825861527, -21.60990478829091899, 58.81947569273916088 ) ) ;
#29106 = CARTESIAN_POINT ( 'NONE',  ( -13.41953676616927460, -9.006914687363744676, 60.73950246439220280 ) ) ;
#29107 = AXIS2_PLACEMENT_3D ( 'NONE', #43883, #35500, #20736 ) ;
#29108 = CARTESIAN_POINT ( 'NONE',  ( -19.50103315386265024, -8.068942516160735323, 60.37581784757137626 ) ) ;
#29109 = DIRECTION ( 'NONE',  ( 0.000000000000000000, -1.000000000000000000, 0.000000000000000000 ) ) ;
#29110 = CARTESIAN_POINT ( 'NONE',  ( -24.74044779172452024, -16.21442189768792375, 62.63682720862403386 ) ) ;
#29111 = CARTESIAN_POINT ( 'NONE',  ( -17.42409385541306222, -14.80920654474411080, 75.49999999999998579 ) ) ;
#29112 = CIRCLE ( 'NONE', #2400, 5.249999999999998224 ) ;
#29113 = CARTESIAN_POINT ( 'NONE',  ( -10.42278038625809700, -14.74509079444783843, 74.90852043434034613 ) ) ;
#29114 = EDGE_CURVE ( 'NONE', #33155, #35366, #40698, .T. ) ;
#29115 = EDGE_CURVE ( 'NONE', #11354, #42239, #26836, .T. ) ;
#29116 = DIRECTION ( 'NONE',  ( -7.166348394334737576E-06, 1.030346079289304524E-05, 0.9999999999212411117 ) ) ;
#29117 = VERTEX_POINT ( 'NONE', #5624 ) ;
#29118 = CARTESIAN_POINT ( 'NONE',  ( -33.95962776134579286, -8.109206544744111511, 50.50000000000000000 ) ) ;
#29119 = DIRECTION ( 'NONE',  ( 0.000000000000000000, 0.000000000000000000, 1.000000000000000000 ) ) ;
#29120 = ADVANCED_FACE ( 'NONE', ( #46248 ), #2413, .T. ) ;
#29121 = AXIS2_PLACEMENT_3D ( 'NONE', #15173, #30231, #34138 ) ;
#29122 = EDGE_CURVE ( 'NONE', #25093, #41531, #33134, .T. ) ;
#29123 = CARTESIAN_POINT ( 'NONE',  ( -18.11889358109259973, -21.82488563948435711, 65.64532159284070190 ) ) ;
#29124 = DIRECTION ( 'NONE',  ( 3.413470714839332458E-33, -1.190614954331866791E-16, 1.000000000000000000 ) ) ;
#29125 = DIRECTION ( 'NONE',  ( -3.549360974551883545E-17, 6.371834667872732552E-18, 1.000000000000000000 ) ) ;
#29126 = CARTESIAN_POINT ( 'NONE',  ( -16.44450580018572339, -21.74194830683597957, 65.41491530808407617 ) ) ;
#29127 = ORIENTED_EDGE ( 'NONE', *, *, #17843, .T. ) ;
#29128 = EDGE_LOOP ( 'NONE', ( #47223, #416, #29864, #29764 ) ) ;
#29129 = CARTESIAN_POINT ( 'NONE',  ( -19.31784385541304516, -6.860780111191487229, 51.02154966934377001 ) ) ;
#29130 = VERTEX_POINT ( 'NONE', #17871 ) ;
#29131 = EDGE_CURVE ( 'NONE', #29545, #20111, #3114, .T. ) ;
#29132 = CARTESIAN_POINT ( 'NONE',  ( -17.34580053807816924, -7.359449399152106608, 67.18072987562666754 ) ) ;
#29133 = CARTESIAN_POINT ( 'NONE',  ( -19.12163971562669218, -7.963538243666484107, 67.31560661829935555 ) ) ;
#29134 = B_SPLINE_CURVE_WITH_KNOTS ( 'NONE', 3,
 ( #25819, #22884, #7124, #22140, #18417, #22375, #33422, #26311, #11536, #14697 ),
 .UNSPECIFIED., .F., .F.,
 ( 4, 2, 2, 2, 4 ),
 ( 0.6272669072877884444, 0.7522669073072847379, 0.8772669073267809203, 1.002266907346277325, 1.127266907365773507 ),
 .UNSPECIFIED. ) ;
#29135 = CARTESIAN_POINT ( 'NONE',  ( -23.41616298382994898, -18.52428493080399008, 72.77840375779385340 ) ) ;
#29136 = CARTESIAN_POINT ( 'NONE',  ( -10.37382936219775154, -14.83089353207902050, 74.81251018390587149 ) ) ;
#29137 = VERTEX_POINT ( 'NONE', #9795 ) ;
#29138 = AXIS2_PLACEMENT_3D ( 'NONE', #8048, #33607, #26246 ) ;
#29139 = CARTESIAN_POINT ( 'NONE',  ( -19.29341177869643431, -22.02104676444090359, 58.68653925579838671 ) ) ;
#29140 = CARTESIAN_POINT ( 'NONE',  ( -22.04378365035703879, -20.13510231884741231, 62.24911246861644543 ) ) ;
#29141 = ORIENTED_EDGE ( 'NONE', *, *, #43150, .F. ) ;
#29142 =( BOUNDED_CURVE ( )  B_SPLINE_CURVE ( 2, ( #768, #45834, #1007, #46065, #23670, #8891, #12325, #23910, #5191 ),
 .UNSPECIFIED., .F., .F. ) 
 B_SPLINE_CURVE_WITH_KNOTS ( ( 3, 2, 2, 2, 3 ),
 ( 0.06687857201681655928, 0.06786219470523666142, 0.06884581739365676356, 0.06982944008207687958, 0.07081306277049698172 ),
 .UNSPECIFIED. ) 
 CURVE ( )  GEOMETRIC_REPRESENTATION_ITEM ( )  RATIONAL_B_SPLINE_CURVE ( ( 0.9999999999999756861, 0.9238795325113110524, 1.000000000000000000, 0.9238795325112867385, 1.000000000000000000, 0.9238795325112867385, 1.000000000000000000, 0.9238795325112509893, 1.000000000000035749 ) ) 
 REPRESENTATION_ITEM ( '' )  );
#29143 = CARTESIAN_POINT ( 'NONE',  ( -42.04765403640853094, -14.90920654474421170, 66.01151855203617913 ) ) ;
#29144 = CIRCLE ( 'NONE', #821, 1.999999999999999778 ) ;
#29145 = ORIENTED_EDGE ( 'NONE', *, *, #35597, .T. ) ;
#29146 = CARTESIAN_POINT ( 'NONE',  ( -17.72634082312590920, -21.85272461445201486, 58.40553378267873796 ) ) ;
#29147 = CARTESIAN_POINT ( 'NONE',  ( -21.48252188606478086, -21.05763224395268196, 69.16794793541382091 ) ) ;
#29148 = PLANE ( 'NONE',  #45468 ) ;
#29149 = ORIENTED_EDGE ( 'NONE', *, *, #13606, .F. ) ;
#29150 = CARTESIAN_POINT ( 'NONE',  ( -20.12289019246589206, -7.865124395032225380, 73.90592041591946781 ) ) ;
#29151 = CARTESIAN_POINT ( 'NONE',  ( -24.82750207115152463, -13.97654542584719373, 73.30766806548945169 ) ) ;
#29152 = CIRCLE ( 'NONE', #4002, 0.4000000000000010214 ) ;
#29153 = EDGE_CURVE ( 'NONE', #30489, #25477, #25523, .T. ) ;
#29154 = CARTESIAN_POINT ( 'NONE',  ( -10.75977711076063414, -17.10919593975601316, 61.15743126648893480 ) ) ;
#29155 = CARTESIAN_POINT ( 'NONE',  ( -23.96897392247960923, -17.29205672707886166, 66.05243358630347927 ) ) ;
#29156 = VERTEX_POINT ( 'NONE', #6083 ) ;
#29157 = B_SPLINE_CURVE_WITH_KNOTS ( 'NONE', 3,
 ( #1250, #14184, #29239, #43302, #39592, #5868, #35879, #2161, #47230, #32452 ),
 .UNSPECIFIED., .F., .F.,
 ( 4, 2, 2, 2, 4 ),
 ( 0.000000000000000000, 0.2500000000000000000, 0.5000000000000000000, 0.7500000000000000000, 1.000000000000000000 ),
 .UNSPECIFIED. ) ;
#29158 = CARTESIAN_POINT ( 'NONE',  ( -17.42409385541299471, -14.80920654474434883, 62.02966884056656482 ) ) ;
#29160 =( BOUNDED_CURVE ( )  B_SPLINE_CURVE ( 3, ( #37371, #26558, #12030, #4168 ),
 .UNSPECIFIED., .F., .F. ) 
 B_SPLINE_CURVE_WITH_KNOTS ( ( 4, 4 ),
 ( 0.4074455897393628456, 0.5000000000000000000 ),
 .UNSPECIFIED. ) 
 CURVE ( )  GEOMETRIC_REPRESENTATION_ITEM ( )  RATIONAL_B_SPLINE_CURVE ( ( 0.6983129098260804080, 0.7760317562606710018, 0.8765941196519728695, 0.9999999999999741318 ) ) 
 REPRESENTATION_ITEM ( '' )  );
#29159 = CARTESIAN_POINT ( 'NONE',  ( -11.98246295270348050, -15.60836430055780610, 53.49999999999995026 ) ) ;
#29161 = LINE ( 'NONE', #44208, #19516 ) ;
#29162 = CARTESIAN_POINT ( 'NONE',  ( -22.29909385650551812, -8.114302828567740988, 52.18300498402516041 ) ) ;
#29163 = EDGE_CURVE ( 'NONE', #32600, #17349, #26056, .T. ) ;
#29164 = VECTOR ( 'NONE', #34041, 1000.000000000000114 ) ;
#29165 = LINE ( 'NONE', #32140, #21214 ) ;
#29166 = CARTESIAN_POINT ( 'NONE',  ( -23.62573085457600541, -18.93877797592854506, 65.93734031310268051 ) ) ;
#29167 = ORIENTED_EDGE ( 'NONE', *, *, #8216, .T. ) ;
#29168 = DIRECTION ( 'NONE',  ( -3.485387654165294196E-16, 2.355958133329952458E-32, -1.000000000000000000 ) ) ;
#29169 = CARTESIAN_POINT ( 'NONE',  ( -14.01118748589247964, -10.49619482288619565, 54.07175714974879099 ) ) ;
#29170 = CARTESIAN_POINT ( 'NONE',  ( -11.73709015858045035, -9.996482182051650511, 67.67709622917277557 ) ) ;
#29171 = ORIENTED_EDGE ( 'NONE', *, *, #36980, .F. ) ;
#29172 = CARTESIAN_POINT ( 'NONE',  ( -17.42409385541299471, -14.80920654474435594, 52.02966884056656482 ) ) ;
#29173 = VECTOR ( 'NONE', #34197, 1000.000000000000000 ) ;
#29174 = VERTEX_POINT ( 'NONE', #47461 ) ;
#29175 = ORIENTED_EDGE ( 'NONE', *, *, #15478, .F. ) ;
#29176 = ORIENTED_EDGE ( 'NONE', *, *, #22728, .T. ) ;
#29177 = EDGE_CURVE ( 'NONE', #33352, #21704, #45725, .T. ) ;
#29179 = CARTESIAN_POINT ( 'NONE',  ( -21.30779305846920479, -20.69320811116774195, 72.53006253430444872 ) ) ;
#29178 = AXIS2_PLACEMENT_3D ( 'NONE', #9251, #20583, #12445 ) ;
#29180 = ADVANCED_FACE ( 'NONE', ( #5853 ), #14169, .T. ) ;
#29181 = LINE ( 'NONE', #22034, #41279 ) ;
#29182 = DIRECTION ( 'NONE',  ( 0.4599824152910791941, 0.8879280250239793837, 2.250728352126283350E-08 ) ) ;
#29183 = FACE_OUTER_BOUND ( 'NONE', #44271, .T. ) ;
#29184 = AXIS2_PLACEMENT_3D ( 'NONE', #36328, #9997, #32642 ) ;
#29185 = EDGE_LOOP ( 'NONE', ( #1796, #41913, #7095, #32656 ) ) ;
#29186 = ORIENTED_EDGE ( 'NONE', *, *, #38661, .T. ) ;
#29187 = ADVANCED_FACE ( 'NONE', ( #20867 ), #2393, .T. ) ;
#29188 = CARTESIAN_POINT ( 'NONE',  ( -17.09909385650551528, -8.114302828567740988, 52.18300498402516041 ) ) ;
#29189 = LINE ( 'NONE', #14371, #46501 ) ;
#29190 = VECTOR ( 'NONE', #3443, 1000.000000000000000 ) ;
#29191 = FACE_OUTER_BOUND ( 'NONE', #36889, .T. ) ;
#29192 = EDGE_CURVE ( 'NONE', #25531, #41086, #35474, .T. ) ;
#29193 = CARTESIAN_POINT ( 'NONE',  ( -20.36159385650551812, -9.295667164867525756, 49.30633214617472504 ) ) ;
#29194 = ORIENTED_EDGE ( 'NONE', *, *, #34713, .F. ) ;
#29195 = LINE ( 'NONE', #33587, #43512 ) ;
#29196 = VECTOR ( 'NONE', #21042, 1000.000000000000000 ) ;
#29197 = CARTESIAN_POINT ( 'NONE',  ( -24.79781851656146330, -15.87314393256401424, 69.64812203948034153 ) ) ;
#29198 = DIRECTION ( 'NONE',  ( 0.6621635203543606574, 0.7493593746073508033, 2.316976118889566110E-08 ) ) ;
#29199 = VERTEX_POINT ( 'NONE', #13696 ) ;
#29200 = CARTESIAN_POINT ( 'NONE',  ( -18.78767905735283605, -20.13749289187802916, 54.07175714974878389 ) ) ;
#29201 = ORIENTED_EDGE ( 'NONE', *, *, #29829, .F. ) ;
#29202 = COLOUR_RGB ( '', 0.40784314, 0.44705882, 0.49803922) ;
#29203 = DIRECTION ( 'NONE',  ( 1.522745436688331916E-06, -7.096186242782870827E-06, 0.9999999999736625123 ) ) ;
#29204 = CARTESIAN_POINT ( 'NONE',  ( -19.47326719839287890, -21.50389106269314965, 65.53656487971998956 ) ) ;
#29205 = CARTESIAN_POINT ( 'NONE',  ( -24.42338697892460075, -14.97596148503881786, 59.47130019869695161 ) ) ;
#29206 = CARTESIAN_POINT ( 'NONE',  ( -9.995192866514953423, -14.24820641570412683, 64.49529709569884517 ) ) ;
#29207 = AXIS2_PLACEMENT_3D ( 'NONE', #41346, #26097, #32741 ) ;
#29208 = ORIENTED_EDGE ( 'NONE', *, *, #29389, .F. ) ;
#29209 = CARTESIAN_POINT ( 'NONE',  ( 23.62590614458706639, -0.009252390952106800612, 50.53028072113869484 ) ) ;
#29210 = ADVANCED_FACE ( 'NONE', ( #32199 ), #40309, .T. ) ;
#29211 = CARTESIAN_POINT ( 'NONE',  ( -16.67409385541329669, -6.859212275519744217, 50.50378509014024075 ) ) ;
#29212 = LINE ( 'NONE', #43273, #22924 ) ;
#29213 = ORIENTED_EDGE ( 'NONE', *, *, #36586, .T. ) ;
#29214 = FACE_OUTER_BOUND ( 'NONE', #3360, .T. ) ;
#29215 = DIRECTION ( 'NONE',  ( 5.329554274754248866E-07, 1.313503380136696700E-06, 0.9999999999989952482 ) ) ;
#29216 = DIRECTION ( 'NONE',  ( -0.9345716196833626643, 0.3557750520798445559, 2.412542607589989711E-09 ) ) ;
#29217 = ORIENTED_EDGE ( 'NONE', *, *, #8665, .F. ) ;
#29218 = CARTESIAN_POINT ( 'NONE',  ( -14.86359179994916246, -21.80616968373489684, 65.29251951080507865 ) ) ;
#29219 = VERTEX_POINT ( 'NONE', #43530 ) ;
#29220 = CARTESIAN_POINT ( 'NONE',  ( -10.99582063857411995, -11.91441743271276188, 74.55840195587596497 ) ) ;
#29221 = CARTESIAN_POINT ( 'NONE',  ( -13.70160630012599157, -20.73736701164767027, 61.62532223698378431 ) ) ;
#29222 = CARTESIAN_POINT ( 'NONE',  ( -24.41778221492472412, -14.51057486539872876, 62.93969914534589094 ) ) ;
#29223 = LINE ( 'NONE', #44260, #730 ) ;
#29224 = ORIENTED_EDGE ( 'NONE', *, *, #25902, .F. ) ;
#29225 = DIRECTION ( 'NONE',  ( -3.071710424422018668E-17, 6.404604876783312462E-16, 1.000000000000000000 ) ) ;
#29226 = CARTESIAN_POINT ( 'NONE',  ( -24.17899325218984785, -11.66673737571591296, 59.66731058339561855 ) ) ;
#29227 = CARTESIAN_POINT ( 'NONE',  ( -23.30282546666849086, -18.60927426030231047, 69.59371984657600763 ) ) ;
#29228 = ORIENTED_EDGE ( 'NONE', *, *, #1090, .F. ) ;
#29229 = CARTESIAN_POINT ( 'NONE',  ( -9.982647249627337516, -14.45068338159927990, 68.11446040317247252 ) ) ;
#29230 = FACE_OUTER_BOUND ( 'NONE', #9394, .T. ) ;
#29232 = VERTEX_POINT ( 'NONE', #48173 ) ;
#29231 = AXIS2_PLACEMENT_3D ( 'NONE', #3466, #29089, #17988 ) ;
#29233 = ORIENTED_EDGE ( 'NONE', *, *, #44320, .F. ) ;
#29234 = CARTESIAN_POINT ( 'NONE',  ( -15.28965001900414755, -21.53148179447737220, 64.99108044553886998 ) ) ;
#29235 = EDGE_CURVE ( 'NONE', #14018, #26370, #22120, .T. ) ;
#29236 = CARTESIAN_POINT ( 'NONE',  ( -13.10977233404386944, -20.39504592733330313, 58.19083229533344337 ) ) ;
#29237 =( BOUNDED_CURVE ( )  B_SPLINE_CURVE ( 3, ( #46262, #32213, #43301, #43046 ),
 .UNSPECIFIED., .F., .F. ) 
 B_SPLINE_CURVE_WITH_KNOTS ( ( 4, 4 ),
 ( 0.5000000000000000000, 0.9074455897393632897 ),
 .UNSPECIFIED. ) 
 CURVE ( )  GEOMETRIC_REPRESENTATION_ITEM ( )  RATIONAL_B_SPLINE_CURVE ( ( 0.9999999999999968914, 0.4567392136813324122, 0.3561768502900325428, 0.6983129098260938417 ) ) 
 REPRESENTATION_ITEM ( '' )  );
#29238 = FACE_OUTER_BOUND ( 'NONE', #8712, .T. ) ;
#29239 = CARTESIAN_POINT ( 'NONE',  ( -19.48861532486628434, -21.49789759945147694, 62.01006052078847119 ) ) ;
#29240 = LINE ( 'NONE', #40549, #39307 ) ;
#29241 = CARTESIAN_POINT ( 'NONE',  ( -11.25989573505624364, -11.38792594226331190, 64.14882039369129529 ) ) ;
#29242 = CARTESIAN_POINT ( 'NONE',  ( -12.82409385759799036, -9.359200813967568422, 50.49621490985803263 ) ) ;
#29243 = EDGE_LOOP ( 'NONE', ( #22308, #28744 ) ) ;
#29244 = ORIENTED_EDGE ( 'NONE', *, *, #33209, .F. ) ;
#29245 = ADVANCED_FACE ( 'NONE', ( #10024 ), #25050, .F. ) ;
#29247 = CARTESIAN_POINT ( 'NONE',  ( -23.70135487130767515, -11.71146637837649074, 63.25218278684473461 ) ) ;
#29246 = CIRCLE ( 'NONE', #2490, 1.250000000000001110 ) ;
#29248 = CIRCLE ( 'NONE', #12726, 0.4000000000000011879 ) ;
#29249 = CARTESIAN_POINT ( 'NONE',  ( -19.99112905230247961, -8.296885111154901793, 73.72096600045514947 ) ) ;
#29250 = CARTESIAN_POINT ( 'NONE',  ( -23.68653687815194786, -11.57061008776568123, 66.43686604568146947 ) ) ;
#29251 = CARTESIAN_POINT ( 'NONE',  ( -10.97672180207948145, -17.53854803984884470, 71.63888375208067316 ) ) ;
#29252 = EDGE_CURVE ( 'NONE', #18613, #38614, #7184, .T. ) ;
#29253 = CARTESIAN_POINT ( 'NONE',  ( -12.18836193727821460, -19.53083876418623532, 57.94154444592973618 ) ) ;
#29254 = EDGE_LOOP ( 'NONE', ( #39808, #10186 ) ) ;
#29255 = CARTESIAN_POINT ( 'NONE',  ( -19.48659385650551457, -9.302874398569244363, 51.68646062012417985 ) ) ;
#29256 = VERTEX_POINT ( 'NONE', #177 ) ;
#29257 = B_SPLINE_CURVE_WITH_KNOTS ( 'NONE', 1,
 ( #16835, #19578 ),
 .UNSPECIFIED., .F., .F.,
 ( 2, 2 ),
 ( 0.000000000000000000, 1.000000000000000000 ),
 .UNSPECIFIED. ) ;
#29258 = DIRECTION ( 'NONE',  ( -3.071710424422018668E-17, 6.404604876783312462E-16, 1.000000000000000000 ) ) ;
#29259 = DIRECTION ( 'NONE',  ( -2.866981220435666553E-17, 1.000000000000000000, 1.190614954331866791E-16 ) ) ;
#29260 = DIRECTION ( 'NONE',  ( 0.9687793358424817702, -0.2479245821708688791, 0.000000000000000000 ) ) ;
#29261 = CARTESIAN_POINT ( 'NONE',  ( -10.03035355355731006, -15.72374577095404824, 61.22284339518546403 ) ) ;
#29262 = EDGE_CURVE ( 'NONE', #28434, #38833, #40990, .T. ) ;
#29263 = ORIENTED_EDGE ( 'NONE', *, *, #32241, .T. ) ;
#29264 = ADVANCED_FACE ( 'NONE', ( #38056 ), #25697, .T. ) ;
#29265 = LINE ( 'NONE', #44299, #39302 ) ;
#29266 = EDGE_CURVE ( 'NONE', #42055, #8895, #42970, .T. ) ;
#29267 = CARTESIAN_POINT ( 'NONE',  ( -14.54749350918766204, -8.372447261038935551, 64.07506791522041567 ) ) ;
#29268 = EDGE_LOOP ( 'NONE', ( #7025, #734 ) ) ;
#29269 = EDGE_CURVE ( 'NONE', #8530, #31901, #4343, .T. ) ;
#29270 = CARTESIAN_POINT ( 'NONE',  ( -14.05371270701021480, -21.00138147690670820, 71.92607703580546286 ) ) ;
#29271 = CARTESIAN_POINT ( 'NONE',  ( -24.12044147510846059, -12.60386701182102698, 73.24785355581104795 ) ) ;
#29272 = EDGE_LOOP ( 'NONE', ( #2740, #17832, #14684, #34128, #15432 ) ) ;
#29273 = CARTESIAN_POINT ( 'NONE',  ( -43.14308517176575464, -25.10920654474410441, 57.24806946917839667 ) ) ;
#29274 = VERTEX_POINT ( 'NONE', #33880 ) ;
#29275 = FACE_OUTER_BOUND ( 'NONE', #24323, .T. ) ;
#29276 = FACE_OUTER_BOUND ( 'NONE', #45554, .T. ) ;
#29277 = ORIENTED_EDGE ( 'NONE', *, *, #10924, .T. ) ;
#29278 = CARTESIAN_POINT ( 'NONE',  ( -13.71897584585257235, -21.27267513736575566, 68.57812350262666712 ) ) ;
#29279 = DIRECTION ( 'NONE',  ( -0.9893521221787096032, 0.1455416721783832079, 6.188545272020285247E-08 ) ) ;
#29280 = ORIENTED_EDGE ( 'NONE', *, *, #18242, .T. ) ;
#29281 = CARTESIAN_POINT ( 'NONE',  ( -18.84910040211995863, -7.954480482427757515, 70.44238404915014939 ) ) ;
#29282 =( BOUNDED_CURVE ( )  B_SPLINE_CURVE ( 3, ( #4570, #23294, #27943, #38279 ),
 .UNSPECIFIED., .F., .F. ) 
 B_SPLINE_CURVE_WITH_KNOTS ( ( 4, 4 ),
 ( 0.4074455897393617909, 0.5000000000000000000 ),
 .UNSPECIFIED. ) 
 CURVE ( )  GEOMETRIC_REPRESENTATION_ITEM ( )  RATIONAL_B_SPLINE_CURVE ( ( 0.6983129098260847378, 0.7760317562606787734, 0.8765941196519803080, 0.9999999999999805711 ) ) 
 REPRESENTATION_ITEM ( '' )  );
#29283 = CARTESIAN_POINT ( 'NONE',  ( -11.11225360959527819, -18.76719628086529212, 61.43744160855001013 ) ) ;
#29284 = CARTESIAN_POINT ( 'NONE',  ( -22.01964724813734620, -15.72799447708766962, 49.52966884056655772 ) ) ;
#29285 = ORIENTED_EDGE ( 'NONE', *, *, #37063, .T. ) ;
#29286 = DIRECTION ( 'NONE',  ( 0.9687793358424819923, -0.2479245821708680464, 0.000000000000000000 ) ) ;
#29287 = LINE ( 'NONE', #10340, #46388 ) ;
#29288 = DIRECTION ( 'NONE',  ( 1.000000000000000000, 2.866981220435666553E-17, 0.000000000000000000 ) ) ;
#29289 = ORIENTED_EDGE ( 'NONE', *, *, #15596, .F. ) ;
#29290 = ORIENTED_EDGE ( 'NONE', *, *, #19436, .F. ) ;
#29291 = CARTESIAN_POINT ( 'NONE',  ( -23.38871250174943839, -10.34516057075380679, 59.72486561860700505 ) ) ;
#29292 = CARTESIAN_POINT ( 'NONE',  ( -16.85710124362929463, -7.832207225656589777, 74.15121474590814898 ) ) ;
#29293 = CARTESIAN_POINT ( 'NONE',  ( -16.48034385759799036, -9.360768649639302552, 51.01397948905922419 ) ) ;
#29294 = CARTESIAN_POINT ( 'NONE',  ( -22.71334156758821265, -10.13600392596141475, 63.22752948238618842 ) ) ;
#29295 = CARTESIAN_POINT ( 'NONE',  ( -13.28240554951661245, -9.100331501070346718, 67.79431631125400770 ) ) ;
#29296 = CARTESIAN_POINT ( 'NONE',  ( -23.70782535920394452, -18.81166901052139551, 69.43225427700679120 ) ) ;
#29297 =( BOUNDED_CURVE ( )  B_SPLINE_CURVE ( 3, ( #26769, #907, #27482, #34372 ),
 .UNSPECIFIED., .F., .F. ) 
 B_SPLINE_CURVE_WITH_KNOTS ( ( 4, 4 ),
 ( 1.570796326794896780, 1.780235837034217283 ),
 .UNSPECIFIED. ) 
 CURVE ( )  GEOMETRIC_REPRESENTATION_ITEM ( )  RATIONAL_B_SPLINE_CURVE ( ( 1.000000000000000000, 0.9963479302455154896, 0.9963479302455154896, 1.000000000000000000 ) ) 
 REPRESENTATION_ITEM ( '' )  );
#29298 = FACE_OUTER_BOUND ( 'NONE', #8293, .T. ) ;
#29299 = ORIENTED_EDGE ( 'NONE', *, *, #21303, .T. ) ;
#29300 = EDGE_CURVE ( 'NONE', #4669, #35358, #22081, .T. ) ;
#29301 = CARTESIAN_POINT ( 'NONE',  ( 0.000000000000000000, 0.000000000000000000, 0.000000000000000000 ) ) ;
#29302 = EDGE_CURVE ( 'NONE', #6531, #42275, #44907, .T. ) ;
#29303 = CARTESIAN_POINT ( 'NONE',  ( -11.64902330566212463, -10.02396254413167576, 54.27966884056655061 ) ) ;
#29304 = ORIENTED_EDGE ( 'NONE', *, *, #37540, .F. ) ;
#29305 =( BOUNDED_SURFACE ( )  B_SPLINE_SURFACE ( 3, 1, ( 
 ( #14742, #48030 ),
 ( #36670, #25386 ),
 ( #41131, #3212 ),
 ( #41365, #10380 ),
 ( #11341, #22181 ),
 ( #32986, #29811 ),
 ( #22415, #44586 ) ),
 .UNSPECIFIED., .T., .F., .F. ) 
 B_SPLINE_SURFACE_WITH_KNOTS ( ( 4, 3, 4 ),
 ( 2, 2 ),
 ( 0.000000000000000000, 0.5000000000000000000, 1.000000000000000000 ),
 ( 0.000000000000000000, 1.000000000000000000 ),
 .UNSPECIFIED. ) 
 GEOMETRIC_REPRESENTATION_ITEM ( )  RATIONAL_B_SPLINE_SURFACE ( (
 ( 1.000000000000000000, 1.000000000000000000),
 ( 0.3333333333333335369, 0.3333333333333330373),
 ( 0.3333333333333335369, 0.3333333333333330373),
 ( 1.000000000000000000, 1.000000000000000000),
 ( 0.3333333333333333703, 0.3333333333333333703),
 ( 0.3333333333333333703, 0.3333333333333333703),
 ( 1.000000000000000000, 1.000000000000000000) ) ) 
 REPRESENTATION_ITEM ( '' )  SURFACE ( )  );
#29306 = ORIENTED_EDGE ( 'NONE', *, *, #10569, .F. ) ;
#29307 = LINE ( 'NONE', #10834, #20183 ) ;
#29308 = CARTESIAN_POINT ( 'NONE',  ( -24.46146587544552276, -14.38248120490118787, 66.46820668217904426 ) ) ;
#29309 = CARTESIAN_POINT ( 'NONE',  ( -23.92344128327244590, -11.16753467582692672, 69.99936603959443460 ) ) ;
#29310 = CARTESIAN_POINT ( 'NONE',  ( -11.63532267033605372, -18.83847007233952908, 72.10174756685907482 ) ) ;
#29311 = ORIENTED_EDGE ( 'NONE', *, *, #33305, .F. ) ;
#29312 = EDGE_CURVE ( 'NONE', #43753, #43742, #19351, .T. ) ;
#29313 = CARTESIAN_POINT ( 'NONE',  ( -18.63018970549565978, -7.457396494496333794, 73.95569010969242640 ) ) ;
#29314 = B_SPLINE_CURVE_WITH_KNOTS ( 'NONE', 3,
 ( #25068, #22336, #6595, #48677, #18382, #14421, #11015, #47706, #6352, #6830 ),
 .UNSPECIFIED., .F., .F.,
 ( 4, 2, 2, 2, 4 ),
 ( 0.1272669073658570793, 0.2522669073463325029, 0.3772669073268078987, 0.5022669073072834056, 0.6272669072877588015 ),
 .UNSPECIFIED. ) ;
#29315 = CARTESIAN_POINT ( 'NONE',  ( -15.03931914688375571, -19.48631565075837457, 52.02966884056656482 ) ) ;
#29316 = EDGE_CURVE ( 'NONE', #14945, #44591, #14986, .T. ) ;
#29317 = EDGE_CURVE ( 'NONE', #35836, #93, #41519, .T. ) ;
#29318 = EDGE_CURVE ( 'NONE', #14220, #17691, #37200, .T. ) ;
#29319 = ORIENTED_EDGE ( 'NONE', *, *, #26740, .F. ) ;
#29320 = CARTESIAN_POINT ( 'NONE',  ( -13.65110067086344792, -21.23324738024127356, 68.57129742521463811 ) ) ;
#29321 = CARTESIAN_POINT ( 'NONE',  ( -19.69914571794098990, -21.90346627284599634, 65.58769322485436248 ) ) ;
#29322 = CARTESIAN_POINT ( 'NONE',  ( -24.76566745545338222, -16.07607805037886450, 66.31970875637813378 ) ) ;
#29323 = ORIENTED_EDGE ( 'NONE', *, *, #3535, .T. ) ;
#29324 = DIRECTION ( 'NONE',  ( 0.000000000000000000, 0.000000000000000000, 1.000000000000000000 ) ) ;
#29325 = ORIENTED_EDGE ( 'NONE', *, *, #14607, .T. ) ;
#29326 = CARTESIAN_POINT ( 'NONE',  ( -23.81973173699715574, -10.98832876278002502, 73.46919161870800963 ) ) ;
#29327 = CARTESIAN_POINT ( 'NONE',  ( -24.38867418725816805, -14.10591363164734524, 69.84378491695960633 ) ) ;
#29328 = VERTEX_POINT ( 'NONE', #411 ) ;
#29329 = CARTESIAN_POINT ( 'NONE',  ( -24.44689184067228638, -14.18710713894228270, 69.93803194250308763 ) ) ;
#29330 = CARTESIAN_POINT ( 'NONE',  ( -24.47354813883760016, -12.39902559715248032, 73.42720875634239519 ) ) ;
#29331 = AXIS2_PLACEMENT_3D ( 'NONE', #37528, #32868, #18087 ) ;
#29332 = CARTESIAN_POINT ( 'NONE',  ( -13.33852097861372421, -12.48893720396535478, 49.52966884056655772 ) ) ;
#29333 = CARTESIAN_POINT ( 'NONE',  ( -18.50162525266306091, -21.72577549820248421, 72.58510940979837756 ) ) ;
#29334 = CARTESIAN_POINT ( 'NONE',  ( -23.91010245674826251, -17.57297063409389537, 62.75888927877479517 ) ) ;
#29335 = DIRECTION ( 'NONE',  ( 0.000000000000000000, 1.000000000000000000, 0.000000000000000000 ) ) ;
#29336 = CARTESIAN_POINT ( 'NONE',  ( -23.96075645138428101, -17.45014240273063066, 65.94357239682317129 ) ) ;
#29337 = EDGE_LOOP ( 'NONE', ( #6539, #12064, #6619, #38668, #18713 ) ) ;
#29338 = CARTESIAN_POINT ( 'NONE',  ( -20.43185948505062299, -8.432683554863363184, 66.79576150497511833 ) ) ;
#29339 = CARTESIAN_POINT ( 'NONE',  ( -10.36816553299425792, -14.63937932467125691, 64.54370954096965818 ) ) ;
#29340 = CARTESIAN_POINT ( 'NONE',  ( -14.48682561153071902, -7.962540396457996827, 63.91261920127995211 ) ) ;
#29341 = CARTESIAN_POINT ( 'NONE',  ( -21.67230677980763431, -11.72453687863643523, 52.02966884056656482 ) ) ;
#29342 = CARTESIAN_POINT ( 'NONE',  ( -10.81476099607377961, -12.49952454704760996, 61.02683403436387977 ) ) ;
#29343 = CARTESIAN_POINT ( 'NONE',  ( -24.27720304158778575, -16.23785116329529643, 62.87712181919398802 ) ) ;
#29344 = ADVANCED_FACE ( 'NONE', ( #4115 ), #34357, .T. ) ;
#29345 = ORIENTED_EDGE ( 'NONE', *, *, #7275, .F. ) ;
#29346 = ORIENTED_EDGE ( 'NONE', *, *, #26458, .T. ) ;
#29347 = DIRECTION ( 'NONE',  ( 1.000000000000000000, -4.164305804376849172E-17, 1.614929280266638808E-16 ) ) ;
#29348 = CARTESIAN_POINT ( 'NONE',  ( -23.93648101794248362, -17.51022725521227841, 65.95829288617392194 ) ) ;
#29349 = ORIENTED_EDGE ( 'NONE', *, *, #20555, .F. ) ;
#29351 = CARTESIAN_POINT ( 'NONE',  ( -11.75134375414733334, -18.91116183774077797, 71.97069383046880375 ) ) ;
#29350 = CYLINDRICAL_SURFACE ( 'NONE', #45580, 5.249999999999998224 ) ;
#29352 = FACE_OUTER_BOUND ( 'NONE', #6977, .T. ) ;
#29353 = CARTESIAN_POINT ( 'NONE',  ( -10.64854695470030599, -12.86019059820356780, 64.55364013863997741 ) ) ;
#29354 = CARTESIAN_POINT ( 'NONE',  ( -12.05615996164320691, -19.97535249625256526, 61.51183308442717390 ) ) ;
#29355 = FACE_BOUND ( 'NONE', #20340, .T. ) ;
#29356 = CARTESIAN_POINT ( 'NONE',  ( -23.86426273889453498, -17.55550152358811999, 66.01527417605778680 ) ) ;
#29357 = CARTESIAN_POINT ( 'NONE',  ( -10.42297872178580853, -14.76125658070002622, 75.02608819853371358 ) ) ;
#29358 = DIRECTION ( 'NONE',  ( -8.419732596317119940E-06, 4.907637675873463559E-06, 0.9999999999525115424 ) ) ;
#29359 = ORIENTED_EDGE ( 'NONE', *, *, #36195, .T. ) ;
#29360 = DIRECTION ( 'NONE',  ( -0.8651630202045381690, 0.5014907262059381532, 5.433021001366390361E-08 ) ) ;
#29361 = CARTESIAN_POINT ( 'NONE',  ( -12.82409385759799036, -9.359200813967568422, 50.49621490985803263 ) ) ;
#29362 = ADVANCED_FACE ( 'NONE', ( #8776 ), #23548, .T. ) ;
#29363 = B_SPLINE_CURVE_WITH_KNOTS ( 'NONE', 3,
 ( #24881, #39894, #6166, #21191, #47763, #13999, #29053, #44100, #41345, #250 ),
 .UNSPECIFIED., .F., .F.,
 ( 4, 2, 2, 2, 4 ),
 ( 0.1272669073658642125, 0.2522669073439609555, 0.3772669073220577540, 0.5022669073001545526, 0.6272669072782512956 ),
 .UNSPECIFIED. ) ;
#29364 = CARTESIAN_POINT ( 'NONE',  ( -16.98991503782990975, -22.24662993548692214, 72.35038528954983406 ) ) ;
#29365 = DIRECTION ( 'NONE',  ( -3.071710424422018668E-17, 6.404604876783312462E-16, 1.000000000000000000 ) ) ;
#29366 = CARTESIAN_POINT ( 'NONE',  ( -21.62409385541304374, -9.359200813967568422, 50.49621490985803263 ) ) ;
#29367 = CARTESIAN_POINT ( 'NONE',  ( -14.91789657710648598, -21.40191547797545724, 58.05129291223532562 ) ) ;
#29368 = CARTESIAN_POINT ( 'NONE',  ( -20.96187357126569850, -17.88286835634646721, 52.02966884056656482 ) ) ;
#29369 = ORIENTED_EDGE ( 'NONE', *, *, #4430, .T. ) ;
#29370 = ORIENTED_EDGE ( 'NONE', *, *, #18095, .F. ) ;
#29371 = B_SPLINE_CURVE_WITH_KNOTS ( 'NONE', 3,
 ( #12652, #38505, #4787, #1313, #16324, #34812, #16084, #46146, #31366, #23991 ),
 .UNSPECIFIED., .F., .F.,
 ( 4, 2, 2, 2, 4 ),
 ( 0.6272669072877984364, 0.7522669073073017243, 0.8772669073268051232, 1.002266907346308411, 1.127266907365811699 ),
 .UNSPECIFIED. ) ;
#29372 = CARTESIAN_POINT ( 'NONE',  ( -15.71784385541304552, -6.860780111191487229, 51.02154966934377711 ) ) ;
#29373 = ORIENTED_EDGE ( 'NONE', *, *, #16635, .T. ) ;
#29374 = CYLINDRICAL_SURFACE ( 'NONE', #40564, 1.250000000000007994 ) ;
#29375 = CIRCLE ( 'NONE', #26239, 5.249999999999998224 ) ;
#29376 = CARTESIAN_POINT ( 'NONE',  ( -12.05806040642128707, -10.23620046216302448, 67.51368956197082127 ) ) ;
#29377 = CARTESIAN_POINT ( 'NONE',  ( 10.57590614458695377, 0.6407533398237006406, 50.52649563099625851 ) ) ;
#29378 = EDGE_CURVE ( 'NONE', #33946, #38947, #31658, .T. ) ;
#29379 = EDGE_CURVE ( 'NONE', #33854, #19106, #32872, .T. ) ;
#29380 = CARTESIAN_POINT ( 'NONE',  ( -15.54494036203377405, -7.599968873926485458, 70.73177050285754319 ) ) ;
#29381 = ORIENTED_EDGE ( 'NONE', *, *, #32710, .F. ) ;
#29382 = CARTESIAN_POINT ( 'NONE',  ( -13.88833677318074500, -20.91193151007171736, 64.87139997340349851 ) ) ;
#29383 = CARTESIAN_POINT ( 'NONE',  ( -12.42993038278122597, -9.833123725877770838, 57.08935529208049076 ) ) ;
#29384 = ORIENTED_EDGE ( 'NONE', *, *, #40346, .F. ) ;
#29385 = DIRECTION ( 'NONE',  ( 0.9956360040033426229, -0.09332174201254549162, 0.000000000000000000 ) ) ;
#29386 = DIRECTION ( 'NONE',  ( -6.919810407550069512E-06, -1.067025350021132924E-05, 0.9999999999191310218 ) ) ;
#29387 = VERTEX_POINT ( 'NONE', #46677 ) ;
#29388 = EDGE_CURVE ( 'NONE', #30767, #33361, #46482, .T. ) ;
#29389 = EDGE_CURVE ( 'NONE', #38508, #47624, #1651, .T. ) ;
#29390 = CARTESIAN_POINT ( 'NONE',  ( -10.93232766038821424, -17.55941949638709687, 68.38249893951126523 ) ) ;
#29391 = CARTESIAN_POINT ( 'NONE',  ( -12.14425517392406917, -10.13739710456042964, 64.17914326607970565 ) ) ;
#29392 = CARTESIAN_POINT ( 'NONE',  ( -23.00454255336054743, -10.50046069577333263, 59.88731295783226471 ) ) ;
#29393 = ORIENTED_EDGE ( 'NONE', *, *, #38286, .F. ) ;
#29394 = CARTESIAN_POINT ( 'NONE',  ( -20.18941624216641273, -7.891347737435665977, 73.83601159825586535 ) ) ;
#29395 = ADVANCED_FACE ( 'NONE', ( #1609 ), #15892, .F. ) ;
#29396 = LINE ( 'NONE', #32830, #43868 ) ;
#29397 = CARTESIAN_POINT ( 'NONE',  ( -13.85393650630732054, -8.270265118416840977, 74.38450092284953996 ) ) ;
#29398 = CARTESIAN_POINT ( 'NONE',  ( -23.91439714532632621, -17.43141235356291574, 65.94357239632037704 ) ) ;
#29399 = ORIENTED_EDGE ( 'NONE', *, *, #43452, .T. ) ;
#29400 = CARTESIAN_POINT ( 'NONE',  ( -15.65212752116712558, -9.867280269464723474, 49.52966884056655772 ) ) ;
#29401 = FACE_OUTER_BOUND ( 'NONE', #39868, .T. ) ;
#29402 = CARTESIAN_POINT ( 'NONE',  ( -16.39155704513022016, -21.78318439201321866, 61.75568132354042916 ) ) ;
#29403 = CARTESIAN_POINT ( 'NONE',  ( -11.64873123714592396, -10.76074834137913960, 74.32396018297762907 ) ) ;
#29404 = ADVANCED_FACE ( 'NONE', ( #30938 ), #45949, .F. ) ;
#29405 = VECTOR ( 'NONE', #30447, 1000.000000000000000 ) ;
#29406 = VERTEX_POINT ( 'NONE', #892 ) ;
#29407 = CARTESIAN_POINT ( 'NONE',  ( -24.19028598586675116, -12.80082241304059210, 62.98831023884616798 ) ) ;
#29408 = DIRECTION ( 'NONE',  ( -1.000000000000000000, -0.000000000000000000, 8.260587980841940012E-17 ) ) ;
#29409 = VERTEX_POINT ( 'NONE', #31406 ) ;
#29410 = FACE_OUTER_BOUND ( 'NONE', #20860, .T. ) ;
#29411 = CARTESIAN_POINT ( 'NONE',  ( -19.20714268997449281, -19.15619313305651161, 49.52966884056656482 ) ) ;
#29412 = CARTESIAN_POINT ( 'NONE',  ( -18.69922557824643761, -7.468382084482742655, 74.02719791125277027 ) ) ;
#29413 = ORIENTED_EDGE ( 'NONE', *, *, #15162, .T. ) ;
#29414 = LINE ( 'NONE', #47414, #42802 ) ;
#29415 = ORIENTED_EDGE ( 'NONE', *, *, #33556, .T. ) ;
#29416 = ORIENTED_EDGE ( 'NONE', *, *, #10402, .F. ) ;
#29417 = ORIENTED_EDGE ( 'NONE', *, *, #5545, .F. ) ;
#29418 = CARTESIAN_POINT ( 'NONE',  ( -17.79909385650551812, -8.114302828567740988, 52.18300498402516041 ) ) ;
#29419 = CARTESIAN_POINT ( 'NONE',  ( -18.81087689773607607, -7.489408793048438540, 70.57079237633290347 ) ) ;
#29420 = CARTESIAN_POINT ( 'NONE',  ( -50.42609385541305755, -14.80920654474415699, 62.02941176470587692 ) ) ;
#29421 = CARTESIAN_POINT ( 'NONE',  ( -13.38575581802539993, -9.030060914960570173, 60.72478133471773987 ) ) ;
#29422 = ORIENTED_EDGE ( 'NONE', *, *, #43293, .F. ) ;
#29423 = ORIENTED_EDGE ( 'NONE', *, *, #43427, .T. ) ;
#29424 = CARTESIAN_POINT ( 'NONE',  ( -19.91159385650551528, -6.922745924619793101, 51.69366785382590024 ) ) ;
#29425 = B_SPLINE_CURVE_WITH_KNOTS ( 'NONE', 1,
 ( #23340, #5115 ),
 .UNSPECIFIED., .F., .F.,
 ( 2, 2 ),
 ( 0.000000000000000000, 1.000000000000000000 ),
 .UNSPECIFIED. ) ;
#29426 = CARTESIAN_POINT ( 'NONE',  ( -11.48080861122161167, -10.31672956615889269, 74.60031634573793724 ) ) ;
#29427 = CARTESIAN_POINT ( 'NONE',  ( -12.23896285002386719, -13.98645721660588137, 52.02966884056656482 ) ) ;
#29428 =( BOUNDED_CURVE ( )  B_SPLINE_CURVE ( 3, ( #40053, #2619, #24795, #32424 ),
 .UNSPECIFIED., .F., .F. ) 
 B_SPLINE_CURVE_WITH_KNOTS ( ( 4, 4 ),
 ( 0.5000000000000000000, 0.9074455897393665094 ),
 .UNSPECIFIED. ) 
 CURVE ( )  GEOMETRIC_REPRESENTATION_ITEM ( )  RATIONAL_B_SPLINE_CURVE ( ( 1.000000000000025757, 0.4567392136813333003, 0.3561768502900126698, 0.6983129098260916212 ) ) 
 REPRESENTATION_ITEM ( '' )  );
#29429 = CARTESIAN_POINT ( 'NONE',  ( -19.23659385650551457, -6.915538690918075382, 49.31353937987644542 ) ) ;
#29430 = ORIENTED_EDGE ( 'NONE', *, *, #8261, .T. ) ;
#29431 = EDGE_CURVE ( 'NONE', #918, #38805, #10788, .T. ) ;
#29432 = CARTESIAN_POINT ( 'NONE',  ( -45.92409385541306222, -14.20920654474410760, 69.94400000000000261 ) ) ;
#29433 = CIRCLE ( 'NONE', #7457, 0.09999999999999939493 ) ;
#29434 = CARTESIAN_POINT ( 'NONE',  ( -18.50932193227059486, -21.77517953109191140, 72.58510940649487964 ) ) ;
#29435 = CARTESIAN_POINT ( 'NONE',  ( -24.41275629217255272, -14.38907661853721542, 69.88105113750283692 ) ) ;
#29436 = ORIENTED_EDGE ( 'NONE', *, *, #47131, .F. ) ;
#29437 = CARTESIAN_POINT ( 'NONE',  ( -24.72409385541305582, -14.80920654474411613, 58.90588235294116970 ) ) ;
#29438 =( BOUNDED_CURVE ( )  B_SPLINE_CURVE ( 3, ( #34991, #16261, #42154, #38438 ),
 .UNSPECIFIED., .F., .F. ) 
 B_SPLINE_CURVE_WITH_KNOTS ( ( 4, 4 ),
 ( 0.4074455897393596260, 0.5000000000000000000 ),
 .UNSPECIFIED. ) 
 CURVE ( )  GEOMETRIC_REPRESENTATION_ITEM ( )  RATIONAL_B_SPLINE_CURVE ( ( 0.6983129098260744128, 0.7760317562606953157, 0.8765941196520076195, 1.000000000000020872 ) ) 
 REPRESENTATION_ITEM ( '' )  );
#29439 = ORIENTED_EDGE ( 'NONE', *, *, #500, .F. ) ;
#29440 = EDGE_CURVE ( 'NONE', #41576, #10249, #37818, .T. ) ;
#29441 = CARTESIAN_POINT ( 'NONE',  ( -12.74141321320493958, -14.42442407569615348, 49.52966884056655772 ) ) ;
#29442 = DIRECTION ( 'NONE',  ( 0.9753750245375039096, 0.2205528542287732985, 7.244220459260265297E-08 ) ) ;
#29443 = CARTESIAN_POINT ( 'NONE',  ( -24.42383174400572088, -14.88139811306343496, 59.24300232022908830 ) ) ;
#29444 = CARTESIAN_POINT ( 'NONE',  ( -17.34909385541293858, -8.112991634885936776, 51.74999426922440193 ) ) ;
#29445 = EDGE_CURVE ( 'NONE', #5150, #23878, #37059, .T. ) ;
#29446 = VERTEX_POINT ( 'NONE', #46438 ) ;
#29447 = CARTESIAN_POINT ( 'NONE',  ( -10.31252162633752079, -12.58677457285831913, 60.91198276946202128 ) ) ;
#29448 = CARTESIAN_POINT ( 'NONE',  ( -24.21202825980905615, -11.73864819121529912, 59.60518815382388169 ) ) ;
#29449 = EDGE_CURVE ( 'NONE', #41197, #14597, #23792, .T. ) ;
#29450 = CARTESIAN_POINT ( 'NONE',  ( -11.25989573505624364, -11.38792594226331190, 64.14882039369129529 ) ) ;
#29451 = LINE ( 'NONE', #40770, #16603 ) ;
#29452 = VERTEX_POINT ( 'NONE', #42256 ) ;
#29453 = DIRECTION ( 'NONE',  ( 0.7915359335728471279, 0.6111226275167354061, 5.146443701300904349E-08 ) ) ;
#29454 = DIRECTION ( 'NONE',  ( -3.071710424422018668E-17, 6.404604876783312462E-16, 1.000000000000000000 ) ) ;
#29455 = CARTESIAN_POINT ( 'NONE',  ( -12.59783444659965390, -19.87951993436981368, 65.15209581050474696 ) ) ;
#29456 = ORIENTED_EDGE ( 'NONE', *, *, #40567, .F. ) ;
#29457 = FACE_BOUND ( 'NONE', #35225, .T. ) ;
#29458 = ORIENTED_EDGE ( 'NONE', *, *, #16884, .F. ) ;
#29459 = LINE ( 'NONE', #7805, #37600 ) ;
#29460 = LINE ( 'NONE', #2861, #9033 ) ;
#29461 = CARTESIAN_POINT ( 'NONE',  ( -24.72409385541305582, -14.80920654474423159, 69.97058823529410176 ) ) ;
#29462 = CARTESIAN_POINT ( 'NONE',  ( -4.424093855413056886, -25.10920654474410441, 47.99999999999998579 ) ) ;
#29463 = ORIENTED_EDGE ( 'NONE', *, *, #13423, .T. ) ;
#29464 = CARTESIAN_POINT ( 'NONE',  ( -10.47191917896302371, -13.98145069646090022, 60.98991602035415838 ) ) ;
#29465 = VERTEX_POINT ( 'NONE', #4576 ) ;
#29466 = CARTESIAN_POINT ( 'NONE',  ( -16.81468282041412010, -21.83654306051557015, 65.22564162490351691 ) ) ;
#29467 = CARTESIAN_POINT ( 'NONE',  ( -23.68653687815194786, -11.57061008776568123, 66.43686604568146947 ) ) ;
#29468 = VERTEX_POINT ( 'NONE', #46188 ) ;
#29469 = DIRECTION ( 'NONE',  ( -9.637352644315596475E-17, 0.000000000000000000, -1.000000000000000000 ) ) ;
#29470 = DIRECTION ( 'NONE',  ( -1.000000000000000000, -2.866981220435666553E-17, 0.000000000000000000 ) ) ;
#29471 = PRODUCT_DEFINITION ( 'UNKNOWN', '', #31393, #35146 ) ;
#29472 = AXIS2_PLACEMENT_3D ( 'NONE', #17227, #13046, #35461 ) ;
#29473 = ORIENTED_EDGE ( 'NONE', *, *, #48207, .T. ) ;
#29474 = ORIENTED_EDGE ( 'NONE', *, *, #5632, .T. ) ;
#29475 = CARTESIAN_POINT ( 'NONE',  ( -15.62301844010884899, -8.044815583578751372, 70.89524431202903543 ) ) ;
#29476 = CARTESIAN_POINT ( 'NONE',  ( -20.50783594841701785, -8.027295835816985914, 66.96599399791791996 ) ) ;
#29477 = DIRECTION ( 'NONE',  ( -3.071710424422018668E-17, 6.404604876783312462E-16, 1.000000000000000000 ) ) ;
#29478 = CARTESIAN_POINT ( 'NONE',  ( -16.57395829291861844, -22.21062093300318807, 65.26918445414273151 ) ) ;
#29479 = CARTESIAN_POINT ( 'NONE',  ( -12.37644160373227287, -19.65923220176213349, 61.69678630681026732 ) ) ;
#29480 = CARTESIAN_POINT ( 'NONE',  ( -16.13263948075386978, -7.878200451182638453, 63.68483172840383588 ) ) ;
#29481 = CARTESIAN_POINT ( 'NONE',  ( -22.83095763869631512, -19.93459457198476770, 72.82895875648904394 ) ) ;
#29482 = VERTEX_POINT ( 'NONE', #38794 ) ;
#29483 = EDGE_LOOP ( 'NONE', ( #46493, #3215, #5883, #4979, #15386 ) ) ;
#29484 = CARTESIAN_POINT ( 'NONE',  ( -13.25302027261275484, -9.121009434035636687, 60.64769990268487732 ) ) ;
#29485 = CARTESIAN_POINT ( 'NONE',  ( -23.09419775198653468, -9.976756388841243606, 66.64158628164071274 ) ) ;
#29486 = DIRECTION ( 'NONE',  ( -3.071710424422018668E-17, 6.404604876783312462E-16, 1.000000000000000000 ) ) ;
#29487 = CARTESIAN_POINT ( 'NONE',  ( -46.47622156840087371, -14.20920654474410760, 70.56550563755013172 ) ) ;
#29488 = CARTESIAN_POINT ( 'NONE',  ( -24.30048628764226137, -16.36411057843138650, 59.27332431757403697 ) ) ;
#29489 = EDGE_LOOP ( 'NONE', ( #18693, #43998, #9428, #42950, #34738 ) ) ;
#29490 = EDGE_CURVE ( 'NONE', #32198, #11365, #26988, .T. ) ;
#29491 = CARTESIAN_POINT ( 'NONE',  ( -17.79909385650551812, -8.114302828567740988, 52.18300498402516041 ) ) ;
#29492 = ORIENTED_EDGE ( 'NONE', *, *, #23693, .F. ) ;
#29493 = CARTESIAN_POINT ( 'NONE',  ( -13.52486571068042487, -17.40907233461224379, 52.02966884056656482 ) ) ;
#29494 = CARTESIAN_POINT ( 'NONE',  ( -12.09300774956044755, -19.42703681131052562, 58.34171032836335513 ) ) ;
#29495 = CARTESIAN_POINT ( 'NONE',  ( -10.73412848974934874, -11.53077067998621175, 71.20365450754333381 ) ) ;
#29496 = ORIENTED_EDGE ( 'NONE', *, *, #34772, .F. ) ;
#29497 = AXIS2_PLACEMENT_3D ( 'NONE', #29598, #48301, #40670 ) ;
#29498 = CARTESIAN_POINT ( 'NONE',  ( -23.34092575347512266, -10.28207967581048088, 59.78698817202694471 ) ) ;
#29499 = CARTESIAN_POINT ( 'NONE',  ( -17.42409385541299471, -14.80920654474435771, 49.52966884056655772 ) ) ;
#29500 = EDGE_CURVE ( 'NONE', #22230, #36064, #29542, .T. ) ;
#29501 = ORIENTED_EDGE ( 'NONE', *, *, #12060, .F. ) ;
#29502 = CARTESIAN_POINT ( 'NONE',  ( -16.97946044980448121, -21.84517136462328324, 72.31543221430108304 ) ) ;
#29503 = EDGE_CURVE ( 'NONE', #39013, #773, #21965, .T. ) ;
#29504 = CARTESIAN_POINT ( 'NONE',  ( -10.11977905767481900, -16.27558856157159539, 71.55476250049129305 ) ) ;
#29505 = ORIENTED_EDGE ( 'NONE', *, *, #11881, .F. ) ;
#29506 = DIRECTION ( 'NONE',  ( 0.9375570856950865561, -0.3478314405900308492, 0.000000000000000000 ) ) ;
#29507 = ORIENTED_EDGE ( 'NONE', *, *, #39407, .T. ) ;
#29508 = CARTESIAN_POINT ( 'NONE',  ( -23.87460028475566887, -17.65420844160683700, 62.47360984062320455 ) ) ;
#29509 = PRODUCT_DEFINITION_SHAPE ( 'NONE', 'NONE',  #16217 ) ;
#29510 = FACE_OUTER_BOUND ( 'NONE', #35131, .T. ) ;
#29511 = ADVANCED_FACE ( 'NONE', ( #24528 ), #10465, .T. ) ;
#29512 = VERTEX_POINT ( 'NONE', #13642 ) ;
#29513 = CARTESIAN_POINT ( 'NONE',  ( -23.97789761167216938, -17.40771579525701895, 66.23797482430366301 ) ) ;
#29514 = DIRECTION ( 'NONE',  ( -3.071710424422018668E-17, 6.404604876783312462E-16, 1.000000000000000000 ) ) ;
#29515 = VERTEX_POINT ( 'NONE', #39762 ) ;
#29516 = DIRECTION ( 'NONE',  ( -0.000000000000000000, -0.000000000000000000, 1.000000000000000000 ) ) ;
#29517 =( BOUNDED_SURFACE ( )  B_SPLINE_SURFACE ( 3, 1, ( 
 ( #32451, #21128 ),
 ( #2646, #6347 ),
 ( #25063, #39832 ),
 ( #47477, #25534 ),
 ( #43782, #21844 ),
 ( #17655, #10290 ),
 ( #18134, #33385 ) ),
 .UNSPECIFIED., .T., .F., .F. ) 
 B_SPLINE_SURFACE_WITH_KNOTS ( ( 4, 3, 4 ),
 ( 2, 2 ),
 ( 0.000000000000000000, 0.5000000000000000000, 1.000000000000000000 ),
 ( 0.000000000000000000, 1.000000000000000000 ),
 .UNSPECIFIED. ) 
 GEOMETRIC_REPRESENTATION_ITEM ( )  RATIONAL_B_SPLINE_SURFACE ( (
 ( 1.000000000000000000, 1.000000000000000000),
 ( 0.3333333333333335369, 0.3333333333333330373),
 ( 0.3333333333333335369, 0.3333333333333330373),
 ( 1.000000000000000000, 1.000000000000000000),
 ( 0.3333333333333333703, 0.3333333333333333703),
 ( 0.3333333333333333703, 0.3333333333333333703),
 ( 1.000000000000000000, 1.000000000000000000) ) ) 
 REPRESENTATION_ITEM ( '' )  SURFACE ( )  );
#29518 = ADVANCED_FACE ( 'NONE', ( #6030 ), #21054, .T. ) ;
#29519 = CARTESIAN_POINT ( 'NONE',  ( -11.07866493849470579, -18.71282305161091486, 61.37736592674749403 ) ) ;
#29520 = CARTESIAN_POINT ( 'NONE',  ( -23.46013293835336100, -11.16077341686890989, 69.77721965307074470 ) ) ;
#29521 = ORIENTED_EDGE ( 'NONE', *, *, #3154, .T. ) ;
#29522 = CARTESIAN_POINT ( 'NONE',  ( -24.61605457543312525, -12.86511826566283290, 66.41751344402152313 ) ) ;
#29523 = EDGE_CURVE ( 'NONE', #28707, #10899, #3050, .T. ) ;
#29524 = B_SPLINE_CURVE_WITH_KNOTS ( 'NONE', 3,
 ( #32362, #35305, #17062, #42945, #42717, #36024, #39252, #47132, #5533, #20554 ),
 .UNSPECIFIED., .F., .F.,
 ( 4, 2, 2, 2, 4 ),
 ( 0.000000000000000000, 0.2500000000000000000, 0.5000000000000000000, 0.7500000000000000000, 1.000000000000000000 ),
 .UNSPECIFIED. ) ;
#29525 = CARTESIAN_POINT ( 'NONE',  ( -24.03992722153932959, -17.24514946215870381, 69.71339794702862491 ) ) ;
#29526 = CYLINDRICAL_SURFACE ( 'NONE', #22443, 1.000000000000000888 ) ;
#29527 = EDGE_LOOP ( 'NONE', ( #15831, #26148, #38770, #10404 ) ) ;
#29528 = VERTEX_POINT ( 'NONE', #18063 ) ;
#29529 = CARTESIAN_POINT ( 'NONE',  ( -23.39264018726221650, -10.35034530683095078, 59.76349971690503082 ) ) ;
#29530 = CARTESIAN_POINT ( 'NONE',  ( -11.88369906670657628, -10.53078588752935651, 71.25427731142369225 ) ) ;
#29531 = CARTESIAN_POINT ( 'NONE',  ( -10.81170448216924740, -12.36318809540519048, 57.34329390664808557 ) ) ;
#29532 = CARTESIAN_POINT ( 'NONE',  ( -15.13034385759799250, -6.857644439848013640, 49.98602051094139398 ) ) ;
#29533 = CARTESIAN_POINT ( 'NONE',  ( -15.81235419205221504, -7.945607373518417837, 67.42535135806457447 ) ) ;
#29534 = CARTESIAN_POINT ( 'NONE',  ( -13.87299615820197296, -20.90301826156740717, 72.34096506744559463 ) ) ;
#29535 = CARTESIAN_POINT ( 'NONE',  ( -19.04853579327176760, -7.948602568230340282, 63.71617106789811658 ) ) ;
#29536 = CARTESIAN_POINT ( 'NONE',  ( -14.66287647794328386, -8.376693760123846033, 64.08978834288900828 ) ) ;
#29537 = AXIS2_PLACEMENT_3D ( 'NONE', #24887, #35950, #16749 ) ;
#29538 = EDGE_LOOP ( 'NONE', ( #34026, #47851, #15644, #13255 ) ) ;
#29539 = CARTESIAN_POINT ( 'NONE',  ( -24.31986544270498030, -13.34244042609839198, 59.36267955695507226 ) ) ;
#29540 = CARTESIAN_POINT ( 'NONE',  ( -22.26799053462541522, -13.56958363389006905, 52.02966884056655061 ) ) ;
#29541 = DIRECTION ( 'NONE',  ( -3.071710424422018668E-17, 6.404604876783312462E-16, 1.000000000000000000 ) ) ;
#29542 = B_SPLINE_CURVE_WITH_KNOTS ( 'NONE', 3,
 ( #5075, #20082, #35088, #12693, #42744, #21775, #28921, #40012, #36761, #47162 ),
 .UNSPECIFIED., .F., .F.,
 ( 4, 2, 2, 2, 4 ),
 ( 0.000000000000000000, 0.2500000000000000000, 0.5000000000000000000, 0.7500000000000000000, 1.000000000000000000 ),
 .UNSPECIFIED. ) ;
#29543 = EDGE_CURVE ( 'NONE', #47790, #30264, #19613, .T. ) ;
#29544 = ORIENTED_EDGE ( 'NONE', *, *, #43249, .F. ) ;
#29545 = VERTEX_POINT ( 'NONE', #39524 ) ;
#29546 = CARTESIAN_POINT ( 'NONE',  ( -22.75539019595754908, -10.19575032747719412, 66.82710158566565894 ) ) ;
#29547 = SURFACE_SIDE_STYLE ('',( #44345 ) ) ;
#29548 = CARTESIAN_POINT ( 'NONE',  ( -17.42409385541305511, -14.80920654474410725, 47.99999999999998579 ) ) ;
#29549 = CARTESIAN_POINT ( 'NONE',  ( -13.43921408130402817, -8.993432070331126127, 60.73950277491898930 ) ) ;
#29550 = ORIENTED_EDGE ( 'NONE', *, *, #7922, .T. ) ;
#29551 = EDGE_CURVE ( 'NONE', #23975, #45444, #34247, .T. ) ;
#29552 = CARTESIAN_POINT ( 'NONE',  ( -24.48935351541090455, -12.44598921085947119, 73.34251321892850228 ) ) ;
#29553 = CARTESIAN_POINT ( 'NONE',  ( -11.35974425695043699, -11.20802616635808313, 64.56370858977317084 ) ) ;
#29554 = ORIENTED_EDGE ( 'NONE', *, *, #36056, .F. ) ;
#29555 = FACE_OUTER_BOUND ( 'NONE', #47000, .T. ) ;
#29556 = CARTESIAN_POINT ( 'NONE',  ( -21.99019323879806365, -13.75373571565882536, 52.02966884056656482 ) ) ;
#29557 =( BOUNDED_CURVE ( )  B_SPLINE_CURVE ( 3, ( #31477, #8594, #46021, #16923 ),
 .UNSPECIFIED., .F., .F. ) 
 B_SPLINE_CURVE_WITH_KNOTS ( ( 4, 4 ),
 ( 0.000000000000000000, 0.4074455897393656767 ),
 .UNSPECIFIED. ) 
 CURVE ( )  GEOMETRIC_REPRESENTATION_ITEM ( )  RATIONAL_B_SPLINE_CURVE ( ( 1.000000000000000000, 0.4567392136813333003, 0.3561768502900307665, 0.6983129098260923984 ) ) 
 REPRESENTATION_ITEM ( '' )  );
#29558 = FACE_OUTER_BOUND ( 'NONE', #22027, .T. ) ;
#29559 = ORIENTED_EDGE ( 'NONE', *, *, #1190, .F. ) ;
#29560 = CARTESIAN_POINT ( 'NONE',  ( -11.87166626389854329, -10.45903512182793982, 67.70716783823823448 ) ) ;
#29561 = VECTOR ( 'NONE', #38877, 1000.000000000000000 ) ;
#29562 = ORIENTED_EDGE ( 'NONE', *, *, #8208, .F. ) ;
#29563 = CARTESIAN_POINT ( 'NONE',  ( -23.79882860864043082, -10.95363794417970738, 73.46169666061963710 ) ) ;
#29564 = ADVANCED_FACE ( 'NONE', ( #43229 ), #26871, .F. ) ;
#29565 = CARTESIAN_POINT ( 'NONE',  ( -19.67760665824181388, -21.48965406232008490, 65.75014118398131302 ) ) ;
#29566 = ORIENTED_EDGE ( 'NONE', *, *, #32718, .T. ) ;
#29567 = CARTESIAN_POINT ( 'NONE',  ( -21.38142803800936420, -21.12127404432104072, 69.15475944846217260 ) ) ;
#29568 = CARTESIAN_POINT ( 'NONE',  ( -19.38509533341928659, -21.58113884793795378, 62.00063448590932325 ) ) ;
#29569 = CARTESIAN_POINT ( 'NONE',  ( -21.99284385650551243, -7.406986770994972602, 48.81910596585309747 ) ) ;
#29570 = EDGE_CURVE ( 'NONE', #43757, #22495, #5804, .T. ) ;
#29571 = CARTESIAN_POINT ( 'NONE',  ( -17.42409385541299471, -14.80920654474435771, 49.52966884056655772 ) ) ;
#29572 = EDGE_CURVE ( 'NONE', #34971, #6268, #2690, .T. ) ;
#29573 = CARTESIAN_POINT ( 'NONE',  ( -24.23700366861210753, -17.82382531738836562, 62.73006892227505915 ) ) ;
#29574 = CARTESIAN_POINT ( 'NONE',  ( -42.05571150247188683, -14.90920654474419038, 65.94705882352940307 ) ) ;
#29575 = CARTESIAN_POINT ( 'NONE',  ( -10.42496409221358178, -14.69883174549087279, 71.32782692796889989 ) ) ;
#29576 = EDGE_LOOP ( 'NONE', ( #30096, #15335, #29933, #24801, #43674 ) ) ;
#29578 = CARTESIAN_POINT ( 'NONE',  ( -46.33910710821349710, -14.20920654474410760, 70.13000000000000966 ) ) ;
#29577 =( BOUNDED_CURVE ( )  B_SPLINE_CURVE ( 3, ( #37443, #3736, #6944, #40429 ),
 .UNSPECIFIED., .F., .F. ) 
 B_SPLINE_CURVE_WITH_KNOTS ( ( 4, 4 ),
 ( 0.9074455897393668424, 1.000000000000000000 ),
 .UNSPECIFIED. ) 
 CURVE ( )  GEOMETRIC_REPRESENTATION_ITEM ( )  RATIONAL_B_SPLINE_CURVE ( ( 0.6983129098260837386, 0.7760317562606902086, 0.8765941196519956291, 1.000000000000000000 ) ) 
 REPRESENTATION_ITEM ( '' )  );
#29579 = CARTESIAN_POINT ( 'NONE',  ( -16.13432406759100601, -21.74052631579560568, 58.30057715624173653 ) ) ;
#29580 = CARTESIAN_POINT ( 'NONE',  ( -14.47196271362616748, -7.969019419113326563, 63.98317130198068270 ) ) ;
#29581 = CYLINDRICAL_SURFACE ( 'NONE', #41536, 2.000000000000003109 ) ;
#29582 = CARTESIAN_POINT ( 'NONE',  ( -17.42409385541299471, -14.80920654474435771, 49.52966884056655772 ) ) ;
#29583 = DIRECTION ( 'NONE',  ( -0.9956360040033419567, 0.09332174201255252766, 0.000000000000000000 ) ) ;
#29584 = ORIENTED_EDGE ( 'NONE', *, *, #16130, .T. ) ;
#29585 = ORIENTED_EDGE ( 'NONE', *, *, #34543, .F. ) ;
#29586 = CARTESIAN_POINT ( 'NONE',  ( -16.98261326800368209, -21.79527086262147861, 72.16543221550985265 ) ) ;
#29587 = CARTESIAN_POINT ( 'NONE',  ( -9.975810198805103113, -14.64163036238288740, 71.46749302621661570 ) ) ;
#29588 = ORIENTED_EDGE ( 'NONE', *, *, #5333, .F. ) ;
#29590 = CARTESIAN_POINT ( 'NONE',  ( -11.70868095541711540, -18.85353058150503713, 71.79759075073991426 ) ) ;
#29589 = CARTESIAN_POINT ( 'NONE',  ( -23.99312320239454976, -11.29471777418100231, 66.60709819448160829 ) ) ;
#29591 = CARTESIAN_POINT ( 'NONE',  ( -13.38575581802539993, -9.030060914960570173, 60.72478133471773276 ) ) ;
#29592 = CARTESIAN_POINT ( 'NONE',  ( -11.57425499491753307, -18.65360305739656610, 64.74707076836355668 ) ) ;
#29593 = DIRECTION ( 'NONE',  ( -3.071710424422018668E-17, 6.404604876783312462E-16, 1.000000000000000000 ) ) ;
#29594 = EDGE_CURVE ( 'NONE', #93, #7630, #47410, .T. ) ;
#29595 = CARTESIAN_POINT ( 'NONE',  ( -11.21150076820731378, -18.14943614556009166, 57.89894789413084197 ) ) ;
#29596 = CARTESIAN_POINT ( 'NONE',  ( -17.65006842549283306, -20.30456235612523841, 54.07175714974878389 ) ) ;
#29597 = EDGE_CURVE ( 'NONE', #8440, #17754, #28428, .T. ) ;
#29598 = CARTESIAN_POINT ( 'NONE',  ( -17.42409385541299471, -14.80920654474435771, 49.52966884056655772 ) ) ;
#29599 =( BOUNDED_CURVE ( )  B_SPLINE_CURVE ( 3, ( #2272, #27651, #2030, #20265 ),
 .UNSPECIFIED., .F., .F. ) 
 B_SPLINE_CURVE_WITH_KNOTS ( ( 4, 4 ),
 ( 0.4074455897393683412, 0.5000000000000000000 ),
 .UNSPECIFIED. ) 
 CURVE ( )  GEOMETRIC_REPRESENTATION_ITEM ( )  RATIONAL_B_SPLINE_CURVE ( ( 0.6983129098260890677, 0.7760317562606889874, 0.8765941196519907441, 0.9999999999999906741 ) ) 
 REPRESENTATION_ITEM ( '' )  );
#29600 = CARTESIAN_POINT ( 'NONE',  ( -18.34560609025200861, -9.386954687716537293, 53.49999999999995026 ) ) ;
#29601 = EDGE_CURVE ( 'NONE', #31901, #23884, #6086, .T. ) ;
#29602 = EDGE_CURVE ( 'NONE', #45418, #28218, #37758, .T. ) ;
#29603 = VERTEX_POINT ( 'NONE', #8000 ) ;
#29604 = DIRECTION ( 'NONE',  ( -1.078386540356568435E-05, 7.293043936188563530E-06, -0.9999999999152598962 ) ) ;
#29605 = CARTESIAN_POINT ( 'NONE',  ( -10.19958527806322302, -12.98708191879287455, 67.85176988805619658 ) ) ;
#29606 = CARTESIAN_POINT ( 'NONE',  ( -24.69984158949002406, -13.20708760842489582, 59.55542051466775888 ) ) ;
#29607 = CARTESIAN_POINT ( 'NONE',  ( -20.53034385759798752, -6.857644439848019857, 49.98602051094138687 ) ) ;
#29608 = CARTESIAN_POINT ( 'NONE',  ( -21.39909385541298548, -8.105421454601382081, 49.25000573077630150 ) ) ;
#29609 = CARTESIAN_POINT ( 'NONE',  ( -14.67242798431547968, -21.73322265534233111, 58.27962637798393786 ) ) ;
#29610 = CARTESIAN_POINT ( 'NONE',  ( -23.85974590284097374, -11.05473623917629844, 73.54848671873985211 ) ) ;
#29611 = ORIENTED_EDGE ( 'NONE', *, *, #23870, .F. ) ;
#29612 = CIRCLE ( 'NONE', #9936, 3.951441697420975618 ) ;
#29613 = VERTEX_POINT ( 'NONE', #29906 ) ;
#29614 = CARTESIAN_POINT ( 'NONE',  ( -15.99909385541304196, -8.105421454601382081, 49.25000573077640098 ) ) ;
#29615 = EDGE_LOOP ( 'NONE', ( #42748, #31884 ) ) ;
#29616 = CARTESIAN_POINT ( 'NONE',  ( -17.11779890868097809, -21.80256347443895848, 72.39216574764959944 ) ) ;
#29617 = CARTESIAN_POINT ( 'NONE',  ( -12.14849447404118088, -10.12808629081546563, 67.91385578414299573 ) ) ;
#29618 = CARTESIAN_POINT ( 'NONE',  ( -24.60351398785051558, -12.81959416700296117, 66.50235511976165981 ) ) ;
#29619 = EDGE_CURVE ( 'NONE', #34569, #4804, #14863, .T. ) ;
#29620 = LINE ( 'NONE', #33528, #37971 ) ;
#29621 = ORIENTED_EDGE ( 'NONE', *, *, #31798, .T. ) ;
#29622 = DIRECTION ( 'NONE',  ( -3.549360974551879847E-17, 6.371834667872723308E-18, 1.000000000000000000 ) ) ;
#29623 = CARTESIAN_POINT ( 'NONE',  ( -17.42409385541305511, -14.80920654474410725, 81.99999999999998579 ) ) ;
#29624 = VERTEX_POINT ( 'NONE', #22022 ) ;
#29625 = DIRECTION ( 'NONE',  ( -0.5097212845717550289, 0.8603395911234820170, 0.000000000000000000 ) ) ;
#29626 = CARTESIAN_POINT ( 'NONE',  ( -15.02898246956647910, -5.450173255943768780, 54.50428052266513390 ) ) ;
#29627 = ORIENTED_EDGE ( 'NONE', *, *, #27266, .F. ) ;
#29628 = CARTESIAN_POINT ( 'NONE',  ( -17.84735443592641602, -7.371153788697909270, 60.19565345827741965 ) ) ;
#29629 = PLANE ( 'NONE',  #7898 ) ;
#29630 = EDGE_CURVE ( 'NONE', #30602, #12986, #29650, .T. ) ;
#29631 = CYLINDRICAL_SURFACE ( 'NONE', #36772, 2.000000000000001776 ) ;
#29632 = VERTEX_POINT ( 'NONE', #7002 ) ;
#29633 = LINE ( 'NONE', #14820, #12053 ) ;
#29634 = CARTESIAN_POINT ( 'NONE',  ( -15.87557863975121641, -7.931372594209569193, 67.14007279017359053 ) ) ;
#29635 = B_SPLINE_CURVE_WITH_KNOTS ( 'NONE', 3,
 ( #21260, #2543, #17544, #13834, #28876, #43921, #48555, #33509, #3495, #18507 ),
 .UNSPECIFIED., .F., .F.,
 ( 4, 2, 2, 2, 4 ),
 ( 0.000000000000000000, 0.2500000000000000000, 0.5000000000000000000, 0.7500000000000000000, 1.000000000000000000 ),
 .UNSPECIFIED. ) ;
#29636 = B_SPLINE_CURVE_WITH_KNOTS ( 'NONE', 3,
 ( #15503, #41636, #8159, #1001, #4446, #19719, #4217, #11110, #26132, #38163 ),
 .UNSPECIFIED., .F., .F.,
 ( 4, 2, 2, 2, 4 ),
 ( 0.000000000000000000, 0.2500000000000000000, 0.5000000000000000000, 0.7500000000000000000, 1.000000000000000000 ),
 .UNSPECIFIED. ) ;
#29637 = CARTESIAN_POINT ( 'NONE',  ( -11.90659230680199165, -10.41482083560927485, 74.53065494142421699 ) ) ;
#29638 = DIRECTION ( 'NONE',  ( -5.731567514496413899E-31, -1.020425574103664789E-16, -1.000000000000000000 ) ) ;
#29639 = VERTEX_POINT ( 'NONE', #3543 ) ;
#29640 = CARTESIAN_POINT ( 'NONE',  ( -10.67448150008226904, -11.65383075329928886, 74.74495363721690921 ) ) ;
#29641 = CARTESIAN_POINT ( 'NONE',  ( -12.73887154267113253, -15.16169402761810048, 49.52966884056655772 ) ) ;
#29642 = CARTESIAN_POINT ( 'NONE',  ( -14.05371385056185574, -21.00138210837564401, 72.07607703579976999 ) ) ;
#29643 = VECTOR ( 'NONE', #17495, 1000.000000000000000 ) ;
#29644 = CIRCLE ( 'NONE', #8421, 2.500000000000000444 ) ;
#29645 = DIRECTION ( 'NONE',  ( -1.000000000000000000, -2.866981220435666553E-17, -0.000000000000000000 ) ) ;
#29646 = FACE_OUTER_BOUND ( 'NONE', #15304, .T. ) ;
#29647 = ORIENTED_EDGE ( 'NONE', *, *, #19074, .F. ) ;
#29648 = CARTESIAN_POINT ( 'NONE',  ( -24.31477923169101629, -16.30090137217950996, 59.40860294853779777 ) ) ;
#29649 = VERTEX_POINT ( 'NONE', #25710 ) ;
#29650 = LINE ( 'NONE', #44442, #32385 ) ;
#29651 = AXIS2_PLACEMENT_3D ( 'NONE', #30863, #12365, #12845 ) ;
#29652 = CARTESIAN_POINT ( 'NONE',  ( -21.65914559189701194, -18.31838547852702703, 53.49899999999994549 ) ) ;
#29653 = CARTESIAN_POINT ( 'NONE',  ( -24.34138250757121469, -16.17068267630804357, 62.89328676667766871 ) ) ;
#29654 = ORIENTED_EDGE ( 'NONE', *, *, #7330, .T. ) ;
#29655 = CARTESIAN_POINT ( 'NONE',  ( -10.05508844999486939, -15.90482974550872974, 64.70760360623624763 ) ) ;
#29656 = CYLINDRICAL_SURFACE ( 'NONE', #18853, 0.1500000000000020484 ) ;
#29657 = ADVANCED_FACE ( 'NONE', ( #44686 ), #45413, .T. ) ;
#29658 = EDGE_CURVE ( 'NONE', #17650, #45493, #38963, .T. ) ;
#29659 = EDGE_LOOP ( 'NONE', ( #5313, #24153, #38174 ) ) ;
#29660 = ORIENTED_EDGE ( 'NONE', *, *, #2796, .F. ) ;
#29661 = CARTESIAN_POINT ( 'NONE',  ( -16.39284385650552167, -7.406986770994973490, 48.81910596585309747 ) ) ;
#29662 = DIRECTION ( 'NONE',  ( 0.7029450532227031756, 0.7112441579020041260, -7.405715380709556396E-09 ) ) ;
#29663 = CARTESIAN_POINT ( 'NONE',  ( -13.76436681951595098, -7.422085961289871747, 53.49999999999995026 ) ) ;
#29664 = LINE ( 'NONE', #41229, #42478 ) ;
#29665 = DIRECTION ( 'NONE',  ( 0.000000000000000000, 0.000000000000000000, -1.000000000000000000 ) ) ;
#29666 = ORIENTED_EDGE ( 'NONE', *, *, #4670, .F. ) ;
#29667 = EDGE_LOOP ( 'NONE', ( #22132, #22894, #3703, #35617, #26136 ) ) ;
#29668 = EDGE_CURVE ( 'NONE', #25804, #45155, #29995, .T. ) ;
#29669 = EDGE_CURVE ( 'NONE', #34964, #4399, #46136, .T. ) ;
#29670 = CARTESIAN_POINT ( 'NONE',  ( -16.48034385650551670, -6.424090610841176385, 49.80797279389977916 ) ) ;
#29671 = CARTESIAN_POINT ( 'NONE',  ( -17.42409385541299471, -14.80920654474434883, 62.02966884056656482 ) ) ;
#29672 = DIRECTION ( 'NONE',  ( 1.000000000000000000, -4.164305804376849788E-17, 1.614929280266638808E-16 ) ) ;
#29673 = CARTESIAN_POINT ( 'NONE',  ( -14.00534385650551883, -8.801233750844183135, 48.81488406609782515 ) ) ;
#29674 = B_SPLINE_CURVE_WITH_KNOTS ( 'NONE', 3,
 ( #3877, #41788, #11744, #30470, #45487, #29722, #41287, #34371, #37329, #7571 ),
 .UNSPECIFIED., .F., .F.,
 ( 4, 2, 2, 2, 4 ),
 ( 0.000000000000000000, 0.2500000000000000000, 0.5000000000000000000, 0.7500000000000000000, 1.000000000000000000 ),
 .UNSPECIFIED. ) ;
#29675 = B_SPLINE_CURVE_WITH_KNOTS ( 'NONE', 3,
 ( #45910, #8242, #27425, #1081, #8731, #43922, #20769, #21262, #28156, #20538 ),
 .UNSPECIFIED., .F., .F.,
 ( 4, 2, 2, 2, 4 ),
 ( 0.1272669073657700656, 0.2522669073462741052, 0.3772669073267782003, 0.5022669073072822954, 0.6272669072877863350 ),
 .UNSPECIFIED. ) ;
#29676 = AXIS2_PLACEMENT_3D ( 'NONE', #42842, #35433, #4937 ) ;
#29677 = ORIENTED_EDGE ( 'NONE', *, *, #47039, .T. ) ;
#29678 = EDGE_CURVE ( 'NONE', #24038, #21562, #26445, .T. ) ;
#29679 = CARTESIAN_POINT ( 'NONE',  ( -18.22551936265966432, -9.873852742195451171, 53.27966884056655061 ) ) ;
#29680 = CIRCLE ( 'NONE', #2158, 1.000000000000000888 ) ;
#29681 = CARTESIAN_POINT ( 'NONE',  ( -11.21783104652298846, -18.93062367394879431, 64.93202350587574756 ) ) ;
#29682 = ORIENTED_EDGE ( 'NONE', *, *, #3154, .F. ) ;
#29683 = DIRECTION ( 'NONE',  ( -0.9687793358424819923, 0.2479245821708680464, 0.000000000000000000 ) ) ;
#29684 = VERTEX_POINT ( 'NONE', #22264 ) ;
#29685 = CARTESIAN_POINT ( 'NONE',  ( -22.66103498339474953, -20.10797505100955718, 69.32417989821951210 ) ) ;
#29686 = CARTESIAN_POINT ( 'NONE',  ( -19.45790305330666925, -21.50891704259349169, 65.65413287592375013 ) ) ;
#29687 = CARTESIAN_POINT ( 'NONE',  ( -11.03557423443333008, -17.80950410671109196, 68.25289248663547426 ) ) ;
#29688 = CARTESIAN_POINT ( 'NONE',  ( -20.84119928492007645, -20.97572016636869918, 62.41471400470057773 ) ) ;
#29689 = ORIENTED_EDGE ( 'NONE', *, *, #681, .T. ) ;
#29690 = CARTESIAN_POINT ( 'NONE',  ( -11.09534973027204074, -10.87830236297815745, 57.36936532087455021 ) ) ;
#29691 = CARTESIAN_POINT ( 'NONE',  ( -4.424093855413049781, -6.359206544744109735, 52.99999999999998579 ) ) ;
#29692 = LINE ( 'NONE', #37803, #25051 ) ;
#29693 = CARTESIAN_POINT ( 'NONE',  ( -22.63560516303400050, -20.13310814558360917, 69.28922553891734992 ) ) ;
#29694 = EDGE_LOOP ( 'NONE', ( #34796, #28321, #38820 ) ) ;
#29695 = CARTESIAN_POINT ( 'NONE',  ( -22.68321696279682342, -10.11402890775583074, 70.01178527271520124 ) ) ;
#29696 = FACE_OUTER_BOUND ( 'NONE', #34304, .T. ) ;
#29697 = DIRECTION ( 'NONE',  ( 0.000000000000000000, -0.9999954153791273948, -0.003028072113819838245 ) ) ;
#29698 = VERTEX_POINT ( 'NONE', #48121 ) ;
#29699 = DIRECTION ( 'NONE',  ( 0.000000000000000000, 0.000000000000000000, 1.000000000000000000 ) ) ;
#29700 = ORIENTED_EDGE ( 'NONE', *, *, #30628, .F. ) ;
#29701 = CARTESIAN_POINT ( 'NONE',  ( -21.37101582717423298, -20.65516655669274826, 69.26269923806351869 ) ) ;
#29702 = CARTESIAN_POINT ( 'NONE',  ( -24.38756562526642213, -15.91227465074931935, 66.34852784166324113 ) ) ;
#29703 = CARTESIAN_POINT ( 'NONE',  ( -18.72680718162379065, -7.880610904852765053, 70.67068030199192208 ) ) ;
#29704 = VECTOR ( 'NONE', #34530, 1000.000000000000114 ) ;
#29705 = LINE ( 'NONE', #29462, #33699 ) ;
#29706 = EDGE_LOOP ( 'NONE', ( #16971, #13907, #4363, #42852, #3243 ) ) ;
#29707 = CARTESIAN_POINT ( 'NONE',  ( -14.27672825910291365, -8.496605361553417168, 74.49954621647665931 ) ) ;
#29708 = VERTEX_POINT ( 'NONE', #33074 ) ;
#29709 =( BOUNDED_SURFACE ( )  B_SPLINE_SURFACE ( 3, 1, ( 
 ( #39893, #11808 ),
 ( #723, #45795 ),
 ( #27454, #11318 ),
 ( #38364, #34686 ),
 ( #4657, #15227 ),
 ( #34191, #33956 ),
 ( #22642, #7882 ) ),
 .UNSPECIFIED., .T., .F., .F. ) 
 B_SPLINE_SURFACE_WITH_KNOTS ( ( 4, 3, 4 ),
 ( 2, 2 ),
 ( 0.000000000000000000, 0.5000000000000000000, 1.000000000000000000 ),
 ( 0.000000000000000000, 1.000000000000000000 ),
 .UNSPECIFIED. ) 
 GEOMETRIC_REPRESENTATION_ITEM ( )  RATIONAL_B_SPLINE_SURFACE ( (
 ( 1.000000000000000000, 1.000000000000000000),
 ( 0.3333333333333335369, 0.3333333333333330373),
 ( 0.3333333333333335369, 0.3333333333333330373),
 ( 1.000000000000000000, 1.000000000000000000),
 ( 0.3333333333333333703, 0.3333333333333333703),
 ( 0.3333333333333333703, 0.3333333333333333703),
 ( 1.000000000000000000, 1.000000000000000000) ) ) 
 REPRESENTATION_ITEM ( '' )  SURFACE ( )  );
#29710 = CARTESIAN_POINT ( 'NONE',  ( -12.68532267716109985, -9.060482739934947460, 71.03420753023118550 ) ) ;
#29711 = CARTESIAN_POINT ( 'NONE',  ( -20.72450927900464634, -21.03929139025762751, 58.93003081252663833 ) ) ;
#29712 = ORIENTED_EDGE ( 'NONE', *, *, #26217, .T. ) ;
#29713 = AXIS2_PLACEMENT_3D ( 'NONE', #42090, #254, #38133 ) ;
#29714 = AXIS2_PLACEMENT_3D ( 'NONE', #15014, #45592, #12081 ) ;
#29715 = DIRECTION ( 'NONE',  ( 0.9979768094191903138, 0.06357898915123796901, 0.000000000000000000 ) ) ;
#29716 = EDGE_CURVE ( 'NONE', #43417, #9318, #37505, .T. ) ;
#29717 = ORIENTED_EDGE ( 'NONE', *, *, #23477, .T. ) ;
#29718 = ORIENTED_EDGE ( 'NONE', *, *, #22919, .T. ) ;
#29719 = CARTESIAN_POINT ( 'NONE',  ( -15.65720112442257950, -8.035743057838505621, 70.90989791475803372 ) ) ;
#29720 = CYLINDRICAL_SURFACE ( 'NONE', #13132, 0.1500000000000056566 ) ;
#29721 = AXIS2_PLACEMENT_3D ( 'NONE', #21828, #44743, #3107 ) ;
#29722 = CARTESIAN_POINT ( 'NONE',  ( -21.27974070113173255, -20.65163647771647604, 69.24553270363776392 ) ) ;
#29723 = DIRECTION ( 'NONE',  ( -0.8651630202045381690, 0.5014907262059381532, 5.433021001366390361E-08 ) ) ;
#29724 =( BOUNDED_CURVE ( )  B_SPLINE_CURVE ( 3, ( #15712, #15222, #15462, #34921 ),
 .UNSPECIFIED., .F., .F. ) 
 B_SPLINE_CURVE_WITH_KNOTS ( ( 4, 4 ),
 ( 0.5000000000000000000, 0.9074455897393653991 ),
 .UNSPECIFIED. ) 
 CURVE ( )  GEOMETRIC_REPRESENTATION_ITEM ( )  RATIONAL_B_SPLINE_CURVE ( ( 1.000000000000008660, 0.4567392136813321346, 0.3561768502900242162, 0.6983129098260942857 ) ) 
 REPRESENTATION_ITEM ( '' )  );
#29725 = CARTESIAN_POINT ( 'NONE',  ( -13.22529448846758982, -9.145569705956512863, 64.19474388871357462 ) ) ;
#29726 = FACE_OUTER_BOUND ( 'NONE', #16559, .T. ) ;
#29727 = CARTESIAN_POINT ( 'NONE',  ( -20.32907747881911575, -11.13165948213017131, 49.52966884056655772 ) ) ;
#29728 = CIRCLE ( 'NONE', #41493, 2.000000000000001776 ) ;
#29729 = ORIENTED_EDGE ( 'NONE', *, *, #3036, .T. ) ;
#29730 = ORIENTED_EDGE ( 'NONE', *, *, #34909, .F. ) ;
#29731 = EDGE_CURVE ( 'NONE', #45314, #33165, #17199, .T. ) ;
#29732 = ADVANCED_FACE ( 'NONE', ( #33820 ), #15339, .T. ) ;
#29733 = CARTESIAN_POINT ( 'NONE',  ( -12.13084389729548640, -10.22855792347674786, 64.04416791493218852 ) ) ;
#29734 = ADVANCED_FACE ( 'NONE', ( #29410 ), #38736, .T. ) ;
#29735 = CARTESIAN_POINT ( 'NONE',  ( -21.36489355414517632, -8.963473290115421932, 73.90128753234840531 ) ) ;
#29736 = CARTESIAN_POINT ( 'NONE',  ( -12.75531685953890282, -14.40201664703461049, 49.52966884056655772 ) ) ;
#29737 = CARTESIAN_POINT ( 'NONE',  ( -10.97013630564127773, -17.52378418614773281, 71.67791182052884835 ) ) ;
#29738 = CARTESIAN_POINT ( 'NONE',  ( -15.15660932275500272, -21.48492473237050859, 65.39124617759186719 ) ) ;
#29739 = ADVANCED_FACE ( 'NONE', ( #12636 ), #23490, .T. ) ;
#29740 = VERTEX_POINT ( 'NONE', #12872 ) ;
#29741 = CARTESIAN_POINT ( 'NONE',  ( -20.38659385650551670, -9.302874398569244363, 51.68646062012417985 ) ) ;
#29742 =( BOUNDED_CURVE ( )  B_SPLINE_CURVE ( 3, ( #14094, #47623, #43697, #13854 ),
 .UNSPECIFIED., .F., .F. ) 
 B_SPLINE_CURVE_WITH_KNOTS ( ( 4, 4 ),
 ( 0.000000000000000000, 0.4074455897393665649 ),
 .UNSPECIFIED. ) 
 CURVE ( )  GEOMETRIC_REPRESENTATION_ITEM ( )  RATIONAL_B_SPLINE_CURVE ( ( 1.000000000000000000, 0.4567392136813314685, 0.3561768502900301003, 0.6983129098260959511 ) ) 
 REPRESENTATION_ITEM ( '' )  );
#29743 = ORIENTED_EDGE ( 'NONE', *, *, #43174, .T. ) ;
#29744 = CARTESIAN_POINT ( 'NONE',  ( -17.42409385541299471, -14.80920654474435594, 52.02966884056656482 ) ) ;
#29745 = ADVANCED_FACE ( 'NONE', ( #5020 ), #5253, .T. ) ;
#29746 = CARTESIAN_POINT ( 'NONE',  ( -16.75933984047804515, -20.01695097968237036, 50.77966884056656482 ) ) ;
#29747 = AXIS2_PLACEMENT_3D ( 'NONE', #29641, #3532, #47872 ) ;
#29748 = CARTESIAN_POINT ( 'NONE',  ( -17.42409385541300182, -14.80920654474440745, 53.27966884056655061 ) ) ;
#29749 = VERTEX_POINT ( 'NONE', #23976 ) ;
#29750 = CARTESIAN_POINT ( 'NONE',  ( -22.50276953350645925, -9.919252841961412770, 73.77601325438966740 ) ) ;
#29751 = VECTOR ( 'NONE', #27649, 1000.000000000000000 ) ;
#29752 = CIRCLE ( 'NONE', #22690, 1.999999999999999334 ) ;
#29753 = FACE_OUTER_BOUND ( 'NONE', #40506, .T. ) ;
#29754 = CARTESIAN_POINT ( 'NONE',  ( -27.41460927708051898, -13.34199974102237896, 54.54971261817296835 ) ) ;
#29755 = EDGE_LOOP ( 'NONE', ( #15184, #40021, #36951, #551, #11101 ) ) ;
#29756 = CONICAL_SURFACE ( 'NONE', #3783, 0.5560000000000009379, 0.06981317007976595157 ) ;
#29757 = CYLINDRICAL_SURFACE ( 'NONE', #39125, 0.1500000000000022427 ) ;
#29758 = CARTESIAN_POINT ( 'NONE',  ( -42.29394679658953038, -14.80920654474417830, 64.04117647058822627 ) ) ;
#29759 = VERTEX_POINT ( 'NONE', #16069 ) ;
#29760 = CARTESIAN_POINT ( 'NONE',  ( -24.67963342063540466, -16.50099095021179352, 59.28478976814308510 ) ) ;
#29761 = VERTEX_POINT ( 'NONE', #1552 ) ;
#29762 = CARTESIAN_POINT ( 'NONE',  ( -20.59270190486383356, -18.27842527154038166, 52.02966884056656482 ) ) ;
#29763 = CARTESIAN_POINT ( 'NONE',  ( -17.59145722722324479, -7.361077857161463456, 63.75045814445680037 ) ) ;
#29764 = ORIENTED_EDGE ( 'NONE', *, *, #12760, .T. ) ;
#29765 = DIRECTION ( 'NONE',  ( 0.000000000000000000, 0.000000000000000000, 1.000000000000000000 ) ) ;
#29766 = CARTESIAN_POINT ( 'NONE',  ( -16.52316554273587101, -21.80170452179945073, 65.24036514508233608 ) ) ;
#29767 = ORIENTED_EDGE ( 'NONE', *, *, #18443, .T. ) ;
#29768 = CARTESIAN_POINT ( 'NONE',  ( -21.44204676556661582, -20.54122665395610525, 72.71549499130021843 ) ) ;
#29769 = ADVANCED_FACE ( 'NONE', ( #34800 ), #42447, .T. ) ;
#29770 = CARTESIAN_POINT ( 'NONE',  ( -11.10470791607724550, -18.75498134223953883, 61.46206221440264983 ) ) ;
#29771 = CARTESIAN_POINT ( 'NONE',  ( -24.72409385541305582, -14.90920654474420104, 66.05294117647058272 ) ) ;
#29772 = B_SPLINE_CURVE_WITH_KNOTS ( 'NONE', 3,
 ( #36690, #29340, #33246, #48286, #14517, #29580, #7192, #18482, #33487, #14766 ),
 .UNSPECIFIED., .F., .F.,
 ( 4, 2, 2, 2, 4 ),
 ( 0.1272669073658055372, 0.2522669073462952549, 0.3772669073267849171, 0.5022669073072746349, 0.6272669072877643526 ),
 .UNSPECIFIED. ) ;
#29773 = B_SPLINE_CURVE_WITH_KNOTS ( 'NONE', 1,
 ( #20862, #42792 ),
 .UNSPECIFIED., .F., .F.,
 ( 2, 2 ),
 ( 0.000000000000000000, 1.000000000000000000 ),
 .UNSPECIFIED. ) ;
#29774 = VERTEX_POINT ( 'NONE', #8716 ) ;
#29775 = CARTESIAN_POINT ( 'NONE',  ( -13.36507556264098717, -20.57353123648257665, 58.04650106771609330 ) ) ;
#29776 = CARTESIAN_POINT ( 'NONE',  ( -14.92957361138602579, -21.82925975653312278, 65.22101252026929785 ) ) ;
#29777 = DIRECTION ( 'NONE',  ( -5.551115123125782702E-17, -1.232595164407830946E-32, -1.000000000000000000 ) ) ;
#29778 = EDGE_CURVE ( 'NONE', #27147, #6936, #17492, .T. ) ;
#29779 = ORIENTED_EDGE ( 'NONE', *, *, #13351, .T. ) ;
#29780 = ORIENTED_EDGE ( 'NONE', *, *, #32346, .F. ) ;
#29781 = DIRECTION ( 'NONE',  ( 0.9926276493613465091, 0.06323820549166281335, 0.1033986416233891870 ) ) ;
#29782 = CARTESIAN_POINT ( 'NONE',  ( -16.96571475693685116, -7.824107681210383802, 74.26018256191720468 ) ) ;
#29784 = FACE_OUTER_BOUND ( 'NONE', #45665, .T. ) ;
#29783 = VECTOR ( 'NONE', #20743, 1000.000000000000227 ) ;
#29785 = CARTESIAN_POINT ( 'NONE',  ( -16.19909385759799036, -8.105421454601382081, 49.25000573077640098 ) ) ;
#29786 = CARTESIAN_POINT ( 'NONE',  ( -23.30132152709437676, -10.22970227413176580, 63.25841351925517841 ) ) ;
#29787 = CARTESIAN_POINT ( 'NONE',  ( -13.17078218117215549, -9.186392337449538203, 67.39414915108072535 ) ) ;
#29788 = CARTESIAN_POINT ( 'NONE',  ( -23.98503169607928953, -17.39005800936845603, 66.22885190747201989 ) ) ;
#29789 = CIRCLE ( 'NONE', #38412, 2.000000000000008882 ) ;
#29790 = AXIS2_PLACEMENT_3D ( 'NONE', #42683, #20021, #12629 ) ;
#29791 = CARTESIAN_POINT ( 'NONE',  ( -14.62687819956926027, -8.392386103536567887, 64.08978840643771946 ) ) ;
#29792 = ORIENTED_EDGE ( 'NONE', *, *, #38290, .F. ) ;
#29793 = CARTESIAN_POINT ( 'NONE',  ( -24.12071557656922494, -11.54438865435207795, 63.06722852297808402 ) ) ;
#29794 = EDGE_CURVE ( 'NONE', #39884, #38652, #27658, .T. ) ;
#29795 = VECTOR ( 'NONE', #1339, 1000.000000000000114 ) ;
#29796 = CARTESIAN_POINT ( 'NONE',  ( -14.24626305875727184, -11.36469298288595553, 52.02966884056656482 ) ) ;
#29797 = DIRECTION ( 'NONE',  ( -0.9687793358424822143, 0.2479245821708672415, 0.000000000000000000 ) ) ;
#29798 = EDGE_CURVE ( 'NONE', #37103, #9885, #31112, .T. ) ;
#29799 = EDGE_LOOP ( 'NONE', ( #10851, #16520, #12465, #6381, #22877 ) ) ;
#29800 = EDGE_CURVE ( 'NONE', #25288, #22645, #46130, .T. ) ;
#29801 = ORIENTED_EDGE ( 'NONE', *, *, #37779, .F. ) ;
#29802 = DIRECTION ( 'NONE',  ( -3.071710424422018668E-17, 6.404604876783312462E-16, 1.000000000000000000 ) ) ;
#29803 = DIRECTION ( 'NONE',  ( 0.000000000000000000, 0.000000000000000000, 1.000000000000000000 ) ) ;
#29804 = CARTESIAN_POINT ( 'NONE',  ( -11.72771377538897042, -10.00769167454747688, 67.60622713944691498 ) ) ;
#29805 = CARTESIAN_POINT ( 'NONE',  ( -10.18203091723714770, -13.06113264623505721, 71.40166907525704687 ) ) ;
#29806 = EDGE_CURVE ( 'NONE', #28884, #4347, #38665, .T. ) ;
#29807 = EDGE_LOOP ( 'NONE', ( #10920, #16282, #15985, #7678 ) ) ;
#29808 = CARTESIAN_POINT ( 'NONE',  ( -24.50475423537784536, -17.33693471837318612, 54.02312124697527906 ) ) ;
#29809 = DIRECTION ( 'NONE',  ( 0.3163880819683246304, 0.8528035521334702551, 0.4154812667942326954 ) ) ;
#29810 = VERTEX_POINT ( 'NONE', #23743 ) ;
#29811 = CARTESIAN_POINT ( 'NONE',  ( -22.33161753753789469, -20.41455022152800325, 62.49085083065315160 ) ) ;
#29812 = VECTOR ( 'NONE', #41276, 1000.000000000000000 ) ;
#29813 =( BOUNDED_SURFACE ( )  B_SPLINE_SURFACE ( 3, 1, ( 
 ( #25031, #36094 ),
 ( #2618, #24564 ),
 ( #24315, #25277 ),
 ( #28489, #28245 ),
 ( #43014, #40051 ),
 ( #40293, #47676 ),
 ( #28958, #20850 ) ),
 .UNSPECIFIED., .T., .F., .F. ) 
 B_SPLINE_SURFACE_WITH_KNOTS ( ( 4, 3, 4 ),
 ( 2, 2 ),
 ( 0.000000000000000000, 0.5000000000000000000, 1.000000000000000000 ),
 ( 0.000000000000000000, 1.000000000000000000 ),
 .UNSPECIFIED. ) 
 GEOMETRIC_REPRESENTATION_ITEM ( )  RATIONAL_B_SPLINE_SURFACE ( (
 ( 1.000000000000000000, 1.000000000000000000),
 ( 0.3333333333333335369, 0.3333333333333330373),
 ( 0.3333333333333335369, 0.3333333333333330373),
 ( 1.000000000000000000, 1.000000000000000000),
 ( 0.3333333333333333703, 0.3333333333333333703),
 ( 0.3333333333333333703, 0.3333333333333333703),
 ( 1.000000000000000000, 1.000000000000000000) ) ) 
 REPRESENTATION_ITEM ( '' )  SURFACE ( )  );
#29814 = DIRECTION ( 'NONE',  ( 0.9687793358424823253, -0.2479245821708663811, 0.000000000000000000 ) ) ;
#29815 =( GEOMETRIC_REPRESENTATION_CONTEXT ( 3 ) GLOBAL_UNCERTAINTY_ASSIGNED_CONTEXT ( ( #44025 ) ) GLOBAL_UNIT_ASSIGNED_CONTEXT ( ( #31009, #26835, #46029 ) ) REPRESENTATION_CONTEXT ( 'NONE', 'WORKASPACE' ) );
#29816 = CARTESIAN_POINT ( 'NONE',  ( -10.85423598487861874, -17.22645666615770921, 64.91122787125294735 ) ) ;
#29817 = ORIENTED_EDGE ( 'NONE', *, *, #37788, .F. ) ;
#29818 = AXIS2_PLACEMENT_3D ( 'NONE', #21504, #36486, #2288 ) ;
#29819 = AXIS2_PLACEMENT_3D ( 'NONE', #11248, #28798, #36169 ) ;
#29820 = VERTEX_POINT ( 'NONE', #15836 ) ;
#29821 = CARTESIAN_POINT ( 'NONE',  ( -19.49109506855409180, -21.54969648977046148, 62.28031529404344013 ) ) ;
#29822 = CARTESIAN_POINT ( 'NONE',  ( -24.39570712928462370, -14.17877393659436080, 69.66777723616006313 ) ) ;
#29823 = ORIENTED_EDGE ( 'NONE', *, *, #18187, .F. ) ;
#29824 = DIRECTION ( 'NONE',  ( -0.3964226963016467820, -0.9180681052388935948, 0.000000000000000000 ) ) ;
#29825 = CYLINDRICAL_SURFACE ( 'NONE', #36741, 0.1499999999999973577 ) ;
#29826 = CARTESIAN_POINT ( 'NONE',  ( -22.66784385650551670, -6.428312510596451368, 51.20221977374900035 ) ) ;
#29827 = CARTESIAN_POINT ( 'NONE',  ( -16.16748626245079379, -22.20318634978239203, 53.49999999999994316 ) ) ;
#29828 = CIRCLE ( 'NONE', #16416, 2.000000000000001332 ) ;
#29829 = EDGE_CURVE ( 'NONE', #45965, #16929, #44551, .T. ) ;
#29830 = DIRECTION ( 'NONE',  ( 0.000000000000000000, 1.000000000000000000, -0.000000000000000000 ) ) ;
#29831 = CARTESIAN_POINT ( 'NONE',  ( -15.46621039653938112, -10.55127575485719760, 49.52966884056655772 ) ) ;
#29832 = CYLINDRICAL_SURFACE ( 'NONE', #13232, 0.1500000000000061007 ) ;
#29833 = ORIENTED_EDGE ( 'NONE', *, *, #16982, .F. ) ;
#29834 = CARTESIAN_POINT ( 'NONE',  ( -16.91855014848012928, -22.24212009645463439, 72.28047803099305213 ) ) ;
#29835 = CARTESIAN_POINT ( 'NONE',  ( -21.99649211598757859, -13.72812852161587038, 49.52966884056655772 ) ) ;
#29836 = CARTESIAN_POINT ( 'NONE',  ( -22.75923595801102550, -10.27751167601812909, 66.54182257657851096 ) ) ;
#29837 = DIRECTION ( 'NONE',  ( 1.000000000000000000, -4.164305804376849788E-17, 1.614929280266638808E-16 ) ) ;
#29838 = CARTESIAN_POINT ( 'NONE',  ( -10.78527719640413451, -12.58937423537859424, 60.79853578751971099 ) ) ;
#29839 = CARTESIAN_POINT ( 'NONE',  ( -23.80628931054383202, -18.65249568317075202, 72.95642365399113771 ) ) ;
#29840 = ORIENTED_EDGE ( 'NONE', *, *, #43642, .T. ) ;
#29841 = ORIENTED_EDGE ( 'NONE', *, *, #21333, .F. ) ;
#29842 = CARTESIAN_POINT ( 'NONE',  ( -4.424093855413053333, -25.10920654474410441, 63.99999999999998579 ) ) ;
#29843 = CARTESIAN_POINT ( 'NONE',  ( -14.95042968149815188, -8.260718009457519884, 56.84999999999994458 ) ) ;
#29844 = ORIENTED_EDGE ( 'NONE', *, *, #22726, .F. ) ;
#29846 = LINE ( 'NONE', #26384, #9203 ) ;
#29845 = CARTESIAN_POINT ( 'NONE',  ( -23.68653687815194786, -11.57061008776567945, 66.43686604568146947 ) ) ;
#29847 = CARTESIAN_POINT ( 'NONE',  ( -24.21255584207132827, -13.09477218448524027, 66.41319906622749158 ) ) ;
#29848 = CARTESIAN_POINT ( 'NONE',  ( -20.70278685264619867, -8.119407593049823291, 63.41783206474445223 ) ) ;
#29849 = DIRECTION ( 'NONE',  ( -5.731567514496413899E-31, -1.020425574103664789E-16, -1.000000000000000000 ) ) ;
#29850 = CARTESIAN_POINT ( 'NONE',  ( -24.27661814142333796, -16.49973396376381984, 62.73761853866894711 ) ) ;
#29851 = CARTESIAN_POINT ( 'NONE',  ( -11.45752044641470668, -19.27057170535650954, 71.87181270239314301 ) ) ;
#29852 = DIRECTION ( 'NONE',  ( -1.000000000000000000, -2.866981220435666553E-17, -0.000000000000000000 ) ) ;
#29853 = B_SPLINE_CURVE_WITH_KNOTS ( 'NONE', 3,
 ( #20347, #20595, #31910, #24289, #35356, #35104, #1869, #16392, #8794, #46927 ),
 .UNSPECIFIED., .F., .F.,
 ( 4, 2, 2, 2, 4 ),
 ( 0.000000000000000000, 0.2500000000000000000, 0.5000000000000000000, 0.7500000000000000000, 1.000000000000000000 ),
 .UNSPECIFIED. ) ;
#29854 = DIRECTION ( 'NONE',  ( 4.115385489419834196E-17, 0.9999954153791273948, 0.003028072113822188795 ) ) ;
#29855 = ORIENTED_EDGE ( 'NONE', *, *, #30870, .F. ) ;
#29856 = CARTESIAN_POINT ( 'NONE',  ( -21.68499601416157674, -9.192516039336663169, 66.66149992327366647 ) ) ;
#29857 = EDGE_CURVE ( 'NONE', #47871, #39323, #4294, .T. ) ;
#29858 = CIRCLE ( 'NONE', #37711, 4.686499999999997890 ) ;
#29859 = CARTESIAN_POINT ( 'NONE',  ( -12.11599782822167271, -20.03693337884723391, 61.55712024599606025 ) ) ;
#29860 = DIRECTION ( 'NONE',  ( 0.9687793358424821033, -0.2479245821708680464, 0.000000000000000000 ) ) ;
#29861 = CARTESIAN_POINT ( 'NONE',  ( -24.23813412381375088, -12.99935709875259704, 66.31718868320673721 ) ) ;
#29862 = CARTESIAN_POINT ( 'NONE',  ( -20.75918756122348441, -8.147305293919229641, 63.42626095967343502 ) ) ;
#29863 = ORIENTED_EDGE ( 'NONE', *, *, #37081, .T. ) ;
#29864 = ORIENTED_EDGE ( 'NONE', *, *, #13237, .F. ) ;
#29865 = CARTESIAN_POINT ( 'NONE',  ( -14.36784385541304232, -9.357632978295830739, 49.97845033065684106 ) ) ;
#29866 = EDGE_CURVE ( 'NONE', #28685, #5757, #24298, .T. ) ;
#29867 = ORIENTED_EDGE ( 'NONE', *, *, #466, .F. ) ;
#29868 = CARTESIAN_POINT ( 'NONE',  ( -17.11743416019711361, -21.80254600073977045, 72.23831284135304998 ) ) ;
#29869 = LINE ( 'NONE', #45375, #905 ) ;
#29870 = CIRCLE ( 'NONE', #28287, 2.499999999999999112 ) ;
#29871 = ADVANCED_FACE ( 'NONE', ( #46627 ), #34300, .T. ) ;
#29872 =( BOUNDED_SURFACE ( )  B_SPLINE_SURFACE ( 3, 1, ( 
 ( #9884, #36925 ),
 ( #17727, #40394 ),
 ( #6183, #18216 ),
 ( #33221, #48260 ),
 ( #14497, #44584 ),
 ( #39914, #36208 ),
 ( #11092, #45321 ) ),
 .UNSPECIFIED., .T., .F., .F. ) 
 B_SPLINE_SURFACE_WITH_KNOTS ( ( 4, 3, 4 ),
 ( 2, 2 ),
 ( 0.000000000000000000, 0.5000000000000000000, 1.000000000000000000 ),
 ( 0.000000000000000000, 1.000000000000000000 ),
 .UNSPECIFIED. ) 
 GEOMETRIC_REPRESENTATION_ITEM ( )  RATIONAL_B_SPLINE_SURFACE ( (
 ( 1.000000000000000000, 1.000000000000000000),
 ( 0.3333333333333335369, 0.3333333333333330373),
 ( 0.3333333333333335369, 0.3333333333333330373),
 ( 1.000000000000000000, 1.000000000000000000),
 ( 0.3333333333333333703, 0.3333333333333333703),
 ( 0.3333333333333333703, 0.3333333333333333703),
 ( 1.000000000000000000, 1.000000000000000000) ) ) 
 REPRESENTATION_ITEM ( '' )  SURFACE ( )  );
#29873 = LINE ( 'NONE', #3277, #13497 ) ;
#29874 = CARTESIAN_POINT ( 'NONE',  ( -21.98892968875003717, -15.92178434430670642, 49.52966884056655772 ) ) ;
#29875 = EDGE_LOOP ( 'NONE', ( #11987, #9837, #32052, #43821, #21319 ) ) ;
#29876 = CARTESIAN_POINT ( 'NONE',  ( -23.07906183844443859, -9.958936969296642516, 66.72677665813928627 ) ) ;
#29877 = CARTESIAN_POINT ( 'NONE',  ( 18.57590614458706924, 2.136931092028983681, 51.79103196254472863 ) ) ;
#29878 = EDGE_LOOP ( 'NONE', ( #33420, #26312, #28401, #14362, #21487 ) ) ;
#29879 = CARTESIAN_POINT ( 'NONE',  ( -17.19811928533322387, -9.313850733363548073, 53.49999999999995026 ) ) ;
#29880 = ADVANCED_FACE ( 'NONE', ( #8233 ), #36047, .T. ) ;
#29881 =( BOUNDED_CURVE ( )  B_SPLINE_CURVE ( 3, ( #23687, #16979, #23432, #19740 ),
 .UNSPECIFIED., .F., .F. ) 
 B_SPLINE_CURVE_WITH_KNOTS ( ( 4, 4 ),
 ( 0.4074455897393668979, 0.5000000000000000000 ),
 .UNSPECIFIED. ) 
 CURVE ( )  GEOMETRIC_REPRESENTATION_ITEM ( )  RATIONAL_B_SPLINE_CURVE ( ( 0.6983129098261043888, 0.7760317562607172981, 0.8765941196520187217, 1.000000000000014877 ) ) 
 REPRESENTATION_ITEM ( '' )  );
#29882 = EDGE_CURVE ( 'NONE', #17452, #19689, #35999, .T. ) ;
#29883 = VERTEX_POINT ( 'NONE', #13820 ) ;
#29884 = CARTESIAN_POINT ( 'NONE',  ( -17.95184243766222565, -21.84304804239566522, 58.61373395300507383 ) ) ;
#29885 = CARTESIAN_POINT ( 'NONE',  ( -11.10300301615976259, -11.79817525417081292, 74.66913066534023358 ) ) ;
#29886 = CARTESIAN_POINT ( 'NONE',  ( -14.42683414290149635, -8.428067600363895906, 67.25975083869262505 ) ) ;
#29887 = EDGE_CURVE ( 'NONE', #30487, #39013, #181, .T. ) ;
#29888 = VERTEX_POINT ( 'NONE', #32332 ) ;
#29889 = FACE_OUTER_BOUND ( 'NONE', #22825, .T. ) ;
#29890 = CARTESIAN_POINT ( 'NONE',  ( -11.77326604373719476, -19.03093417793677133, 68.21689334798529103 ) ) ;
#29891 = CIRCLE ( 'NONE', #41697, 4.686499999999999666 ) ;
#29892 = VECTOR ( 'NONE', #24741, 1000.000000000000114 ) ;
#29893 = CARTESIAN_POINT ( 'NONE',  ( -15.07489245205697159, -21.40335507889944111, 65.40596683994178306 ) ) ;
#29894 = CARTESIAN_POINT ( 'NONE',  ( -10.88286923018596575, -17.43962093083235843, 68.11193994895104709 ) ) ;
#29895 = EDGE_LOOP ( 'NONE', ( #41990, #14991, #14648, #22972, #42158 ) ) ;
#29896 = CARTESIAN_POINT ( 'NONE',  ( -11.45656716003344933, -19.26928393672501727, 71.73039932227760573 ) ) ;
#29897 = FACE_OUTER_BOUND ( 'NONE', #47236, .T. ) ;
#29898 = AXIS2_PLACEMENT_3D ( 'NONE', #24823, #14185, #44040 ) ;
#29899 = CARTESIAN_POINT ( 'NONE',  ( -22.09321184435721719, -14.28490438881294367, 49.52966884056655772 ) ) ;
#29900 = CARTESIAN_POINT ( 'NONE',  ( -50.42609385541305755, -14.90920654474420104, 66.05294117647058272 ) ) ;
#29901 = CARTESIAN_POINT ( 'NONE',  ( -20.38659385650551670, -9.302874398569244363, 51.68646062012417985 ) ) ;
#29902 = ORIENTED_EDGE ( 'NONE', *, *, #19647, .T. ) ;
#29903 = CARTESIAN_POINT ( 'NONE',  ( -17.69342360693616456, -22.25450524205111691, 58.54519988936747410 ) ) ;
#29904 = CARTESIAN_POINT ( 'NONE',  ( -24.71300512064630794, -13.26796065199660113, 59.61913874400077873 ) ) ;
#29905 = EDGE_LOOP ( 'NONE', ( #46418, #27844 ) ) ;
#29906 = CARTESIAN_POINT ( 'NONE',  ( -8.424093855413063991, -25.10920654474410441, 48.99999999999997868 ) ) ;
#29907 = DIRECTION ( 'NONE',  ( 0.9687793358424822143, -0.2479245821708672415, 0.000000000000000000 ) ) ;
#29908 = CARTESIAN_POINT ( 'NONE',  ( -15.10382451463400955, -18.89477942154363532, 52.02966884056656482 ) ) ;
#29909 = ORIENTED_EDGE ( 'NONE', *, *, #2776, .T. ) ;
#29910 = DIRECTION ( 'NONE',  ( -0.7700094066334552956, -0.6380325334150243055, -2.326497556385353503E-17 ) ) ;
#29911 = CARTESIAN_POINT ( 'NONE',  ( -23.47627603871685409, -18.32658462313428060, 72.99041477383734389 ) ) ;
#29912 = ORIENTED_EDGE ( 'NONE', *, *, #37338, .F. ) ;
#29913 = VERTEX_POINT ( 'NONE', #39950 ) ;
#29914 = CARTESIAN_POINT ( 'NONE',  ( -13.29909385650551812, -8.114302828567740988, 52.18300498402516041 ) ) ;
#29915 = CARTESIAN_POINT ( 'NONE',  ( -12.84690951644825851, -8.931012861620404308, 67.56438176077992352 ) ) ;
#29916 = DIRECTION ( 'NONE',  ( -2.201155566701781786E-06, -7.355553121729402965E-06, -0.9999999999705254661 ) ) ;
#29917 = CARTESIAN_POINT ( 'NONE',  ( -21.01334446694451685, -11.79580940901521657, 52.02966884056656482 ) ) ;
#29918 = CARTESIAN_POINT ( 'NONE',  ( -19.37616851487812752, -21.99900361761337919, 58.71002773933979313 ) ) ;
#29919 = ORIENTED_EDGE ( 'NONE', *, *, #3322, .F. ) ;
#29920 = ORIENTED_EDGE ( 'NONE', *, *, #41515, .F. ) ;
#29921 = CARTESIAN_POINT ( 'NONE',  ( -14.45534385650551989, -7.417179338643134834, 52.18511593390279302 ) ) ;
#29922 = EDGE_CURVE ( 'NONE', #15790, #34971, #22537, .T. ) ;
#29923 = AXIS2_PLACEMENT_3D ( 'NONE', #32717, #44082, #21170 ) ;
#29924 = DIRECTION ( 'NONE',  ( 0.000000000000000000, 0.000000000000000000, 1.000000000000000000 ) ) ;
#29925 = CARTESIAN_POINT ( 'NONE',  ( -23.52949419687348964, -11.28347464189849525, 70.17738639980606763 ) ) ;
#29926 = CARTESIAN_POINT ( 'NONE',  ( -14.51159385650551492, -6.922745924619793101, 51.69366785382590024 ) ) ;
#29927 = AXIS2_PLACEMENT_3D ( 'NONE', #36375, #14668, #32462 ) ;
#29928 = EDGE_LOOP ( 'NONE', ( #34155, #46337, #8111, #45959, #5252 ) ) ;
#29929 = DIRECTION ( 'NONE',  ( -0.9687793358424822143, 0.2479245821708672415, 0.000000000000000000 ) ) ;
#29930 = CARTESIAN_POINT ( 'NONE',  ( -10.48480550552488744, -16.05393363305330823, 68.27767801788075985 ) ) ;
#29931 = AXIS2_PLACEMENT_3D ( 'NONE', #21560, #36312, #44700 ) ;
#29932 = CARTESIAN_POINT ( 'NONE',  ( -11.41947236009895228, -18.50911967460687535, 65.16195962094886340 ) ) ;
#29933 = ORIENTED_EDGE ( 'NONE', *, *, #34707, .T. ) ;
#29934 = LINE ( 'NONE', #33853, #41423 ) ;
#29935 = EDGE_CURVE ( 'NONE', #17825, #20557, #15847, .T. ) ;
#29936 = ORIENTED_EDGE ( 'NONE', *, *, #43597, .F. ) ;
#29937 = B_SPLINE_CURVE_WITH_KNOTS ( 'NONE', 3,
 ( #11426, #7760, #363, #3805, #44692, #30407, #10949, #2643, #41720, #8008 ),
 .UNSPECIFIED., .F., .F.,
 ( 4, 2, 2, 2, 4 ),
 ( 0.6272669072877923302, 0.7522669073072929535, 0.8772669073267936879, 1.002266907346294422, 1.127266907365795046 ),
 .UNSPECIFIED. ) ;
#29938 = CYLINDRICAL_SURFACE ( 'NONE', #26060, 0.1499999999999991063 ) ;
#29939 = DIRECTION ( 'NONE',  ( -1.000000000000000000, 0.000000000000000000, 9.637352644315596475E-17 ) ) ;
#29940 = EDGE_CURVE ( 'NONE', #27443, #9159, #22152, .T. ) ;
#29942 = ADVANCED_FACE ( 'NONE', ( #43166 ), #27577, .T. ) ;
#29941 = DIRECTION ( 'NONE',  ( 0.9757441136919974278, 0.2189141945955503377, 0.000000000000000000 ) ) ;
#29943 = CARTESIAN_POINT ( 'NONE',  ( -9.989595930756898667, -14.32624556671389549, 64.54837224505392612 ) ) ;
#29944 = MECHANICAL_DESIGN_GEOMETRIC_PRESENTATION_REPRESENTATION (  '', ( #2418 ), #22107 ) ;
#29945 = EDGE_LOOP ( 'NONE', ( #38862, #44514, #8683, #29045, #37024 ) ) ;
#29946 = CARTESIAN_POINT ( 'NONE',  ( -10.40174226954351866, -17.29724918936392442, 61.34238429002267878 ) ) ;
#29947 = CARTESIAN_POINT ( 'NONE',  ( -16.50454536406711981, -22.20232556258728351, 65.34068991928313608 ) ) ;
#29948 = DIRECTION ( 'NONE',  ( 0.5088156898428700670, 0.8608754809899751281, 5.922709712265243479E-08 ) ) ;
#29949 = CARTESIAN_POINT ( 'NONE',  ( -10.07931644449276476, -16.05763419655898616, 68.15580616013423310 ) ) ;
#29950 = ORIENTED_EDGE ( 'NONE', *, *, #29678, .T. ) ;
#29951 = CARTESIAN_POINT ( 'NONE',  ( -10.37497031247464463, -14.69804315800203298, 71.62782692816419683 ) ) ;
#29952 = CARTESIAN_POINT ( 'NONE',  ( -17.15992076746773876, -7.363842158706400021, 70.59697549560173968 ) ) ;
#29953 = CARTESIAN_POINT ( 'NONE',  ( -18.76558392140857023, -7.480892851696864021, 70.55563303198719893 ) ) ;
#29954 = FACE_BOUND ( 'NONE', #30978, .T. ) ;
#29955 = VERTEX_POINT ( 'NONE', #2036 ) ;
#29956 = CARTESIAN_POINT ( 'NONE',  ( -13.11455056595802660, -20.88644485624005398, 58.20796624012236720 ) ) ;
#29957 = CARTESIAN_POINT ( 'NONE',  ( -10.53944148391707891, -16.08179225747893071, 71.67580357262283997 ) ) ;
#29958 = CARTESIAN_POINT ( 'NONE',  ( -16.09584876169039802, -7.477806291315723719, 63.85666425603482566 ) ) ;
#29959 = ORIENTED_EDGE ( 'NONE', *, *, #42149, .F. ) ;
#29960 = DIRECTION ( 'NONE',  ( 0.9687793358424821033, -0.2479245821708677133, 0.000000000000000000 ) ) ;
#29961 = ORIENTED_EDGE ( 'NONE', *, *, #8617, .F. ) ;
#29962 = DIRECTION ( 'NONE',  ( -0.9529680021988312655, 0.3030709269876716294, 3.918663088761644638E-08 ) ) ;
#29963 = CARTESIAN_POINT ( 'NONE',  ( -47.22409385541305937, -12.70920654474410760, 70.87000000000000455 ) ) ;
#29964 = CARTESIAN_POINT ( 'NONE',  ( -14.07539642552819359, -8.605278304397881328, 74.19954655214911554 ) ) ;
#29965 = EDGE_LOOP ( 'NONE', ( #19115, #35092 ) ) ;
#29966 = FACE_OUTER_BOUND ( 'NONE', #26789, .T. ) ;
#29967 = AXIS2_PLACEMENT_3D ( 'NONE', #1794, #35747, #43415 ) ;
#29968 = CARTESIAN_POINT ( 'NONE',  ( -11.00648394673626562, -17.60476015118163673, 68.17010079748926898 ) ) ;
#29969 = EDGE_LOOP ( 'NONE', ( #34102, #45682, #47413, #1910 ) ) ;
#29970 = EDGE_CURVE ( 'NONE', #9317, #41086, #24703, .T. ) ;
#29971 = ORIENTED_EDGE ( 'NONE', *, *, #6560, .F. ) ;
#29972 = ORIENTED_EDGE ( 'NONE', *, *, #24708, .T. ) ;
#29973 = CARTESIAN_POINT ( 'NONE',  ( -15.79261328423922706, -21.67602794760135154, 72.20142491214876657 ) ) ;
#29974 = CARTESIAN_POINT ( 'NONE',  ( -22.34470957656571599, -19.78791530553215949, 69.47417989488683077 ) ) ;
#29975 = AXIS2_PLACEMENT_3D ( 'NONE', #27972, #5587, #16645 ) ;
#29976 = CARTESIAN_POINT ( 'NONE',  ( -12.45502217426375680, -20.36096218193827667, 71.99308960123012469 ) ) ;
#29977 = CARTESIAN_POINT ( 'NONE',  ( -10.57110082969170683, -13.38215148069720861, 74.67817647591368768 ) ) ;
#29978 = CARTESIAN_POINT ( 'NONE',  ( -10.40174263535760524, -17.29725023780839166, 61.34238537770443855 ) ) ;
#29979 = LINE ( 'NONE', #45016, #41241 ) ;
#29980 = CARTESIAN_POINT ( 'NONE',  ( -10.39241571269986331, -17.41794234916963191, 54.27966884056652219 ) ) ;
#29981 = VERTEX_POINT ( 'NONE', #39470 ) ;
#29982 = ORIENTED_EDGE ( 'NONE', *, *, #25791, .T. ) ;
#29983 = CARTESIAN_POINT ( 'NONE',  ( -16.46477641927899782, -7.821750181629138154, 60.61517342399707076 ) ) ;
#29984 = VECTOR ( 'NONE', #10011, 1000.000000000000000 ) ;
#29985 = ADVANCED_FACE ( 'NONE', ( #5752 ), #20755, .T. ) ;
#29986 = PLANE ( 'NONE',  #30718 ) ;
#29987 = CARTESIAN_POINT ( 'NONE',  ( -11.89178972046640936, -10.43929686452144878, 71.11893105542935700 ) ) ;
#29988 = CYLINDRICAL_SURFACE ( 'NONE', #33871, 0.1500000000000028255 ) ;
#29989 = ORIENTED_EDGE ( 'NONE', *, *, #38306, .T. ) ;
#29990 = CARTESIAN_POINT ( 'NONE',  ( -17.40534385650551741, -8.801233750844183135, 48.81488406609782515 ) ) ;
#29991 = ORIENTED_EDGE ( 'NONE', *, *, #38582, .T. ) ;
#29992 =( GEOMETRIC_REPRESENTATION_CONTEXT ( 3 ) GLOBAL_UNCERTAINTY_ASSIGNED_CONTEXT ( ( #31709 ) ) GLOBAL_UNIT_ASSIGNED_CONTEXT ( ( #26344, #44574, #7894 ) ) REPRESENTATION_CONTEXT ( 'NONE', 'WORKASPACE' ) );
#29993 = LINE ( 'NONE', #26290, #35885 ) ;
#29994 = CARTESIAN_POINT ( 'NONE',  ( -11.96073139429061527, -19.87431630704028152, 57.97036459255868124 ) ) ;
#29995 = CIRCLE ( 'NONE', #43388, 2.000000000000000888 ) ;
#29996 = DIRECTION ( 'NONE',  ( -3.549360974551883545E-17, 6.371834667872732552E-18, 1.000000000000000000 ) ) ;
#29997 = ORIENTED_EDGE ( 'NONE', *, *, #36988, .T. ) ;
#29998 = CYLINDRICAL_SURFACE ( 'NONE', #43942, 0.3999999999999975797 ) ;
#29999 = AXIS2_PLACEMENT_3D ( 'NONE', #7907, #5834, #13186 ) ;
#30000 = CYLINDRICAL_SURFACE ( 'NONE', #18049, 0.1500000000000061007 ) ;
#30001 = CARTESIAN_POINT ( 'NONE',  ( -14.80624607021532135, -8.317144234858641738, 60.31996281969095719 ) ) ;
#30002 = ADVANCED_FACE ( 'NONE', ( #18841 ), #33206, .T. ) ;
#30003 = EDGE_CURVE ( 'NONE', #32441, #19332, #21915, .T. ) ;
#30004 = ORIENTED_EDGE ( 'NONE', *, *, #27819, .F. ) ;
#30005 = CARTESIAN_POINT ( 'NONE',  ( -22.72409385759798894, -9.359200813967568422, 50.49621490985803263 ) ) ;
#30006 =( BOUNDED_CURVE ( )  B_SPLINE_CURVE ( 3, ( #37760, #34065, #356, #22025 ),
 .UNSPECIFIED., .F., .F. ) 
 B_SPLINE_CURVE_WITH_KNOTS ( ( 4, 4 ),
 ( 0.5000000000000000000, 0.9074455897393618464 ),
 .UNSPECIFIED. ) 
 CURVE ( )  GEOMETRIC_REPRESENTATION_ITEM ( )  RATIONAL_B_SPLINE_CURVE ( ( 1.000000000000016653, 0.4567392136813336334, 0.3561768502900192201, 0.6983129098260912881 ) ) 
 REPRESENTATION_ITEM ( '' )  );
#30007 = CARTESIAN_POINT ( 'NONE',  ( -10.05862335131466700, -15.92885902279982524, 64.69266873560974318 ) ) ;
#30008 = CARTESIAN_POINT ( 'NONE',  ( -24.03783269458455862, -17.25936868619852760, 65.82868649746481537 ) ) ;
#30009 = ORIENTED_EDGE ( 'NONE', *, *, #40366, .F. ) ;
#30010 = DIRECTION ( 'NONE',  ( -0.4433615477241707459, 0.8963428685495451465, -2.661652803430156647E-08 ) ) ;
#30011 = VERTEX_POINT ( 'NONE', #3188 ) ;
#30012 = FACE_OUTER_BOUND ( 'NONE', #36210, .T. ) ;
#30013 = EDGE_CURVE ( 'NONE', #45327, #28927, #8413, .T. ) ;
#30014 = ADVANCED_FACE ( 'NONE', ( #10586 ), #44565, .T. ) ;
#30015 = CARTESIAN_POINT ( 'NONE',  ( -24.87290000513101873, -14.67112934921935974, 62.82801050733710468 ) ) ;
#30016 = VERTEX_POINT ( 'NONE', #14982 ) ;
#30017 = CARTESIAN_POINT ( 'NONE',  ( -22.09234465700630423, -20.09219189623108548, 62.23439162498055310 ) ) ;
#30018 = AXIS2_PLACEMENT_3D ( 'NONE', #46367, #45886, #11909 ) ;
#30019 = EDGE_CURVE ( 'NONE', #44359, #45444, #34823, .T. ) ;
#30020 = CARTESIAN_POINT ( 'NONE',  ( -20.60788153932096023, -8.518722016582882972, 63.32593600985608617 ) ) ;
#30021 = ORIENTED_EDGE ( 'NONE', *, *, #3076, .T. ) ;
#30022 = CARTESIAN_POINT ( 'NONE',  ( -14.62687819956926027, -8.392386103536567887, 64.08978840643771946 ) ) ;
#30023 = ADVANCED_FACE ( 'NONE', ( #29298 ), #25595, .T. ) ;
#30024 = DIRECTION ( 'NONE',  ( 0.7111926860893301727, -0.6953514824629924984, 0.1033986416233890065 ) ) ;
#30025 =( BOUNDED_CURVE ( )  B_SPLINE_CURVE ( 3, ( #38976, #6467, #20520, #42922 ),
 .UNSPECIFIED., .F., .F. ) 
 B_SPLINE_CURVE_WITH_KNOTS ( ( 4, 4 ),
 ( 0.5000000000000000000, 0.9074455897393682857 ),
 .UNSPECIFIED. ) 
 CURVE ( )  GEOMETRIC_REPRESENTATION_ITEM ( )  RATIONAL_B_SPLINE_CURVE ( ( 0.9999999999999892308, 0.4567392136813265835, 0.3561768502900357625, 0.6983129098261049439 ) ) 
 REPRESENTATION_ITEM ( '' )  );
#30026 = DIRECTION ( 'NONE',  ( -3.071710424422018668E-17, 6.404604876783312462E-16, 1.000000000000000000 ) ) ;
#30027 = ORIENTED_EDGE ( 'NONE', *, *, #1216, .T. ) ;
#30029 = CARTESIAN_POINT ( 'NONE',  ( -12.15399223456666178, -9.543296633619027247, 57.20440205305690995 ) ) ;
#30028 =( BOUNDED_SURFACE ( )  B_SPLINE_SURFACE ( 3, 1, ( 
 ( #27319, #5165 ),
 ( #27568, #42607 ),
 ( #4675, #9105 ),
 ( #42349, #23647 ),
 ( #38645, #19940 ),
 ( #46288, #20173 ),
 ( #1454, #23388 ) ),
 .UNSPECIFIED., .T., .F., .F. ) 
 B_SPLINE_SURFACE_WITH_KNOTS ( ( 4, 3, 4 ),
 ( 2, 2 ),
 ( 0.000000000000000000, 0.5000000000000000000, 1.000000000000000000 ),
 ( 0.000000000000000000, 1.000000000000000000 ),
 .UNSPECIFIED. ) 
 GEOMETRIC_REPRESENTATION_ITEM ( )  RATIONAL_B_SPLINE_SURFACE ( (
 ( 1.000000000000000000, 1.000000000000000000),
 ( 0.3333333333333335369, 0.3333333333333330373),
 ( 0.3333333333333335369, 0.3333333333333330373),
 ( 1.000000000000000000, 1.000000000000000000),
 ( 0.3333333333333333703, 0.3333333333333333703),
 ( 0.3333333333333333703, 0.3333333333333333703),
 ( 1.000000000000000000, 1.000000000000000000) ) ) 
 REPRESENTATION_ITEM ( '' )  SURFACE ( )  );
#30030 = B_SPLINE_CURVE_WITH_KNOTS ( 'NONE', 3,
 ( #32008, #39146, #43591, #39398, #31277, #28562, #16964, #43089, #9369, #28325 ),
 .UNSPECIFIED., .F., .F.,
 ( 4, 2, 2, 2, 4 ),
 ( 0.000000000000000000, 0.2500000000000000000, 0.5000000000000000000, 0.7500000000000000000, 1.000000000000000000 ),
 .UNSPECIFIED. ) ;
#30031 = CARTESIAN_POINT ( 'NONE',  ( -13.33151401730585306, -20.55006798877650454, 58.06122216312902395 ) ) ;
#30032 = AXIS2_PLACEMENT_3D ( 'NONE', #7286, #17845, #7529 ) ;
#30033 = CARTESIAN_POINT ( 'NONE',  ( -15.92409385541305333, -14.80920654474410547, 52.21286476528345588 ) ) ;
#30034 = ADVANCED_FACE ( 'NONE', ( #11319 ), #40861, .F. ) ;
#30035 = ORIENTED_EDGE ( 'NONE', *, *, #2760, .F. ) ;
#30036 = VERTEX_POINT ( 'NONE', #44822 ) ;
#30037 = AXIS2_PLACEMENT_3D ( 'NONE', #14478, #6649, #2937 ) ;
#30038 = CARTESIAN_POINT ( 'NONE',  ( -24.26595340233995302, -13.32969406988797623, 59.36267925071750540 ) ) ;
#30039 = CARTESIAN_POINT ( 'NONE',  ( -24.25510706449861686, -16.56479617024167084, 59.53821300994621168 ) ) ;
#30040 = FACE_OUTER_BOUND ( 'NONE', #41546, .T. ) ;
#30041 = LINE ( 'NONE', #479, #33859 ) ;
#30042 = CARTESIAN_POINT ( 'NONE',  ( -14.90534385759799463, -7.595227055684746986, 51.75156210489594599 ) ) ;
#30043 = FACE_OUTER_BOUND ( 'NONE', #24566, .T. ) ;
#30044 = CARTESIAN_POINT ( 'NONE',  ( -12.15935936027619668, -9.537873432754242486, 57.21218613097342143 ) ) ;
#30045 = FACE_OUTER_BOUND ( 'NONE', #38173, .T. ) ;
#30046 =( BOUNDED_CURVE ( )  B_SPLINE_CURVE ( 3, ( #26491, #41025, #7798, #22815 ),
 .UNSPECIFIED., .F., .F. ) 
 B_SPLINE_CURVE_WITH_KNOTS ( ( 4, 4 ),
 ( 0.5000000000000000000, 0.9074455897393733927 ),
 .UNSPECIFIED. ) 
 CURVE ( )  GEOMETRIC_REPRESENTATION_ITEM ( )  RATIONAL_B_SPLINE_CURVE ( ( 0.9999999999999990008, 0.4567392136813159809, 0.3561768502900249933, 0.6983129098261249279 ) ) 
 REPRESENTATION_ITEM ( '' )  );
#30047 = CARTESIAN_POINT ( 'NONE',  ( -16.50454536406711981, -22.20232556258728351, 65.34068991928313608 ) ) ;
#30048 = ORIENTED_EDGE ( 'NONE', *, *, #28979, .T. ) ;
#30049 = DIRECTION ( 'NONE',  ( -1.000000000000000000, -2.866981220435666553E-17, 0.000000000000000000 ) ) ;
#30050 = B_SPLINE_CURVE_WITH_KNOTS ( 'NONE', 1,
 ( #29253, #10540 ),
 .UNSPECIFIED., .F., .F.,
 ( 2, 2 ),
 ( 0.000000000000000000, 1.000000000000000000 ),
 .UNSPECIFIED. ) ;
#30051 = AXIS2_PLACEMENT_3D ( 'NONE', #20780, #35785, #2064 ) ;
#30052 = CARTESIAN_POINT ( 'NONE',  ( -19.92776479198160189, -21.39998277484045275, 72.41950795000725805 ) ) ;
#30053 = CYLINDRICAL_SURFACE ( 'NONE', #27592, 4.686499999999997002 ) ;
#30054 = EDGE_LOOP ( 'NONE', ( #14587, #9740, #46539, #511, #46685 ) ) ;
#30055 = EDGE_LOOP ( 'NONE', ( #9976, #1901, #5168, #4101, #5051 ) ) ;
#30056 = CARTESIAN_POINT ( 'NONE',  ( -17.70250950100762566, -21.85374724789173584, 58.40553377166283866 ) ) ;
#30057 = SURFACE_STYLE_USAGE ( .BOTH. , #29547 ) ;
#30058 = CARTESIAN_POINT ( 'NONE',  ( -22.06352460594304787, -8.980016202103444201, 63.37649054182217867 ) ) ;
#30059 = PLANE ( 'NONE',  #22513 ) ;
#30060 = EDGE_CURVE ( 'NONE', #43790, #35496, #25997, .T. ) ;
#30061 = ORIENTED_EDGE ( 'NONE', *, *, #38030, .T. ) ;
#30062 = CARTESIAN_POINT ( 'NONE',  ( -22.72031779163844689, -16.29245029320677673, 53.49999999999995026 ) ) ;
#30063 = CARTESIAN_POINT ( 'NONE',  ( -23.00441852451001523, -19.11762575345012749, 58.88410642058938294 ) ) ;
#30064 = ADVANCED_FACE ( 'NONE', ( #26333 ), #22395, .T. ) ;
#30065 = VERTEX_POINT ( 'NONE', #14002 ) ;
#30066 = AXIS2_PLACEMENT_3D ( 'NONE', #37773, #30170, #3316 ) ;
#30067 = CARTESIAN_POINT ( 'NONE',  ( 18.57590614458695200, 1.636933384339416264, 51.78951792648778252 ) ) ;
#30068 = LINE ( 'NONE', #33719, #33583 ) ;
#30069 = CARTESIAN_POINT ( 'NONE',  ( -10.83447761903821061, -17.17455418348055218, 64.69909585894313864 ) ) ;
#30070 = ORIENTED_EDGE ( 'NONE', *, *, #6068, .T. ) ;
#30071 = CARTESIAN_POINT ( 'NONE',  ( -21.71715435735689326, -9.279671086701025473, 66.94533469040406715 ) ) ;
#30072 = ORIENTED_EDGE ( 'NONE', *, *, #40353, .T. ) ;
#30073 = CARTESIAN_POINT ( 'NONE',  ( -19.57546054543010783, -21.94189796748987575, 62.03857704761023939 ) ) ;
#30074 = DIRECTION ( 'NONE',  ( -1.000000000000000000, -2.866981220435666553E-17, 0.000000000000000000 ) ) ;
#30075 = EDGE_LOOP ( 'NONE', ( #40447, #42157, #18587, #33476 ) ) ;
#30076 = CARTESIAN_POINT ( 'NONE',  ( -15.13017050835524913, -18.89591645955643884, 49.52966884056656482 ) ) ;
#30077 = CARTESIAN_POINT ( 'NONE',  ( -10.29385348138020539, -12.64970417265235803, 64.38340698725603772 ) ) ;
#30078 = EDGE_CURVE ( 'NONE', #13279, #32426, #2493, .T. ) ;
#30079 = CARTESIAN_POINT ( 'NONE',  ( -20.08034385650551812, -6.424090610841176385, 49.80797279389978627 ) ) ;
#30080 = CARTESIAN_POINT ( 'NONE',  ( -10.70532053225239366, -12.67267096592666675, 61.08381491717225487 ) ) ;
#30081 = EDGE_CURVE ( 'NONE', #35856, #508, #47707, .T. ) ;
#30082 = CARTESIAN_POINT ( 'NONE',  ( -23.96654618570108042, -17.44381333609114648, 62.35872369075587329 ) ) ;
#30083 = DIRECTION ( 'NONE',  ( 6.312331213287273068E-07, 6.220915576652692866E-06, 0.9999999999804508599 ) ) ;
#30084 = CARTESIAN_POINT ( 'NONE',  ( -17.20472057461396176, -21.85940646863547343, 72.37363138342533375 ) ) ;
#30085 = ORIENTED_EDGE ( 'NONE', *, *, #24068, .T. ) ;
#30086 = CARTESIAN_POINT ( 'NONE',  ( -10.43291801062321866, -14.45783718407127694, 64.49689883712670735 ) ) ;
#30087 = LINE ( 'NONE', #25636, #23467 ) ;
#30088 = CARTESIAN_POINT ( 'NONE',  ( -42.68438797306012589, -14.80920654474413745, 60.91764705882351905 ) ) ;
#30089 = CARTESIAN_POINT ( 'NONE',  ( -12.54046192938994153, -19.89396152535205076, 65.16115129690373919 ) ) ;
#30090 = CYLINDRICAL_SURFACE ( 'NONE', #27460, 2.500000000000001332 ) ;
#30091 = CARTESIAN_POINT ( 'NONE',  ( -24.18432332345330948, -12.99280965528459930, 63.02367257271272649 ) ) ;
#30092 = VERTEX_POINT ( 'NONE', #36656 ) ;
#30093 = ORIENTED_EDGE ( 'NONE', *, *, #35779, .F. ) ;
#30094 = CARTESIAN_POINT ( 'NONE',  ( -23.62594491300536959, -11.45603751788689095, 66.70742424642772050 ) ) ;
#30095 = CARTESIAN_POINT ( 'NONE',  ( -10.47550909334574598, -13.59594187864236581, 74.67817481325579365 ) ) ;
#30096 = ORIENTED_EDGE ( 'NONE', *, *, #5872, .T. ) ;
#30097 = CARTESIAN_POINT ( 'NONE',  ( -24.03794070092309454, -17.10236419872843783, 73.18336037747248213 ) ) ;
#30098 = CARTESIAN_POINT ( 'NONE',  ( -24.20826260513847217, -13.07918714609906452, 66.37417080772955558 ) ) ;
#30099 = CARTESIAN_POINT ( 'NONE',  ( -12.50376665500426654, -9.829597046481099554, 57.10552118696781321 ) ) ;
#30100 = DIRECTION ( 'NONE',  ( -0.5729733056696844073, 0.8195740302071247152, 7.403245352187747277E-08 ) ) ;
#30101 = EDGE_CURVE ( 'NONE', #33816, #46437, #42589, .T. ) ;
#30102 = CARTESIAN_POINT ( 'NONE',  ( -23.38410589725464916, -10.33907962427212190, 59.71708035543083071 ) ) ;
#30103 = DIRECTION ( 'NONE',  ( 0.9687793358424821033, -0.2479245821708679909, 0.000000000000000000 ) ) ;
#30104 = CARTESIAN_POINT ( 'NONE',  ( -14.06267692155865312, -8.668962760654556732, 74.49954661250710330 ) ) ;
#30105 = CARTESIAN_POINT ( 'NONE',  ( 7.325906144586951996, -6.109215713985405749, 50.50605614422795497 ) ) ;
#30106 = CARTESIAN_POINT ( 'NONE',  ( -42.79045946627278596, -14.90920654474414775, 60.06907511312216741 ) ) ;
#30107 = PRODUCT_RELATED_PRODUCT_CATEGORY ( 'part', '', ( #8746 ) ) ;
#30108 = ORIENTED_EDGE ( 'NONE', *, *, #31913, .F. ) ;
#30109 = DIRECTION ( 'NONE',  ( 9.880513543698878618E-06, 1.241746734295183170E-06, -0.9999999999504167736 ) ) ;
#30110 = DIRECTION ( 'NONE',  ( -0.6538427738826437796, -0.7566304428460742804, 5.916677973164435741E-08 ) ) ;
#30111 = CARTESIAN_POINT ( 'NONE',  ( -12.10599200002982556, -20.02663609087960239, 61.58174067880212021 ) ) ;
#30112 = CARTESIAN_POINT ( 'NONE',  ( -20.75534385759799250, -8.623186033802570094, 49.24843789510466507 ) ) ;
#30113 = FACE_OUTER_BOUND ( 'NONE', #42163, .T. ) ;
#30114 = CARTESIAN_POINT ( 'NONE',  ( -11.81178328723415660, -10.62567094834893311, 74.73885052262691886 ) ) ;
#30115 = CARTESIAN_POINT ( 'NONE',  ( -18.05316936118225968, -22.23335149483498085, 65.53187476518867527 ) ) ;
#30116 = VERTEX_POINT ( 'NONE', #37898 ) ;
#30117 = ORIENTED_EDGE ( 'NONE', *, *, #44807, .T. ) ;
#30118 = CARTESIAN_POINT ( 'NONE',  ( -14.53659385541304339, -8.995762431863214559, 51.38120296130585274 ) ) ;
#30119 = VERTEX_POINT ( 'NONE', #46025 ) ;
#30120 = CARTESIAN_POINT ( 'NONE',  ( -15.74909385759799108, -8.112991634885936776, 51.74999426922421719 ) ) ;
#30121 = DIRECTION ( 'NONE',  ( -3.071710424422018668E-17, 6.404604876783312462E-16, 1.000000000000000000 ) ) ;
#30122 =( BOUNDED_CURVE ( )  B_SPLINE_CURVE ( 3, ( #48277, #32770, #36223, #6919 ),
 .UNSPECIFIED., .F., .F. ) 
 B_SPLINE_CURVE_WITH_KNOTS ( ( 4, 4 ),
 ( 0.000000000000000000, 0.4074455897393698955 ),
 .UNSPECIFIED. ) 
 CURVE ( )  GEOMETRIC_REPRESENTATION_ITEM ( )  RATIONAL_B_SPLINE_CURVE ( ( 1.000000000000000000, 0.4567392136813278603, 0.3561768502900287681, 0.6983129098261027234 ) ) 
 REPRESENTATION_ITEM ( '' )  );
#30123 = ADVANCED_FACE ( 'NONE', ( #12523 ), #13485, .T. ) ;
#30124 = CARTESIAN_POINT ( 'NONE',  ( -11.30361205576526196, -11.41219277671509147, 64.44882039656690154 ) ) ;
#30125 = CARTESIAN_POINT ( 'NONE',  ( -16.16379340615718618, -22.15191857530921382, 58.47080845268740035 ) ) ;
#30126 = AXIS2_PLACEMENT_3D ( 'NONE', #7230, #44187, #36732 ) ;
#30127 = ORIENTED_EDGE ( 'NONE', *, *, #38941, .T. ) ;
#30128 = DIRECTION ( 'NONE',  ( 0.9687793358424819923, -0.2479245821708678799, 3.596521012361014201E-17 ) ) ;
#30129 = CARTESIAN_POINT ( 'NONE',  ( -24.20371252810814866, -12.87440185077122834, 66.58774614429587757 ) ) ;
#30130 = ORIENTED_EDGE ( 'NONE', *, *, #41302, .F. ) ;
#30131 = FACE_OUTER_BOUND ( 'NONE', #32251, .T. ) ;
#30132 = CARTESIAN_POINT ( 'NONE',  ( -6.424093855413058662, -6.859206544744110623, 52.99999999999998579 ) ) ;
#30133 = ORIENTED_EDGE ( 'NONE', *, *, #19406, .T. ) ;
#30134 = CARTESIAN_POINT ( 'NONE',  ( -23.38417127501956116, -19.28035200660907122, 62.54062256979923973 ) ) ;
#30135 = CARTESIAN_POINT ( 'NONE',  ( -17.42409385541299471, -14.80920654474435771, 49.52966884056655772 ) ) ;
#30136 = CARTESIAN_POINT ( 'NONE',  ( -22.07022430586338402, -11.86582892075562334, 54.07175714974878389 ) ) ;
#30137 = ORIENTED_EDGE ( 'NONE', *, *, #12533, .T. ) ;
#30138 = CARTESIAN_POINT ( 'NONE',  ( -10.89280197141400919, -11.22507430941316642, 64.33377434530349603 ) ) ;
#30139 = EDGE_CURVE ( 'NONE', #34661, #575, #7289, .T. ) ;
#30140 = CARTESIAN_POINT ( 'NONE',  ( -17.42409385541299471, -14.80920654474435594, 52.02966884056656482 ) ) ;
#30141 = EDGE_CURVE ( 'NONE', #12343, #1510, #23372, .T. ) ;
#30142 = CARTESIAN_POINT ( 'NONE',  ( -27.42409385541305156, -14.65920654474411045, 48.99999999999997868 ) ) ;
#30143 = CARTESIAN_POINT ( 'NONE',  ( -23.96382046939319821, -17.30576672235113378, 66.01645378202925940 ) ) ;
#30144 = VERTEX_POINT ( 'NONE', #30776 ) ;
#30145 = LINE ( 'NONE', #25950, #39977 ) ;
#30146 = CARTESIAN_POINT ( 'NONE',  ( -10.92750425249182022, -11.16255029878774252, 64.26386639478288032 ) ) ;
#30147 = CARTESIAN_POINT ( 'NONE',  ( -10.39074299160501980, -14.27365074699323522, 68.15800167629423356 ) ) ;
#30148 = CARTESIAN_POINT ( 'NONE',  ( -20.94708704702029323, -20.85805098747363928, 62.22357391611139832 ) ) ;
#30149 = EDGE_CURVE ( 'NONE', #1086, #42645, #41095, .T. ) ;
#30150 = CARTESIAN_POINT ( 'NONE',  ( -50.42409385541304800, -15.80920654474410725, 74.99999999999998579 ) ) ;
#30151 = CARTESIAN_POINT ( 'NONE',  ( -19.93659385650551741, -6.915538690918074494, 49.31353937987644542 ) ) ;
#30152 = EDGE_LOOP ( 'NONE', ( #20205, #13097, #34198, #17220, #34067 ) ) ;
#30153 = FACE_OUTER_BOUND ( 'NONE', #20959, .T. ) ;
#30154 = CARTESIAN_POINT ( 'NONE',  ( -21.37409385759799108, -6.859212275519751323, 50.50378509014259265 ) ) ;
#30155 = VERTEX_POINT ( 'NONE', #46266 ) ;
#30156 = CARTESIAN_POINT ( 'NONE',  ( -24.72409385541305582, -14.80920654474414810, 61.92352941176469727 ) ) ;
#30157 = ADVANCED_FACE ( 'NONE', ( #19922 ), #19189, .T. ) ;
#30158 = CARTESIAN_POINT ( 'NONE',  ( -22.55199058362584452, -10.04362098402029346, 73.49777690555987419 ) ) ;
#30159 = FACE_OUTER_BOUND ( 'NONE', #27352, .T. ) ;
#30160 = EDGE_CURVE ( 'NONE', #30521, #10974, #36269, .T. ) ;
#30161 = ORIENTED_EDGE ( 'NONE', *, *, #9765, .F. ) ;
#30162 = CARTESIAN_POINT ( 'NONE',  ( -14.72744631621160494, -8.295007313424175521, 60.60524229057013201 ) ) ;
#30163 = PLANE ( 'NONE',  #48503 ) ;
#30164 = B_SPLINE_CURVE_WITH_KNOTS ( 'NONE', 3,
 ( #5998, #39493, #5039, #35547, #47127, #1822, #17060, #5773, #27683, #12412 ),
 .UNSPECIFIED., .F., .F.,
 ( 4, 2, 2, 2, 4 ),
 ( 0.1272669073658617700, 0.2522669073463401634, 0.3772669073268185014, 0.5022669073072968393, 0.6272669072877752328 ),
 .UNSPECIFIED. ) ;
#30165 = DIRECTION ( 'NONE',  ( 0.000000000000000000, 0.000000000000000000, 1.000000000000000000 ) ) ;
#30166 = EDGE_LOOP ( 'NONE', ( #1816, #7869, #5888, #45334 ) ) ;
#30167 = VECTOR ( 'NONE', #23292, 1000.000000000000000 ) ;
#30168 = CARTESIAN_POINT ( 'NONE',  ( -14.14284385650552167, -8.811426318492348031, 52.18089403414752070 ) ) ;
#30169 = CARTESIAN_POINT ( 'NONE',  ( -12.84137621205286628, -8.935279004184852880, 67.50130000652654871 ) ) ;
#30170 = DIRECTION ( 'NONE',  ( -0.5881408891789771110, -0.8087584895849666555, 7.565907428972492613E-08 ) ) ;
#30171 =( BOUNDED_SURFACE ( )  B_SPLINE_SURFACE ( 3, 1, ( 
 ( #38835, #20375 ),
 ( #30976, #30742 ),
 ( #42053, #15932 ),
 ( #23835, #934 ),
 ( #9294, #8327 ),
 ( #45769, #1161 ),
 ( #16661, #24316 ) ),
 .UNSPECIFIED., .T., .F., .F. ) 
 B_SPLINE_SURFACE_WITH_KNOTS ( ( 4, 3, 4 ),
 ( 2, 2 ),
 ( 0.000000000000000000, 0.5000000000000000000, 1.000000000000000000 ),
 ( 0.000000000000000000, 1.000000000000000000 ),
 .UNSPECIFIED. ) 
 GEOMETRIC_REPRESENTATION_ITEM ( )  RATIONAL_B_SPLINE_SURFACE ( (
 ( 1.000000000000000000, 1.000000000000000000),
 ( 0.3333333333333335369, 0.3333333333333330373),
 ( 0.3333333333333335369, 0.3333333333333330373),
 ( 1.000000000000000000, 1.000000000000000000),
 ( 0.3333333333333333703, 0.3333333333333333703),
 ( 0.3333333333333333703, 0.3333333333333333703),
 ( 1.000000000000000000, 1.000000000000000000) ) ) 
 REPRESENTATION_ITEM ( '' )  SURFACE ( )  );
#30172 = CARTESIAN_POINT ( 'NONE',  ( -24.85419441251774941, -14.26332397151243647, 69.77558371844806118 ) ) ;
#30173 = DIRECTION ( 'NONE',  ( 0.000000000000000000, 0.000000000000000000, 1.000000000000000000 ) ) ;
#30174 = EDGE_CURVE ( 'NONE', #45761, #936, #34180, .T. ) ;
#30175 = ORIENTED_EDGE ( 'NONE', *, *, #1683, .T. ) ;
#30176 = ORIENTED_EDGE ( 'NONE', *, *, #25609, .T. ) ;
#30177 = CARTESIAN_POINT ( 'NONE',  ( -15.52409385650551421, -6.426201560718813433, 50.50509628382439331 ) ) ;
#30178 = CYLINDRICAL_SURFACE ( 'NONE', #15036, 4.686499999999997002 ) ;
#30179 = FILL_AREA_STYLE_COLOUR ( '', #29202 ) ;
#30180 = EDGE_CURVE ( 'NONE', #15909, #2586, #26646, .T. ) ;
#30181 = CARTESIAN_POINT ( 'NONE',  ( -16.76159385650551314, -9.295667164867525756, 49.30633214617472504 ) ) ;
#30182 =( BOUNDED_CURVE ( )  B_SPLINE_CURVE ( 3, ( #40290, #6559, #44723, #33350 ),
 .UNSPECIFIED., .F., .F. ) 
 B_SPLINE_CURVE_WITH_KNOTS ( ( 4, 4 ),
 ( 0.4074455897393631787, 0.5000000000000000000 ),
 .UNSPECIFIED. ) 
 CURVE ( )  GEOMETRIC_REPRESENTATION_ITEM ( )  RATIONAL_B_SPLINE_CURVE ( ( 0.6983129098261022794, 0.7760317562607047526, 0.8765941196520036227, 0.9999999999999977796 ) ) 
 REPRESENTATION_ITEM ( '' )  );
#30183 = CARTESIAN_POINT ( 'NONE',  ( -10.80190757246176325, -17.07816907218938951, 61.45743131804429282 ) ) ;
#30184 = CARTESIAN_POINT ( 'NONE',  ( -20.42942694929465119, -8.423054519096806914, 59.99692253513481432 ) ) ;
#30185 = DIRECTION ( 'NONE',  ( 3.484385612528001215E-15, 0.000000000000000000, -1.000000000000000000 ) ) ;
#30186 = CARTESIAN_POINT ( 'NONE',  ( -23.78373255665641750, -17.85216390223663652, 59.00938192581773478 ) ) ;
#30187 = ORIENTED_EDGE ( 'NONE', *, *, #37615, .T. ) ;
#30188 = CARTESIAN_POINT ( 'NONE',  ( -12.36794899618824140, -19.72224014812425708, 61.69678633597966666 ) ) ;
#30189 = EDGE_CURVE ( 'NONE', #27648, #44379, #4008, .T. ) ;
#30190 = VERTEX_POINT ( 'NONE', #34927 ) ;
#30191 = CARTESIAN_POINT ( 'NONE',  ( -10.41569439578338496, -15.57669382292980131, 61.05261153187079515 ) ) ;
#30192 = CARTESIAN_POINT ( 'NONE',  ( -18.17450402892199790, -21.77015454618090473, 68.88685014060939693 ) ) ;
#30193 = CARTESIAN_POINT ( 'NONE',  ( -24.42140808089354920, -17.36692438891622103, 69.53527060154695505 ) ) ;
#30194 = CARTESIAN_POINT ( 'NONE',  ( -22.07022430586338402, -11.86582892075562157, 53.49999999999995026 ) ) ;
#30195 = AXIS2_PLACEMENT_3D ( 'NONE', #11181, #44930, #33068 ) ;
#30196 = ORIENTED_EDGE ( 'NONE', *, *, #2436, .F. ) ;
#30197 = CARTESIAN_POINT ( 'NONE',  ( -10.78898398081525301, -17.19290454168847404, 61.44271037915215317 ) ) ;
#30198 = CARTESIAN_POINT ( 'NONE',  ( -24.17899278864585355, -11.66673636667039027, 59.66731167108189737 ) ) ;
#30199 = B_SPLINE_CURVE_WITH_KNOTS ( 'NONE', 3,
 ( #17698, #40849, #3177, #32953, #17468, #36171, #22148, #32727, #47998, #18184 ),
 .UNSPECIFIED., .F., .F.,
 ( 4, 2, 2, 2, 4 ),
 ( 0.000000000000000000, 0.2500000000000000000, 0.5000000000000000000, 0.7500000000000000000, 1.000000000000000000 ),
 .UNSPECIFIED. ) ;
#30200 = DIRECTION ( 'NONE',  ( -3.071710424422018668E-17, 6.404604876783312462E-16, 1.000000000000000000 ) ) ;
#30201 = CARTESIAN_POINT ( 'NONE',  ( -24.32102769702319378, -16.00663948712615081, 66.06324977198688941 ) ) ;
#30202 = ORIENTED_EDGE ( 'NONE', *, *, #17839, .F. ) ;
#30203 = CARTESIAN_POINT ( 'NONE',  ( -10.53260261225980621, -17.63940775673892603, 68.19747689442833405 ) ) ;
#30204 = CARTESIAN_POINT ( 'NONE',  ( -17.14435614197124025, -7.364337588275183144, 70.61223108419747518 ) ) ;
#30205 = CARTESIAN_POINT ( 'NONE',  ( -12.59809028756154525, -19.87976139299041023, 64.88177373049498442 ) ) ;
#30206 = FACE_BOUND ( 'NONE', #43041, .T. ) ;
#30208 = ADVANCED_FACE ( 'NONE', ( #15470 ), #39230, .T. ) ;
#30207 = VERTEX_POINT ( 'NONE', #484 ) ;
#30209 = CARTESIAN_POINT ( 'NONE',  ( -13.16483405634261850, -20.92159860622343004, 58.24638845815591992 ) ) ;
#30210 = CARTESIAN_POINT ( 'NONE',  ( -10.83536383905390998, -17.31742040078651357, 64.62739380450889826 ) ) ;
#30211 = DIRECTION ( 'NONE',  ( 1.224646799147353207E-16, 1.000000000000000000, -1.912410701131276611E-32 ) ) ;
#30212 = EDGE_CURVE ( 'NONE', #37972, #5768, #9327, .T. ) ;
#30213 = CARTESIAN_POINT ( 'NONE',  ( -24.31823732957325745, -17.63313362019280106, 66.05861802595141796 ) ) ;
#30214 = ORIENTED_EDGE ( 'NONE', *, *, #11660, .F. ) ;
#30215 = DIRECTION ( 'NONE',  ( -3.071710424422018668E-17, 6.404604876783312462E-16, 1.000000000000000000 ) ) ;
#30216 = ORIENTED_EDGE ( 'NONE', *, *, #43381, .T. ) ;
#30217 = CARTESIAN_POINT ( 'NONE',  ( -10.29385348138020539, -12.64970417265235803, 64.38340698725603772 ) ) ;
#30218 = CARTESIAN_POINT ( 'NONE',  ( -16.97420703900234074, -7.769956100637374519, 70.69855872207435254 ) ) ;
#30219 = PLANE ( 'NONE',  #20403 ) ;
#30220 = ORIENTED_EDGE ( 'NONE', *, *, #23033, .F. ) ;
#30221 = DIRECTION ( 'NONE',  ( 0.000000000000000000, 0.000000000000000000, 1.000000000000000000 ) ) ;
#30222 = ORIENTED_EDGE ( 'NONE', *, *, #42471, .T. ) ;
#30223 = ORIENTED_EDGE ( 'NONE', *, *, #36652, .T. ) ;
#30224 = ORIENTED_EDGE ( 'NONE', *, *, #22639, .T. ) ;
#30225 = CARTESIAN_POINT ( 'NONE',  ( -15.32672178808326535, -21.95796145784420261, 72.30221390644346968 ) ) ;
#30226 = CARTESIAN_POINT ( 'NONE',  ( -20.57133303063786300, -8.056536552513840377, 67.03749994897439990 ) ) ;
#30227 = CARTESIAN_POINT ( 'NONE',  ( -19.39004244333994720, -21.99530814555272329, 58.68540713731352554 ) ) ;
#30228 = CARTESIAN_POINT ( 'NONE',  ( -14.33942418930512019, -10.56099362034968614, 52.02966884056656482 ) ) ;
#30229 = ADVANCED_FACE ( 'NONE', ( #42815 ), #35166, .T. ) ;
#30230 = CARTESIAN_POINT ( 'NONE',  ( -13.97628689860590079, -8.204186434626230096, 70.84302338899487950 ) ) ;
#30231 = DIRECTION ( 'NONE',  ( -5.731567514496413899E-31, -1.020425574103664789E-16, -1.000000000000000000 ) ) ;
#30232 = EDGE_CURVE ( 'NONE', #5757, #31902, #8979, .T. ) ;
#30233 = EDGE_LOOP ( 'NONE', ( #38575, #4344, #40370, #34331 ) ) ;
#30234 = ORIENTED_EDGE ( 'NONE', *, *, #20786, .F. ) ;
#30235 =( BOUNDED_SURFACE ( )  B_SPLINE_SURFACE ( 3, 1, ( 
 ( #41690, #4499 ),
 ( #42428, #37980 ),
 ( #34281, #20735 ),
 ( #24441, #6194 ),
 ( #35254, #47079 ),
 ( #27638, #35499 ),
 ( #24189, #13560 ) ),
 .UNSPECIFIED., .T., .F., .F. ) 
 B_SPLINE_SURFACE_WITH_KNOTS ( ( 4, 3, 4 ),
 ( 2, 2 ),
 ( 0.000000000000000000, 0.5000000000000000000, 1.000000000000000000 ),
 ( 0.000000000000000000, 1.000000000000000000 ),
 .UNSPECIFIED. ) 
 GEOMETRIC_REPRESENTATION_ITEM ( )  RATIONAL_B_SPLINE_SURFACE ( (
 ( 1.000000000000000000, 1.000000000000000000),
 ( 0.3333333333333335369, 0.3333333333333330373),
 ( 0.3333333333333335369, 0.3333333333333330373),
 ( 1.000000000000000000, 1.000000000000000000),
 ( 0.3333333333333333703, 0.3333333333333333703),
 ( 0.3333333333333333703, 0.3333333333333333703),
 ( 1.000000000000000000, 1.000000000000000000) ) ) 
 REPRESENTATION_ITEM ( '' )  SURFACE ( )  );
#30236 = CARTESIAN_POINT ( 'NONE',  ( -19.36683724782897897, -21.58655468785150688, 62.00975759738177118 ) ) ;
#30237 = EDGE_CURVE ( 'NONE', #26502, #3283, #31349, .T. ) ;
#30238 = EDGE_CURVE ( 'NONE', #5029, #24134, #42527, .T. ) ;
#30239 = VECTOR ( 'NONE', #17575, 1000.000000000000341 ) ;
#30240 = CARTESIAN_POINT ( 'NONE',  ( -13.90930827832509387, -8.240377080047705860, 74.39292945093751541 ) ) ;
#30241 = CARTESIAN_POINT ( 'NONE',  ( -10.05341976060008058, -15.89348643430029462, 64.65771587268669407 ) ) ;
#30242 = LINE ( 'NONE', #45261, #25245 ) ;
#30243 = ORIENTED_EDGE ( 'NONE', *, *, #38381, .F. ) ;
#30244 = CARTESIAN_POINT ( 'NONE',  ( -14.48034385650551847, -6.424090610841176385, 49.80797279389977916 ) ) ;
#30245 = EDGE_LOOP ( 'NONE', ( #13649, #29840, #27614, #2473, #17615 ) ) ;
#30246 = CARTESIAN_POINT ( 'NONE',  ( -9.993180735906239676, -14.27626192956519269, 64.53803862179867679 ) ) ;
#30247 = LINE ( 'NONE', #44293, #11151 ) ;
#30248 = DIRECTION ( 'NONE',  ( 0.5327540375067997269, 0.8462701315302331162, 7.203825861310633201E-08 ) ) ;
#30249 = ORIENTED_EDGE ( 'NONE', *, *, #24078, .T. ) ;
#30250 = CARTESIAN_POINT ( 'NONE',  ( -20.38868793477728403, -7.974332091099226361, 70.42913073863570617 ) ) ;
#30251 = B_SPLINE_CURVE_WITH_KNOTS ( 'NONE', 3,
 ( #17367, #32408, #41001, #29426, #22045, #48374, #18569, #33579, #7027, #37038 ),
 .UNSPECIFIED., .F., .F.,
 ( 4, 2, 2, 2, 4 ),
 ( 0.1272669073658565242, 0.2522669073463414957, 0.3772669073268264395, 0.5022669073073113832, 0.6272669072877963270 ),
 .UNSPECIFIED. ) ;
#30252 = DIRECTION ( 'NONE',  ( -3.071710424422018668E-17, 6.404604876783312462E-16, 1.000000000000000000 ) ) ;
#30253 = EDGE_CURVE ( 'NONE', #47529, #47620, #17166, .T. ) ;
#30254 = EDGE_LOOP ( 'NONE', ( #3417, #31417 ) ) ;
#30255 = CARTESIAN_POINT ( 'NONE',  ( -10.38618466708840415, -14.33732170831495978, 60.91821109628303788 ) ) ;
#30256 = CARTESIAN_POINT ( 'NONE',  ( -14.63795604342543655, -7.899797297607364044, 60.46996282252440835 ) ) ;
#30257 = DIRECTION ( 'NONE',  ( -0.3478314405900309603, -0.9375570856950864451, 0.000000000000000000 ) ) ;
#30258 = ORIENTED_EDGE ( 'NONE', *, *, #5232, .F. ) ;
#30259 = CARTESIAN_POINT ( 'NONE',  ( -24.69316504521514233, -16.44114857855330669, 59.32321200223080382 ) ) ;
#30260 = VERTEX_POINT ( 'NONE', #35883 ) ;
#30261 = VECTOR ( 'NONE', #10274, 1000.000000000000000 ) ;
#30262 = DIRECTION ( 'NONE',  ( 6.471065204144449778E-06, 1.909039588689591427E-06, -0.9999999999772404280 ) ) ;
#30263 = CYLINDRICAL_SURFACE ( 'NONE', #17782, 1.999999999999999556 ) ;
#30264 = VERTEX_POINT ( 'NONE', #24346 ) ;
#30265 = FACE_OUTER_BOUND ( 'NONE', #34701, .T. ) ;
#30266 = CARTESIAN_POINT ( 'NONE',  ( -24.06765785688162751, -12.42634649716644013, 69.92810001462744651 ) ) ;
#30267 = VECTOR ( 'NONE', #34914, 1000.000000000000000 ) ;
#30268 = CARTESIAN_POINT ( 'NONE',  ( -20.92409385541305511, -25.10920654474410441, 78.99999999999998579 ) ) ;
#30269 = ADVANCED_FACE ( 'NONE', ( #1691 ), #45859, .T. ) ;
#30270 = ORIENTED_EDGE ( 'NONE', *, *, #30788, .F. ) ;
#30271 = CARTESIAN_POINT ( 'NONE',  ( -21.42950876998643750, -20.55006782965317669, 72.59734371715153145 ) ) ;
#30272 = CARTESIAN_POINT ( 'NONE',  ( -16.34730751551633077, -7.892078375978933913, 60.48411973959233734 ) ) ;
#30273 = B_SPLINE_CURVE_WITH_KNOTS ( 'NONE', 3,
 ( #11716, #3850, #30445, #10987, #37300, #18858, #45459, #33866, #4102, #19101 ),
 .UNSPECIFIED., .F., .F.,
 ( 4, 2, 2, 2, 4 ),
 ( 0.1272669073657819172, 0.2522669073462828759, 0.3772669073267839179, 0.5022669073072848489, 0.6272669072877858909 ),
 .UNSPECIFIED. ) ;
#30274 = CARTESIAN_POINT ( 'NONE',  ( -21.76886496386750736, -13.05243499865791890, 52.02966884056656482 ) ) ;
#30275 = ORIENTED_EDGE ( 'NONE', *, *, #28089, .T. ) ;
#30276 = CARTESIAN_POINT ( 'NONE',  ( -19.09948850906665285, -8.012659424734943414, 63.73089235424028942 ) ) ;
#30277 = CARTESIAN_POINT ( 'NONE',  ( -21.73098984888145679, -8.730191469543168381, 70.31627926275058371 ) ) ;
#30278 = ORIENTED_EDGE ( 'NONE', *, *, #48546, .T. ) ;
#30279 = ORIENTED_EDGE ( 'NONE', *, *, #27193, .T. ) ;
#30280 = DIRECTION ( 'NONE',  ( -0.2573866790907600177, -0.9663084897829604669, -6.714855467380868574E-08 ) ) ;
#30281 = CARTESIAN_POINT ( 'NONE',  ( -15.02405691534179688, -8.340062653448301333, 47.99999999999994316 ) ) ;
#30282 = CYLINDRICAL_SURFACE ( 'NONE', #43788, 1.999999999999999112 ) ;
#30283 = EDGE_LOOP ( 'NONE', ( #32484, #6795, #9395, #17859 ) ) ;
#30284 = CARTESIAN_POINT ( 'NONE',  ( -21.90534385650552096, -8.801233750844183135, 48.81488406609782515 ) ) ;
#30285 = CARTESIAN_POINT ( 'NONE',  ( -12.45784128279547431, -19.74247851094704487, 61.41181112604091652 ) ) ;
#30286 = B_SPLINE_CURVE_WITH_KNOTS ( 'NONE', 3,
 ( #47809, #9679, #44151, #24695, #48052, #40419, #5966, #21708, #35993, #36691 ),
 .UNSPECIFIED., .F., .F.,
 ( 4, 2, 2, 2, 4 ),
 ( 0.6272669072877788965, 0.7522669073072940638, 0.8772669073268093420, 1.002266907346324398, 1.127266907365839677 ),
 .UNSPECIFIED. ) ;
#30287 = CARTESIAN_POINT ( 'NONE',  ( -12.15399301493812878, -9.543295845094297292, 57.20440096431307353 ) ) ;
#30288 = CARTESIAN_POINT ( 'NONE',  ( -22.58237342315448615, -13.83214364962418053, 52.02966884056656482 ) ) ;
#30289 = CARTESIAN_POINT ( 'NONE',  ( -13.02585106727260822, -13.15662797718154309, 49.52966884056655772 ) ) ;
#30290 = ORIENTED_EDGE ( 'NONE', *, *, #11053, .T. ) ;
#30291 = CYLINDRICAL_SURFACE ( 'NONE', #44658, 2.000000000000001332 ) ;
#30292 = EDGE_CURVE ( 'NONE', #17919, #44193, #47369, .T. ) ;
#30293 = EDGE_CURVE ( 'NONE', #20123, #48485, #32611, .T. ) ;
#30294 = B_SPLINE_CURVE_WITH_KNOTS ( 'NONE', 1,
 ( #47528, #20701 ),
 .UNSPECIFIED., .F., .F.,
 ( 2, 2 ),
 ( 0.000000000000000000, 1.000000000000000000 ),
 .UNSPECIFIED. ) ;
#30295 = CYLINDRICAL_SURFACE ( 'NONE', #20158, 2.000000000000001332 ) ;
#30296 = DIRECTION ( 'NONE',  ( 0.9687793358424821033, -0.2479245821708679909, 0.000000000000000000 ) ) ;
#30297 = VERTEX_POINT ( 'NONE', #37029 ) ;
#30298 = VECTOR ( 'NONE', #3741, 1000.000000000000114 ) ;
#30299 = EDGE_CURVE ( 'NONE', #15104, #26867, #17191, .T. ) ;
#30300 = EDGE_CURVE ( 'NONE', #32895, #32695, #22482, .T. ) ;
#30301 = ORIENTED_EDGE ( 'NONE', *, *, #3362, .F. ) ;
#30302 = CARTESIAN_POINT ( 'NONE',  ( -19.89748337530321365, -21.35767964923046236, 68.98863364564390110 ) ) ;
#30303 = AXIS2_PLACEMENT_3D ( 'NONE', #16975, #12817, #12579 ) ;
#30304 = CARTESIAN_POINT ( 'NONE',  ( -17.01596769717176372, -7.370308014455987156, 74.07522855441366971 ) ) ;
#30305 = CARTESIAN_POINT ( 'NONE',  ( -13.31969252371020929, -21.02664138888986756, 61.71657530956684212 ) ) ;
#30306 = FACE_OUTER_BOUND ( 'NONE', #4284, .T. ) ;
#30307 =( BOUNDED_CURVE ( )  B_SPLINE_CURVE ( 3, ( #3361, #7559, #7321, #647 ),
 .UNSPECIFIED., .F., .F. ) 
 B_SPLINE_CURVE_WITH_KNOTS ( ( 4, 4 ),
 ( 0.4074455897393696735, 0.5000000000000000000 ),
 .UNSPECIFIED. ) 
 CURVE ( )  GEOMETRIC_REPRESENTATION_ITEM ( )  RATIONAL_B_SPLINE_CURVE ( ( 0.6983129098261152690, 0.7760317562607143005, 0.8765941196520082856, 0.9999999999999950040 ) ) 
 REPRESENTATION_ITEM ( '' )  );
#30308 = EDGE_LOOP ( 'NONE', ( #22953, #42728, #44766, #9201, #43725 ) ) ;
#30309 = CARTESIAN_POINT ( 'NONE',  ( -13.53325622885376944, -21.16256470055228789, 65.17124264509627096 ) ) ;
#30310 = DIRECTION ( 'NONE',  ( 3.071710424422018668E-17, -6.404604876783312462E-16, -1.000000000000000000 ) ) ;
#30311 = EDGE_CURVE ( 'NONE', #40297, #16415, #26117, .T. ) ;
#30312 = ORIENTED_EDGE ( 'NONE', *, *, #39279, .F. ) ;
#30313 = CARTESIAN_POINT ( 'NONE',  ( -10.37871274698333046, -17.23124524545501046, 61.41389037703014964 ) ) ;
#30314 = CARTESIAN_POINT ( 'NONE',  ( -11.10300763040008398, -10.86615618544839457, 57.39398486019972268 ) ) ;
#30315 = CARTESIAN_POINT ( 'NONE',  ( -50.42609385541305755, -14.80920654474426534, 72.98823529411762934 ) ) ;
#30316 =( BOUNDED_SURFACE ( )  B_SPLINE_SURFACE ( 3, 1, ( 
 ( #10096, #25119 ),
 ( #12814, #16502 ),
 ( #5691, #9630 ),
 ( #9859, #35938 ),
 ( #24646, #2213 ),
 ( #35690, #24874 ),
 ( #29046, #40139 ) ),
 .UNSPECIFIED., .T., .F., .F. ) 
 B_SPLINE_SURFACE_WITH_KNOTS ( ( 4, 3, 4 ),
 ( 2, 2 ),
 ( 0.000000000000000000, 0.5000000000000000000, 1.000000000000000000 ),
 ( 0.000000000000000000, 1.000000000000000000 ),
 .UNSPECIFIED. ) 
 GEOMETRIC_REPRESENTATION_ITEM ( )  RATIONAL_B_SPLINE_SURFACE ( (
 ( 1.000000000000000000, 1.000000000000000000),
 ( 0.3333333333333335369, 0.3333333333333330373),
 ( 0.3333333333333335369, 0.3333333333333330373),
 ( 1.000000000000000000, 1.000000000000000000),
 ( 0.3333333333333333703, 0.3333333333333333703),
 ( 0.3333333333333333703, 0.3333333333333333703),
 ( 1.000000000000000000, 1.000000000000000000) ) ) 
 REPRESENTATION_ITEM ( '' )  SURFACE ( )  );
#30317 = ORIENTED_EDGE ( 'NONE', *, *, #7685, .T. ) ;
#30318 =( BOUNDED_CURVE ( )  B_SPLINE_CURVE ( 3, ( #2043, #17041, #6230, #32090 ),
 .UNSPECIFIED., .F., .F. ) 
 B_SPLINE_CURVE_WITH_KNOTS ( ( 4, 4 ),
 ( 0.9074455897393708392, 1.000000000000000000 ),
 .UNSPECIFIED. ) 
 CURVE ( )  GEOMETRIC_REPRESENTATION_ITEM ( )  RATIONAL_B_SPLINE_CURVE ( ( 0.6983129098261174894, 0.7760317562607192965, 0.8765941196520135037, 1.000000000000000000 ) ) 
 REPRESENTATION_ITEM ( '' )  );
#30319 = CARTESIAN_POINT ( 'NONE',  ( -41.67850562011894056, -14.80920654474422271, 68.96470588235293064 ) ) ;
#30320 = ORIENTED_EDGE ( 'NONE', *, *, #47944, .T. ) ;
#30321 = CARTESIAN_POINT ( 'NONE',  ( -22.28538024775887294, -19.92612572838908491, 72.78833238834644703 ) ) ;
#30322 = LINE ( 'NONE', #42116, #48614 ) ;
#30323 = ORIENTED_EDGE ( 'NONE', *, *, #43485, .F. ) ;
#30324 = CARTESIAN_POINT ( 'NONE',  ( -13.65684165595416921, -8.849801312179289781, 56.98439896120441261 ) ) ;
#30325 = PLANE ( 'NONE',  #28936 ) ;
#30326 = CARTESIAN_POINT ( 'NONE',  ( -21.03659385650551528, -6.915538690918074494, 49.31353937987644542 ) ) ;
#30327 = CARTESIAN_POINT ( 'NONE',  ( -10.78967749848787427, -12.41559940729129785, 61.21342246320382685 ) ) ;
#30328 = CARTESIAN_POINT ( 'NONE',  ( -10.63109664364847440, -11.75017249117723317, 74.70840197822751350 ) ) ;
#30329 = DIRECTION ( 'NONE',  ( -0.000000000000000000, -1.000000000000000000, -0.000000000000000000 ) ) ;
#30330 = CARTESIAN_POINT ( 'NONE',  ( -45.92409385541306222, -14.80920654474410902, 70.50000000000000000 ) ) ;
#30331 = VERTEX_POINT ( 'NONE', #33832 ) ;
#30332 = DIRECTION ( 'NONE',  ( -1.149299189161336899E-05, 1.849289878362067349E-06, -0.9999999999322456423 ) ) ;
#30333 =( BOUNDED_SURFACE ( )  B_SPLINE_SURFACE ( 3, 1, ( 
 ( #38107, #45283 ),
 ( #19402, #15204 ),
 ( #34406, #38601 ),
 ( #4885, #11530 ),
 ( #41575, #45774 ),
 ( #1167, #38341 ),
 ( #31213, #7858 ) ),
 .UNSPECIFIED., .T., .F., .F. ) 
 B_SPLINE_SURFACE_WITH_KNOTS ( ( 4, 3, 4 ),
 ( 2, 2 ),
 ( 0.000000000000000000, 0.5000000000000000000, 1.000000000000000000 ),
 ( 0.000000000000000000, 1.000000000000000000 ),
 .UNSPECIFIED. ) 
 GEOMETRIC_REPRESENTATION_ITEM ( )  RATIONAL_B_SPLINE_SURFACE ( (
 ( 1.000000000000000000, 1.000000000000000000),
 ( 0.3333333333333335369, 0.3333333333333330373),
 ( 0.3333333333333335369, 0.3333333333333330373),
 ( 1.000000000000000000, 1.000000000000000000),
 ( 0.3333333333333333703, 0.3333333333333333703),
 ( 0.3333333333333333703, 0.3333333333333333703),
 ( 1.000000000000000000, 1.000000000000000000) ) ) 
 REPRESENTATION_ITEM ( '' )  SURFACE ( )  );
#30334 = CARTESIAN_POINT ( 'NONE',  ( -13.24203256135214346, -20.97556893053616989, 58.15994682967826179 ) ) ;
#30335 = CIRCLE ( 'NONE', #15356, 2.000000000000001776 ) ;
#30336 = B_SPLINE_CURVE_WITH_KNOTS ( 'NONE', 1,
 ( #11782, #18920 ),
 .UNSPECIFIED., .F., .F.,
 ( 2, 2 ),
 ( 0.000000000000000000, 1.000000000000000000 ),
 .UNSPECIFIED. ) ;
#30337 = CARTESIAN_POINT ( 'NONE',  ( -11.89179040387956832, -10.43929601004734486, 70.96893105543333036 ) ) ;
#30338 = DIRECTION ( 'NONE',  ( -0.1738928961406289164, 0.9847645711904029486, 7.871847295470929299E-08 ) ) ;
#30339 = CARTESIAN_POINT ( 'NONE',  ( -22.79478857039302042, -9.645877667282650947, 73.60348353842616120 ) ) ;
#30340 = ORIENTED_EDGE ( 'NONE', *, *, #16268, .T. ) ;
#30341 = ORIENTED_EDGE ( 'NONE', *, *, #18126, .F. ) ;
#30342 = CARTESIAN_POINT ( 'NONE',  ( -21.46132321166677315, -9.088779937831205302, 73.79055940392021284 ) ) ;
#30343 = CARTESIAN_POINT ( 'NONE',  ( -14.67111461712440601, -7.886426496449994161, 60.43500955848998757 ) ) ;
#30344 = ORIENTED_EDGE ( 'NONE', *, *, #28419, .T. ) ;
#30345 = CARTESIAN_POINT ( 'NONE',  ( -10.01391823204708231, -15.58571177677185915, 57.68137499724732464 ) ) ;
#30346 = FACE_OUTER_BOUND ( 'NONE', #23197, .T. ) ;
#30347 = CARTESIAN_POINT ( 'NONE',  ( -12.55420361774382698, -9.778633124847853964, 57.27862503956445295 ) ) ;
#30348 = DIRECTION ( 'NONE',  ( -9.637352644315596475E-17, 0.000000000000000000, -1.000000000000000000 ) ) ;
#30349 = CARTESIAN_POINT ( 'NONE',  ( -24.39228817134714689, -14.13808901473641377, 73.40654960426921605 ) ) ;
#30350 = CARTESIAN_POINT ( 'NONE',  ( -23.59429156608431200, -18.98457121427007976, 65.98422751227842298 ) ) ;
#30351 = FACE_OUTER_BOUND ( 'NONE', #19513, .T. ) ;
#30352 = CARTESIAN_POINT ( 'NONE',  ( -24.39634131874377587, -15.43191468712751302, 73.11189705367094405 ) ) ;
#30353 = EDGE_CURVE ( 'NONE', #3366, #18637, #29248, .T. ) ;
#30354 = CARTESIAN_POINT ( 'NONE',  ( -24.10946622006557760, -11.52159296043784309, 63.15229477024898586 ) ) ;
#30355 = CARTESIAN_POINT ( 'NONE',  ( -19.59054105953293856, -21.52187752522791442, 69.02662522961304603 ) ) ;
#30356 = CARTESIAN_POINT ( 'NONE',  ( -11.35719102664687874, -18.40077844947705188, 58.09242476654641507 ) ) ;
#30357 = CARTESIAN_POINT ( 'NONE',  ( -50.42609385541305755, -14.90920654474422236, 68.96470588235293064 ) ) ;
#30358 = DIRECTION ( 'NONE',  ( -2.866981220435666553E-17, 1.000000000000000000, 1.190614954331866791E-16 ) ) ;
#30359 = ORIENTED_EDGE ( 'NONE', *, *, #38038, .T. ) ;
#30360 = ORIENTED_EDGE ( 'NONE', *, *, #32394, .F. ) ;
#30361 = PLANE ( 'NONE',  #15527 ) ;
#30362 = EDGE_CURVE ( 'NONE', #2842, #1538, #13652, .T. ) ;
#30363 = VERTEX_POINT ( 'NONE', #30660 ) ;
#30364 = CARTESIAN_POINT ( 'NONE',  ( -23.14284385541300182, -7.587656875400161205, 49.25157356644805873 ) ) ;
#30365 = EDGE_CURVE ( 'NONE', #16073, #16677, #14853, .T. ) ;
#30366 = DIRECTION ( 'NONE',  ( -3.071710424422018668E-17, 6.404604876783312462E-16, 1.000000000000000000 ) ) ;
#30367 = ADVANCED_FACE ( 'NONE', ( #41724 ), #11204, .T. ) ;
#30368 = CONICAL_SURFACE ( 'NONE', #25621, 3077.683537175336824, 1.256637061435925240 ) ;
#30369 = CARTESIAN_POINT ( 'NONE',  ( -13.39714536113074139, -8.541322072920136677, 57.06993516337580274 ) ) ;
#30370 = LINE ( 'NONE', #38456, #47442 ) ;
#30371 = VERTEX_POINT ( 'NONE', #44951 ) ;
#30372 = DIRECTION ( 'NONE',  ( 8.563106566420985232E-06, -6.519503004583679708E-06, 0.9999999999420846608 ) ) ;
#30373 = CARTESIAN_POINT ( 'NONE',  ( -18.80072161947576603, -7.487499411268177418, 70.52068027036284548 ) ) ;
#30374 = EDGE_LOOP ( 'NONE', ( #14547, #7013, #10659, #21165 ) ) ;
#30375 = CARTESIAN_POINT ( 'NONE',  ( -18.78659385759798894, -7.222650657624104298, 49.61879703869476543 ) ) ;
#30376 = CARTESIAN_POINT ( 'NONE',  ( -23.93808071853957031, -17.37550477255097903, 69.48509980817377141 ) ) ;
#30377 = EDGE_LOOP ( 'NONE', ( #41814, #20072, #46338, #12906, #7511 ) ) ;
#30378 = CYLINDRICAL_SURFACE ( 'NONE', #35443, 4.686499999999997002 ) ;
#30379 = CARTESIAN_POINT ( 'NONE',  ( -17.42409385541299471, -14.80920654474435771, 49.52966884056655772 ) ) ;
#30380 = CARTESIAN_POINT ( 'NONE',  ( -12.56172001024846452, -20.45377019276184427, 71.99149100736865137 ) ) ;
#30381 = ORIENTED_EDGE ( 'NONE', *, *, #12122, .T. ) ;
#30382 = CARTESIAN_POINT ( 'NONE',  ( -10.73229864388703625, -12.57879810080903482, 64.56836243396730879 ) ) ;
#30383 = CARTESIAN_POINT ( 'NONE',  ( -10.28365401573067039, -12.68397276782584449, 64.41836109611280392 ) ) ;
#30384 = CARTESIAN_POINT ( 'NONE',  ( -11.55100916664023103, -10.22540270530303275, 71.14609986067189595 ) ) ;
#30385 = DIRECTION ( 'NONE',  ( -3.071710424422018668E-17, 6.404604876783312462E-16, 1.000000000000000000 ) ) ;
#30386 = ORIENTED_EDGE ( 'NONE', *, *, #11905, .F. ) ;
#30387 = CARTESIAN_POINT ( 'NONE',  ( -24.25510706449861686, -16.56479617024167084, 59.53821300994621168 ) ) ;
#30388 = DIRECTION ( 'NONE',  ( -0.6562885720885138774, 0.7545099801500438907, 1.193821363054685294E-08 ) ) ;
#30389 = FACE_OUTER_BOUND ( 'NONE', #2929, .T. ) ;
#30390 = CARTESIAN_POINT ( 'NONE',  ( -23.45651108574825372, -18.46362474097727002, 69.17883092557275404 ) ) ;
#30391 = FACE_OUTER_BOUND ( 'NONE', #46986, .T. ) ;
#30392 = CARTESIAN_POINT ( 'NONE',  ( -10.90759852523040507, -17.49952041063523822, 68.09721944423129969 ) ) ;
#30393 = CARTESIAN_POINT ( 'NONE',  ( -19.99284385650551599, -7.406986770994972602, 48.81910596585309747 ) ) ;
#30394 = EDGE_LOOP ( 'NONE', ( #21659, #18213 ) ) ;
#30395 = CARTESIAN_POINT ( 'NONE',  ( -24.63355139826557760, -12.92841318297298692, 62.94608782021682458 ) ) ;
#30396 = CARTESIAN_POINT ( 'NONE',  ( -21.14909385759798965, -8.112991634885936776, 51.74999426922421719 ) ) ;
#30397 = ORIENTED_EDGE ( 'NONE', *, *, #39745, .F. ) ;
#30398 = CARTESIAN_POINT ( 'NONE',  ( -15.10382451463400955, -18.89477942154363888, 49.52966884056656482 ) ) ;
#30399 = CARTESIAN_POINT ( 'NONE',  ( -21.54284385759798681, -7.587656875400192291, 49.25157356644813689 ) ) ;
#30400 = CARTESIAN_POINT ( 'NONE',  ( -10.40181215838624240, -12.32098906055858478, 57.37211424251319158 ) ) ;
#30401 = ADVANCED_FACE ( 'NONE', ( #3557 ), #45678, .T. ) ;
#30402 = ORIENTED_EDGE ( 'NONE', *, *, #3955, .F. ) ;
#30403 = B_SPLINE_CURVE_WITH_KNOTS ( 'NONE', 3,
 ( #21479, #40652, #33008, #32780, #13809, #6210, #47576, #44862, #17749, #6690 ),
 .UNSPECIFIED., .F., .F.,
 ( 4, 2, 2, 2, 4 ),
 ( 0.6272669072977357096, 0.7522669073147704166, 0.8772669073318051236, 1.002266907348839720, 1.127266907365874538 ),
 .UNSPECIFIED. ) ;
#30404 = CARTESIAN_POINT ( 'NONE',  ( -18.51768661843271602, -21.77690966467453393, 68.70025907080108141 ) ) ;
#30405 = AXIS2_PLACEMENT_3D ( 'NONE', #2911, #228, #41322 ) ;
#30406 = AXIS2_PLACEMENT_3D ( 'NONE', #11030, #13959, #41069 ) ;
#30407 = CARTESIAN_POINT ( 'NONE',  ( -18.39099673902470045, -22.19624494031300088, 68.92176384159974134 ) ) ;
#30408 = B_SPLINE_CURVE_WITH_KNOTS ( 'NONE', 1,
 ( #42957, #46168 ),
 .UNSPECIFIED., .F., .F.,
 ( 2, 2 ),
 ( 0.000000000000000000, 1.000000000000000000 ),
 .UNSPECIFIED. ) ;
#30409 = ORIENTED_EDGE ( 'NONE', *, *, #36438, .T. ) ;
#30410 = CARTESIAN_POINT ( 'NONE',  ( -13.41159385650551528, -6.922745924619793101, 51.69366785382590024 ) ) ;
#30411 =( BOUNDED_SURFACE ( )  B_SPLINE_SURFACE ( 3, 1, ( 
 ( #35452, #27589 ),
 ( #46315, #20694 ),
 ( #5684, #8889 ),
 ( #43351, #35684 ),
 ( #31770, #1737 ),
 ( #12324, #24145 ),
 ( #39401, #28066 ) ),
 .UNSPECIFIED., .T., .F., .F. ) 
 B_SPLINE_SURFACE_WITH_KNOTS ( ( 4, 3, 4 ),
 ( 2, 2 ),
 ( 0.000000000000000000, 0.5000000000000000000, 1.000000000000000000 ),
 ( 0.000000000000000000, 1.000000000000000000 ),
 .UNSPECIFIED. ) 
 GEOMETRIC_REPRESENTATION_ITEM ( )  RATIONAL_B_SPLINE_SURFACE ( (
 ( 1.000000000000000000, 1.000000000000000000),
 ( 0.3333333333333335369, 0.3333333333333330373),
 ( 0.3333333333333335369, 0.3333333333333330373),
 ( 1.000000000000000000, 1.000000000000000000),
 ( 0.3333333333333333703, 0.3333333333333333703),
 ( 0.3333333333333333703, 0.3333333333333333703),
 ( 1.000000000000000000, 1.000000000000000000) ) ) 
 REPRESENTATION_ITEM ( '' )  SURFACE ( )  );
#30412 = DIRECTION ( 'NONE',  ( -3.071710424422018668E-17, 6.404604876783312462E-16, 1.000000000000000000 ) ) ;
#30413 = FACE_OUTER_BOUND ( 'NONE', #33180, .T. ) ;
#30414 = CARTESIAN_POINT ( 'NONE',  ( -21.75868347184070473, -16.62218431696164345, 52.02966884056656482 ) ) ;
#30415 = CARTESIAN_POINT ( 'NONE',  ( -17.42409385541299471, -14.80920654474435594, 52.02966884056656482 ) ) ;
#30416 = VERTEX_POINT ( 'NONE', #4070 ) ;
#30417 = ORIENTED_EDGE ( 'NONE', *, *, #11564, .F. ) ;
#30418 = CARTESIAN_POINT ( 'NONE',  ( -13.22466815457524447, -9.790356681133982164, 49.88235584379216192 ) ) ;
#30419 = EDGE_CURVE ( 'NONE', #27633, #35167, #19067, .T. ) ;
#30420 = CARTESIAN_POINT ( 'NONE',  ( -17.42409385541299471, -14.80920654474434883, 62.02966884056656482 ) ) ;
#30421 = CARTESIAN_POINT ( 'NONE',  ( -19.61601346313181082, -21.50980264518277707, 65.46486213821818012 ) ) ;
#30422 = ADVANCED_FACE ( 'NONE', ( #33570 ), #22520, .T. ) ;
#30423 = CARTESIAN_POINT ( 'NONE',  ( -14.34284385650551563, -8.811426318492348031, 52.18089403414752070 ) ) ;
#30424 = B_SPLINE_CURVE_WITH_KNOTS ( 'NONE', 3,
 ( #5500, #17183, #3150, #24844, #18157, #35900, #2180, #36863, #47725, #36385 ),
 .UNSPECIFIED., .F., .F.,
 ( 4, 2, 2, 2, 4 ),
 ( 0.6272669072878305219, 0.7522669073073273704, 0.8772669073268243300, 1.002266907346321290, 1.127266907365818138 ),
 .UNSPECIFIED. ) ;
#30425 = EDGE_CURVE ( 'NONE', #43774, #35420, #48366, .T. ) ;
#30426 = CARTESIAN_POINT ( 'NONE',  ( -21.12516169987187098, -20.80993955427394582, 69.06922321213187388 ) ) ;
#30427 = CARTESIAN_POINT ( 'NONE',  ( -10.59656512619885227, -13.05092609425065220, 68.02360230423869325 ) ) ;
#30428 = CARTESIAN_POINT ( 'NONE',  ( -18.90996118681096405, -7.968724231816139536, 67.20071784163268092 ) ) ;
#30429 = DIRECTION ( 'NONE',  ( -0.8459089628457130416, -0.5333273165489313961, 7.771812504399801304E-08 ) ) ;
#30430 = ADVANCED_FACE ( 'NONE', ( #30413 ), #19837, .T. ) ;
#30431 = VERTEX_POINT ( 'NONE', #38012 ) ;
#30432 = DIRECTION ( 'NONE',  ( 0.000000000000000000, 0.000000000000000000, 1.000000000000000000 ) ) ;
#30433 = AXIS2_PLACEMENT_3D ( 'NONE', #24180, #46597, #20233 ) ;
#30434 = CIRCLE ( 'NONE', #46166, 0.2499999999999976408 ) ;
#30435 = ORIENTED_EDGE ( 'NONE', *, *, #23584, .F. ) ;
#30436 = CARTESIAN_POINT ( 'NONE',  ( -20.22859725435685618, -8.395501029963087447, 67.00777471169989497 ) ) ;
#30437 = CARTESIAN_POINT ( 'NONE',  ( -12.51505295934874518, -9.205071670917405413, 74.47956342064293267 ) ) ;
#30438 = CARTESIAN_POINT ( 'NONE',  ( -24.27033112822875438, -13.12649005559073068, 63.13264177271826583 ) ) ;
#30439 = EDGE_LOOP ( 'NONE', ( #4768, #35357, #28836, #6639 ) ) ;
#30440 = CARTESIAN_POINT ( 'NONE',  ( -18.12717186014929283, -21.82707771419581633, 61.76047256604253732 ) ) ;
#30441 = CARTESIAN_POINT ( 'NONE',  ( -14.67759629421408718, -7.883812837594224021, 60.49809014262143592 ) ) ;
#30442 = VECTOR ( 'NONE', #46712, 1000.000000000000000 ) ;
#30443 = CARTESIAN_POINT ( 'NONE',  ( -19.39738106961548425, -7.625280727630859623, 60.06069365028482565 ) ) ;
#30444 = ORIENTED_EDGE ( 'NONE', *, *, #4998, .F. ) ;
#30445 = CARTESIAN_POINT ( 'NONE',  ( -19.49467501587391638, -21.96586113430295484, 62.13470298284286031 ) ) ;
#30446 = CARTESIAN_POINT ( 'NONE',  ( -20.81921389985186721, -21.44071754855728784, 58.75979745677555854 ) ) ;
#30447 = DIRECTION ( 'NONE',  ( -3.071710424422018668E-17, 6.404604876783312462E-16, 1.000000000000000000 ) ) ;
#30448 = FACE_BOUND ( 'NONE', #36338, .T. ) ;
#30449 = VERTEX_POINT ( 'NONE', #22276 ) ;
#30450 = CARTESIAN_POINT ( 'NONE',  ( -18.08967161758600994, -21.83134672834333045, 68.90694883545079108 ) ) ;
#30451 = LINE ( 'NONE', #8055, #42839 ) ;
#30452 = CARTESIAN_POINT ( 'NONE',  ( -24.16575376147897813, -12.74704232990201547, 69.77243002240838621 ) ) ;
#30453 = CARTESIAN_POINT ( 'NONE',  ( -21.53550107051403018, -9.078485192726875042, 74.01617645989524874 ) ) ;
#30454 = ORIENTED_EDGE ( 'NONE', *, *, #19366, .T. ) ;
#30455 = CARTESIAN_POINT ( 'NONE',  ( -22.66727051383977809, -10.09628829486277546, 70.31178520457007153 ) ) ;
#30456 = ORIENTED_EDGE ( 'NONE', *, *, #30963, .T. ) ;
#30457 = CARTESIAN_POINT ( 'NONE',  ( -19.86569447268031041, -19.73755174630646891, 53.49999999999995026 ) ) ;
#30458 = LINE ( 'NONE', #11734, #28278 ) ;
#30459 =( BOUNDED_CURVE ( )  B_SPLINE_CURVE ( 3, ( #6377, #35911, #21637, #21407 ),
 .UNSPECIFIED., .F., .F. ) 
 B_SPLINE_CURVE_WITH_KNOTS ( ( 4, 4 ),
 ( 0.5000000000000000000, 0.9074455897393683967 ),
 .UNSPECIFIED. ) 
 CURVE ( )  GEOMETRIC_REPRESENTATION_ITEM ( )  RATIONAL_B_SPLINE_CURVE ( ( 1.000000000000004663, 0.4567392136813338555, 0.3561768502900276023, 0.6983129098260909551 ) ) 
 REPRESENTATION_ITEM ( '' )  );
#30460 = EDGE_CURVE ( 'NONE', #8065, #1168, #8843, .T. ) ;
#30461 = CARTESIAN_POINT ( 'NONE',  ( -13.91686280105865947, -8.236299372188803147, 74.31459218752463869 ) ) ;
#30462 = VERTEX_POINT ( 'NONE', #42708 ) ;
#30463 = B_SPLINE_CURVE_WITH_KNOTS ( 'NONE', 3,
 ( #23721, #42899, #20242, #38711, #31813, #39193, #5481, #35249, #1527, #16533 ),
 .UNSPECIFIED., .F., .F.,
 ( 4, 2, 2, 2, 4 ),
 ( 0.6272669072976988502, 0.7522669073147150165, 0.8772669073317311828, 1.002266907348747349, 1.127266907365763515 ),
 .UNSPECIFIED. ) ;
#30464 = CARTESIAN_POINT ( 'NONE',  ( -13.17364477763805652, -9.395196358873663556, 49.41429196092195042 ) ) ;
#30465 = EDGE_LOOP ( 'NONE', ( #15174, #1241, #31877, #3286 ) ) ;
#30466 = ORIENTED_EDGE ( 'NONE', *, *, #7328, .T. ) ;
#30467 = ORIENTED_EDGE ( 'NONE', *, *, #89, .F. ) ;
#30468 = DIRECTION ( 'NONE',  ( 1.415640159446835064E-31, -4.937737817590986075E-15, 1.000000000000000000 ) ) ;
#30469 = CARTESIAN_POINT ( 'NONE',  ( -24.72409385541305582, -14.80920654474426357, 72.08823529411763786 ) ) ;
#30470 = CARTESIAN_POINT ( 'NONE',  ( -21.26695983349702246, -20.66012254167596041, 69.12738141313978701 ) ) ;
#30471 = DIRECTION ( 'NONE',  ( -4.436160455182634911E-06, -7.761523761658527715E-06, 0.9999999999600395206 ) ) ;
#30472 = DIRECTION ( 'NONE',  ( 0.8705373987491421550, -0.4921022631314296847, 4.758021987246392719E-08 ) ) ;
#30473 = CARTESIAN_POINT ( 'NONE',  ( -19.20714268997449281, -19.15619313305651161, 49.52966884056656482 ) ) ;
#30474 = ADVANCED_FACE ( 'NONE', ( #35292 ), #46395, .T. ) ;
#30475 = CARTESIAN_POINT ( 'NONE',  ( -19.43397188950632781, -8.102277950761333614, 60.15020107494644463 ) ) ;
#30476 =( BOUNDED_SURFACE ( )  B_SPLINE_SURFACE ( 3, 1, ( 
 ( #16366, #8508 ),
 ( #27462, #883 ),
 ( #4568, #23785 ),
 ( #26746, #19591 ),
 ( #401, #12685 ),
 ( #12201, #20075 ),
 ( #11719, #34599 ) ),
 .UNSPECIFIED., .T., .F., .F. ) 
 B_SPLINE_SURFACE_WITH_KNOTS ( ( 4, 3, 4 ),
 ( 2, 2 ),
 ( 0.000000000000000000, 0.5000000000000000000, 1.000000000000000000 ),
 ( 0.000000000000000000, 1.000000000000000000 ),
 .UNSPECIFIED. ) 
 GEOMETRIC_REPRESENTATION_ITEM ( )  RATIONAL_B_SPLINE_SURFACE ( (
 ( 1.000000000000000000, 1.000000000000000000),
 ( 0.3333333333333335369, 0.3333333333333330373),
 ( 0.3333333333333335369, 0.3333333333333330373),
 ( 1.000000000000000000, 1.000000000000000000),
 ( 0.3333333333333333703, 0.3333333333333333703),
 ( 0.3333333333333333703, 0.3333333333333333703),
 ( 1.000000000000000000, 1.000000000000000000) ) ) 
 REPRESENTATION_ITEM ( '' )  SURFACE ( )  );
#30477 = VECTOR ( 'NONE', #20823, 1000.000000000000114 ) ;
#30478 = VECTOR ( 'NONE', #4153, 1000.000000000000114 ) ;
#30479 = VERTEX_POINT ( 'NONE', #42460 ) ;
#30480 = ORIENTED_EDGE ( 'NONE', *, *, #20532, .T. ) ;
#30481 = CARTESIAN_POINT ( 'NONE',  ( -16.09168231696496676, -7.478562553351938647, 60.31373090009974902 ) ) ;
#30482 = EDGE_CURVE ( 'NONE', #17825, #21318, #23990, .T. ) ;
#30483 = CARTESIAN_POINT ( 'NONE',  ( -9.995738364564658696, -14.24060042610175358, 64.50308557176904856 ) ) ;
#30484 = CARTESIAN_POINT ( 'NONE',  ( -10.50393342808087560, -15.87404512457899664, 68.08841022104337526 ) ) ;
#30485 = AXIS2_PLACEMENT_3D ( 'NONE', #38152, #38394, #42843 ) ;
#30486 = CARTESIAN_POINT ( 'NONE',  ( -23.73810165963432084, -18.76483127932742789, 69.40716580542252245 ) ) ;
#30487 = VERTEX_POINT ( 'NONE', #8474 ) ;
#30488 = CARTESIAN_POINT ( 'NONE',  ( -14.36784385650551954, -6.428312510596451368, 51.20221977374900035 ) ) ;
#30489 = VERTEX_POINT ( 'NONE', #12887 ) ;
#30490 = EDGE_CURVE ( 'NONE', #5443, #19021, #37627, .T. ) ;
#30491 = CARTESIAN_POINT ( 'NONE',  ( -11.62161759534551919, -18.81995649556354877, 71.98686160459075722 ) ) ;
#30492 = CARTESIAN_POINT ( 'NONE',  ( -19.04853579327176760, -7.948602568230340282, 63.71617106789811658 ) ) ;
#30493 = CARTESIAN_POINT ( 'NONE',  ( -15.29809733969474195, -21.47854975192407778, 68.87592918283094434 ) ) ;
#30494 = EDGE_CURVE ( 'NONE', #36010, #486, #26952, .T. ) ;
#30495 = VERTEX_POINT ( 'NONE', #16814 ) ;
#30496 = CARTESIAN_POINT ( 'NONE',  ( -17.42409385541299471, -14.80920654474434883, 62.02966884056656482 ) ) ;
#30497 = DIRECTION ( 'NONE',  ( 3.071710424422018668E-17, -6.404604876783312462E-16, -1.000000000000000000 ) ) ;
#30498 = CARTESIAN_POINT ( 'NONE',  ( -12.36756753426621813, -9.896138138887707214, 57.37463480816234096 ) ) ;
#30499 = EDGE_LOOP ( 'NONE', ( #18862, #7325 ) ) ;
#30500 = CARTESIAN_POINT ( 'NONE',  ( -8.424093855413063991, -15.80920654474410725, 48.99999999999997868 ) ) ;
#30501 = EDGE_CURVE ( 'NONE', #43447, #22665, #20287, .T. ) ;
#30502 = DIRECTION ( 'NONE',  ( -3.071710424422018668E-17, 6.404604876783312462E-16, 1.000000000000000000 ) ) ;
#30503 = CARTESIAN_POINT ( 'NONE',  ( -23.83512934130040861, -17.76108582422602922, 66.08789927488301430 ) ) ;
#30504 = ORIENTED_EDGE ( 'NONE', *, *, #11058, .F. ) ;
#30505 = DIRECTION ( 'NONE',  ( -0.9862050927915950727, -0.1655279884246635413, -7.765682857010803534E-08 ) ) ;
#30506 = EDGE_CURVE ( 'NONE', #48597, #17465, #6439, .T. ) ;
#30507 = VECTOR ( 'NONE', #28529, 1000.000000000000000 ) ;
#30508 = AXIS2_PLACEMENT_3D ( 'NONE', #22191, #27094, #11349 ) ;
#30509 = ORIENTED_EDGE ( 'NONE', *, *, #42892, .F. ) ;
#30510 = CARTESIAN_POINT ( 'NONE',  ( -10.54994933093899867, -13.24305344519376959, 71.49356453765415154 ) ) ;
#30511 = CARTESIAN_POINT ( 'NONE',  ( -17.42409385541299471, -14.80920654474435594, 52.02966884056656482 ) ) ;
#30512 = ORIENTED_EDGE ( 'NONE', *, *, #36711, .F. ) ;
#30513 = EDGE_CURVE ( 'NONE', #9257, #1174, #42698, .T. ) ;
#30514 = DIRECTION ( 'NONE',  ( -3.071710424422018668E-17, 6.404604876783312462E-16, 1.000000000000000000 ) ) ;
#30515 = CARTESIAN_POINT ( 'NONE',  ( -23.81768792596037798, -11.95822681598703063, 59.76619129867536628 ) ) ;
#30516 = FACE_OUTER_BOUND ( 'NONE', #23773, .T. ) ;
#30517 = ORIENTED_EDGE ( 'NONE', *, *, #17708, .T. ) ;
#30518 = PLANE ( 'NONE',  #14206 ) ;
#30519 = CARTESIAN_POINT ( 'NONE',  ( -10.90063107880032867, -21.18736481497725421, 54.44843099904677075 ) ) ;
#30520 = CARTESIAN_POINT ( 'NONE',  ( -11.39216336840796373, -18.45920852072106300, 61.29182966166492719 ) ) ;
#30521 = VERTEX_POINT ( 'NONE', #20539 ) ;
#30522 = DIRECTION ( 'NONE',  ( 1.224646799147353207E-16, 1.000000000000000000, -1.912410701131276611E-32 ) ) ;
#30523 = CARTESIAN_POINT ( 'NONE',  ( -21.57995947450667984, -9.113990939708571659, 70.14604673427196246 ) ) ;
#30524 = EDGE_LOOP ( 'NONE', ( #36584, #13778, #25471, #11688, #42712 ) ) ;
#30525 = VERTEX_POINT ( 'NONE', #5032 ) ;
#30526 = PLANE ( 'NONE',  #32260 ) ;
#30527 = CARTESIAN_POINT ( 'NONE',  ( 18.87590614458706995, 1.890747609047893185, 50.53028072113869484 ) ) ;
#30528 = CARTESIAN_POINT ( 'NONE',  ( 18.07590614458695200, 2.144077342217588722, 49.43104278224995340 ) ) ;
#30529 = CARTESIAN_POINT ( 'NONE',  ( -13.38659385759799214, -7.222650657624104298, 49.61879703869476543 ) ) ;
#30530 = CARTESIAN_POINT ( 'NONE',  ( -13.07932274695846964, -16.56597809083076100, 49.52966884056655772 ) ) ;
#30531 = CARTESIAN_POINT ( 'NONE',  ( -17.09591293804728807, -10.13421140726271297, 49.52966884056655772 ) ) ;
#30532 = CYLINDRICAL_SURFACE ( 'NONE', #18447, 1.249999999999998668 ) ;
#30533 = CARTESIAN_POINT ( 'NONE',  ( -10.79572441526863180, -11.40795732096215254, 67.80359905390240272 ) ) ;
#30534 = VERTEX_POINT ( 'NONE', #9210 ) ;
#30535 = DIRECTION ( 'NONE',  ( -0.9918916210775229336, -0.1270866320121812332, 6.503929234589265847E-08 ) ) ;
#30536 =( LENGTH_UNIT ( ) NAMED_UNIT ( * ) SI_UNIT ( .MILLI., .METRE. ) );
#30537 = CARTESIAN_POINT ( 'NONE',  ( -17.06879511326789256, -7.767867012253359071, 73.97490359703523666 ) ) ;
#30538 = FACE_OUTER_BOUND ( 'NONE', #40349, .T. ) ;
#30539 = CIRCLE ( 'NONE', #17128, 2.000000000000000888 ) ;
#30540 = AXIS2_PLACEMENT_3D ( 'NONE', #13870, #2086, #21300 ) ;
#30541 = ORIENTED_EDGE ( 'NONE', *, *, #26815, .T. ) ;
#30542 = VECTOR ( 'NONE', #20620, 1000.000000000000114 ) ;
#30543 = ORIENTED_EDGE ( 'NONE', *, *, #9071, .T. ) ;
#30544 = EDGE_CURVE ( 'NONE', #44170, #22485, #11907, .T. ) ;
#30545 = CARTESIAN_POINT ( 'NONE',  ( -50.42609385541305755, -14.90920654474427565, 73.09411764705880898 ) ) ;
#30546 = CARTESIAN_POINT ( 'NONE',  ( -12.79725838692604434, -20.12850099319811292, 71.80653676770127447 ) ) ;
#30547 = CARTESIAN_POINT ( 'NONE',  ( -21.89130958583942288, -9.354787850460871468, 63.20625856529903075 ) ) ;
#30548 = CARTESIAN_POINT ( 'NONE',  ( -10.05862351292959467, -15.92886012141397245, 64.69266982328383619 ) ) ;
#30549 = AXIS2_PLACEMENT_3D ( 'NONE', #41268, #18865, #37309 ) ;
#30550 = ORIENTED_EDGE ( 'NONE', *, *, #12337, .T. ) ;
#30551 = DIRECTION ( 'NONE',  ( -5.935091885548698876E-07, -2.117535313761473712E-07, 0.9999999999998014921 ) ) ;
#30552 = CARTESIAN_POINT ( 'NONE',  ( -13.27770465421436619, -9.107456272842560097, 64.20946529204060482 ) ) ;
#30553 = VERTEX_POINT ( 'NONE', #38991 ) ;
#30554 = DIRECTION ( 'NONE',  ( 1.616182858256158472E-16, 0.003028072113829171491, -0.9999954153791273948 ) ) ;
#30555 = FACE_OUTER_BOUND ( 'NONE', #25390, .T. ) ;
#30556 = ORIENTED_EDGE ( 'NONE', *, *, #4349, .F. ) ;
#30557 = CARTESIAN_POINT ( 'NONE',  ( -45.92409385541306222, -14.20920654474410760, 70.50000000000000000 ) ) ;
#30558 = ADVANCED_FACE ( 'NONE', ( #46873 ), #14318, .T. ) ;
#30559 = ORIENTED_EDGE ( 'NONE', *, *, #37606, .F. ) ;
#30560 = CARTESIAN_POINT ( 'NONE',  ( -22.51726263819124441, -19.68384825699994423, 72.79400547081151274 ) ) ;
#30561 = CARTESIAN_POINT ( 'NONE',  ( -20.39214861733253770, -8.469596852450818503, 63.50224710712079457 ) ) ;
#30562 = ORIENTED_EDGE ( 'NONE', *, *, #27895, .T. ) ;
#30563 = CARTESIAN_POINT ( 'NONE',  ( -9.982716954774490503, -14.44908413001617298, 67.97304700561097945 ) ) ;
#30564 = ADVANCED_FACE ( 'NONE', ( #46145 ), #12404, .T. ) ;
#30565 = EDGE_CURVE ( 'NONE', #30011, #19030, #36327, .T. ) ;
#30566 = DIRECTION ( 'NONE',  ( -1.066846703571655765E-06, 9.113387012630844478E-06, 0.9999999999579040066 ) ) ;
#30567 = CARTESIAN_POINT ( 'NONE',  ( -21.88034385650551883, -6.424090610841176385, 49.80797279389978627 ) ) ;
#30568 = CARTESIAN_POINT ( 'NONE',  ( -12.87522519725752268, -8.909181681006783649, 67.52942783090081491 ) ) ;
#30569 = AXIS2_PLACEMENT_3D ( 'NONE', #9869, #47304, #24886 ) ;
#30570 = CARTESIAN_POINT ( 'NONE',  ( -18.91168463870544869, -7.914867951563272719, 63.31600393140114136 ) ) ;
#30571 = CARTESIAN_POINT ( 'NONE',  ( -10.66703363856100317, -12.79807828486586807, 64.26836111018113229 ) ) ;
#30572 = ORIENTED_EDGE ( 'NONE', *, *, #21274, .T. ) ;
#30573 = CARTESIAN_POINT ( 'NONE',  ( -19.18784625403669963, -21.58347547587811377, 58.52507428381958476 ) ) ;
#30574 = AXIS2_PLACEMENT_3D ( 'NONE', #10943, #44443, #33822 ) ;
#30575 = VECTOR ( 'NONE', #19847, 1000.000000000000000 ) ;
#30576 = CARTESIAN_POINT ( 'NONE',  ( -13.43773910423563400, -20.62433115109003268, 58.33177939114180788 ) ) ;
#30577 = DIRECTION ( 'NONE',  ( -3.071710424422018668E-17, 6.404604876783312462E-16, 1.000000000000000000 ) ) ;
#30578 = CARTESIAN_POINT ( 'NONE',  ( -24.84449963183508459, -13.71944596863515464, 53.49999999999994316 ) ) ;
#30579 = CARTESIAN_POINT ( 'NONE',  ( -17.06648941491218707, -7.818287007874094030, 70.56323971375660165 ) ) ;
#30580 = ORIENTED_EDGE ( 'NONE', *, *, #8005, .T. ) ;
#30581 = ORIENTED_EDGE ( 'NONE', *, *, #34370, .F. ) ;
#30582 = DIRECTION ( 'NONE',  ( 0.4251432040024066827, 0.9051260995521939190, 1.185120001106693976E-09 ) ) ;
#30583 = LINE ( 'NONE', #11859, #27370 ) ;
#30584 = ORIENTED_EDGE ( 'NONE', *, *, #35114, .F. ) ;
#30585 = CARTESIAN_POINT ( 'NONE',  ( -23.22909885928854834, -6.086929677699679075, 53.49999999999995026 ) ) ;
#30586 = CARTESIAN_POINT ( 'NONE',  ( -15.74539340629102924, -7.550670488425484272, 67.31724133890321582 ) ) ;
#30587 = AXIS2_PLACEMENT_3D ( 'NONE', #30496, #11771, #26790 ) ;
#30588 = FACE_OUTER_BOUND ( 'NONE', #12457, .T. ) ;
#30589 = FACE_OUTER_BOUND ( 'NONE', #46097, .T. ) ;
#30590 = CARTESIAN_POINT ( 'NONE',  ( -14.22441598498101989, -8.081217260141077219, 67.44470407312981308 ) ) ;
#30591 = CARTESIAN_POINT ( 'NONE',  ( -24.29039363205059843, -16.40874438636378230, 59.12892251125953891 ) ) ;
#30592 = FACE_OUTER_BOUND ( 'NONE', #38250, .T. ) ;
#30593 = DIRECTION ( 'NONE',  ( 4.115385489419892128E-17, 0.9999954153791273948, 0.003028072113818697231 ) ) ;
#30594 = EDGE_CURVE ( 'NONE', #47031, #2695, #22449, .T. ) ;
#30595 = CARTESIAN_POINT ( 'NONE',  ( -17.42409385541299471, -14.80920654474434883, 62.02966884056656482 ) ) ;
#30596 = CARTESIAN_POINT ( 'NONE',  ( -12.11086159817483932, -20.03164753588056257, 61.51865900489719508 ) ) ;
#30597 = CARTESIAN_POINT ( 'NONE',  ( -13.79232328012607312, -20.79486899771962172, 68.68455086219127281 ) ) ;
#30598 = CARTESIAN_POINT ( 'NONE',  ( -19.77787797429642325, -21.45850311741518368, 72.49658723834933483 ) ) ;
#30599 =( BOUNDED_SURFACE ( )  B_SPLINE_SURFACE ( 3, 1, ( 
 ( #24986, #2331 ),
 ( #28196, #2577 ),
 ( #36294, #17577 ),
 ( #5798, #17338 ),
 ( #21540, #16849 ),
 ( #31889, #39756 ),
 ( #39277, #39519 ) ),
 .UNSPECIFIED., .T., .F., .F. ) 
 B_SPLINE_SURFACE_WITH_KNOTS ( ( 4, 3, 4 ),
 ( 2, 2 ),
 ( 0.000000000000000000, 0.5000000000000000000, 1.000000000000000000 ),
 ( 0.000000000000000000, 1.000000000000000000 ),
 .UNSPECIFIED. ) 
 GEOMETRIC_REPRESENTATION_ITEM ( )  RATIONAL_B_SPLINE_SURFACE ( (
 ( 1.000000000000000000, 1.000000000000000000),
 ( 0.3333333333333335369, 0.3333333333333330373),
 ( 0.3333333333333335369, 0.3333333333333330373),
 ( 1.000000000000000000, 1.000000000000000000),
 ( 0.3333333333333333703, 0.3333333333333333703),
 ( 0.3333333333333333703, 0.3333333333333333703),
 ( 1.000000000000000000, 1.000000000000000000) ) ) 
 REPRESENTATION_ITEM ( '' )  SURFACE ( )  );
#30600 = CARTESIAN_POINT ( 'NONE',  ( -18.45262242793555885, -21.79183460504582470, 65.50099240037707204 ) ) ;
#30601 = ORIENTED_EDGE ( 'NONE', *, *, #44739, .T. ) ;
#30602 = VERTEX_POINT ( 'NONE', #28157 ) ;
#30603 = CARTESIAN_POINT ( 'NONE',  ( -20.23203131230217267, -21.71059417314907591, 72.51823477531823414 ) ) ;
#30604 = ORIENTED_EDGE ( 'NONE', *, *, #44209, .T. ) ;
#30605 = CARTESIAN_POINT ( 'NONE',  ( -46.29409385541305966, -12.76354662275040219, 71.04301729251712061 ) ) ;
#30606 = VECTOR ( 'NONE', #4219, 1000.000000000000000 ) ;
#30607 = B_SPLINE_CURVE_WITH_KNOTS ( 'NONE', 1,
 ( #24039, #1360 ),
 .UNSPECIFIED., .F., .F.,
 ( 2, 2 ),
 ( 0.000000000000000000, 1.000000000000000000 ),
 .UNSPECIFIED. ) ;
#30608 = CARTESIAN_POINT ( 'NONE',  ( -22.78151503426583702, -19.98625364524674097, 72.75905110386234753 ) ) ;
#30609 =( BOUNDED_SURFACE ( )  B_SPLINE_SURFACE ( 3, 1, ( 
 ( #47233, #43785 ),
 ( #21131, #21381 ),
 ( #13477, #10046 ),
 ( #2649, #28994 ),
 ( #17658, #32685 ),
 ( #47705, #40323 ),
 ( #15409, #26771 ) ),
 .UNSPECIFIED., .T., .F., .F. ) 
 B_SPLINE_SURFACE_WITH_KNOTS ( ( 4, 3, 4 ),
 ( 2, 2 ),
 ( 0.000000000000000000, 0.5000000000000000000, 1.000000000000000000 ),
 ( 0.000000000000000000, 1.000000000000000000 ),
 .UNSPECIFIED. ) 
 GEOMETRIC_REPRESENTATION_ITEM ( )  RATIONAL_B_SPLINE_SURFACE ( (
 ( 1.000000000000000000, 1.000000000000000000),
 ( 0.3333333333333335369, 0.3333333333333330373),
 ( 0.3333333333333335369, 0.3333333333333330373),
 ( 1.000000000000000000, 1.000000000000000000),
 ( 0.3333333333333333703, 0.3333333333333333703),
 ( 0.3333333333333333703, 0.3333333333333333703),
 ( 1.000000000000000000, 1.000000000000000000) ) ) 
 REPRESENTATION_ITEM ( '' )  SURFACE ( )  );
#30610 = VECTOR ( 'NONE', #9453, 1000.000000000000114 ) ;
#30611 = VECTOR ( 'NONE', #28825, 1000.000000000000114 ) ;
#30612 = CARTESIAN_POINT ( 'NONE',  ( -16.00544582274271477, -7.903112417841744453, 63.95538887075813506 ) ) ;
#30613 = CARTESIAN_POINT ( 'NONE',  ( -16.11840895131430429, -22.14390444347510822, 58.48596779410638646 ) ) ;
#30614 = ORIENTED_EDGE ( 'NONE', *, *, #18582, .T. ) ;
#30615 = CARTESIAN_POINT ( 'NONE',  ( -15.95021555058110607, -7.506329832067567764, 63.79198235507756465 ) ) ;
#30616 = AXIS2_PLACEMENT_3D ( 'NONE', #37557, #26254, #7555 ) ;
#30617 = FACE_OUTER_BOUND ( 'NONE', #40955, .T. ) ;
#30618 = ORIENTED_EDGE ( 'NONE', *, *, #7572, .F. ) ;
#30619 = CARTESIAN_POINT ( 'NONE',  ( -10.79220951835107023, -12.56890123353462307, 57.55530741402424155 ) ) ;
#30620 = FACE_OUTER_BOUND ( 'NONE', #33727, .T. ) ;
#30621 =( BOUNDED_SURFACE ( )  B_SPLINE_SURFACE ( 3, 1, ( 
 ( #48344, #45399 ),
 ( #7496, #40968 ),
 ( #45170, #22496 ),
 ( #7741, #26434 ),
 ( #7252, #29640 ),
 ( #41702, #2625 ),
 ( #18542, #37493 ) ),
 .UNSPECIFIED., .T., .F., .F. ) 
 B_SPLINE_SURFACE_WITH_KNOTS ( ( 4, 3, 4 ),
 ( 2, 2 ),
 ( 0.000000000000000000, 0.5000000000000000000, 1.000000000000000000 ),
 ( 0.000000000000000000, 1.000000000000000000 ),
 .UNSPECIFIED. ) 
 GEOMETRIC_REPRESENTATION_ITEM ( )  RATIONAL_B_SPLINE_SURFACE ( (
 ( 1.000000000000000000, 1.000000000000000000),
 ( 0.3333333333333335369, 0.3333333333333330373),
 ( 0.3333333333333335369, 0.3333333333333330373),
 ( 1.000000000000000000, 1.000000000000000000),
 ( 0.3333333333333333703, 0.3333333333333333703),
 ( 0.3333333333333333703, 0.3333333333333333703),
 ( 1.000000000000000000, 1.000000000000000000) ) ) 
 REPRESENTATION_ITEM ( '' )  SURFACE ( )  );
#30622 = ORIENTED_EDGE ( 'NONE', *, *, #48078, .T. ) ;
#30623 = CARTESIAN_POINT ( 'NONE',  ( -13.42648243792925378, -12.34047032955235679, 49.52966884056655772 ) ) ;
#30624 = CARTESIAN_POINT ( 'NONE',  ( -16.78341102624552050, -22.23169286577646986, 68.88055947109249644 ) ) ;
#30625 = CARTESIAN_POINT ( 'NONE',  ( -22.58065782673598321, -12.89613362149922438, 53.49999999999995026 ) ) ;
#30626 = ORIENTED_EDGE ( 'NONE', *, *, #43652, .F. ) ;
#30627 = CARTESIAN_POINT ( 'NONE',  ( -17.42409385541299471, -14.80920654474435771, 49.52966884056655772 ) ) ;
#30628 = EDGE_CURVE ( 'NONE', #18626, #1976, #12771, .T. ) ;
#30629 = FACE_OUTER_BOUND ( 'NONE', #27498, .T. ) ;
#30630 = CYLINDRICAL_SURFACE ( 'NONE', #44968, 1.249999999999998668 ) ;
#30631 = ORIENTED_EDGE ( 'NONE', *, *, #12545, .F. ) ;
#30632 = CARTESIAN_POINT ( 'NONE',  ( -17.38034385759799250, -9.360768649639311434, 51.01397948905922419 ) ) ;
#30633 = DIRECTION ( 'NONE',  ( -0.1186632576870824130, 0.9929345553837299887, 6.051931679537041823E-08 ) ) ;
#30634 = CARTESIAN_POINT ( 'NONE',  ( -20.85321405943728834, -20.91189875045330737, 62.41471372066478551 ) ) ;
#30635 = EDGE_CURVE ( 'NONE', #36955, #19273, #43185, .T. ) ;
#30636 = ADVANCED_FACE ( 'NONE', ( #40216 ), #40801, .T. ) ;
#30637 = CARTESIAN_POINT ( 'NONE',  ( -22.33376602745314798, -19.86903051493497685, 69.18890041286789483 ) ) ;
#30638 = CARTESIAN_POINT ( 'NONE',  ( -19.76784385650551457, -6.428312510596451368, 51.20221977374900035 ) ) ;
#30640 = EDGE_CURVE ( 'NONE', #29387, #17516, #34204, .T. ) ;
#30639 = ORIENTED_EDGE ( 'NONE', *, *, #43012, .F. ) ;
#30641 = AXIS2_PLACEMENT_3D ( 'NONE', #32082, #35526, #43167 ) ;
#30642 = CARTESIAN_POINT ( 'NONE',  ( -24.10584592916820057, -12.56049825913868645, 73.24225570139947195 ) ) ;
#30643 = DIRECTION ( 'NONE',  ( -3.071710424422018668E-17, 6.404604876783312462E-16, 1.000000000000000000 ) ) ;
#30644 = VERTEX_POINT ( 'NONE', #47605 ) ;
#30645 = DIRECTION ( 'NONE',  ( -1.148482744091818979E-06, 2.957121237693701878E-08, 0.9999999999993399724 ) ) ;
#30646 = EDGE_CURVE ( 'NONE', #35257, #10902, #9555, .T. ) ;
#30647 = DIRECTION ( 'NONE',  ( -5.551115123125782702E-17, -1.232595164407830946E-32, -1.000000000000000000 ) ) ;
#30648 = CARTESIAN_POINT ( 'NONE',  ( -13.11946000997128436, -9.225961346166455357, 67.52942785706356688 ) ) ;
#30649 = ORIENTED_EDGE ( 'NONE', *, *, #46117, .F. ) ;
#30650 = CARTESIAN_POINT ( 'NONE',  ( -21.24554616535955631, -21.20453920045676810, 65.76949338751086316 ) ) ;
#30651 = AXIS2_PLACEMENT_3D ( 'NONE', #16509, #9637, #9141 ) ;
#30652 = CIRCLE ( 'NONE', #46348, 1.049999999999998934 ) ;
#30653 = CARTESIAN_POINT ( 'NONE',  ( -24.42340526462838923, -14.70674901051565975, 59.46973661257310084 ) ) ;
#30654 = CARTESIAN_POINT ( 'NONE',  ( -23.48373383537063930, -18.31359856532379737, 72.95471315433937320 ) ) ;
#30655 = EDGE_CURVE ( 'NONE', #39625, #46585, #19381, .T. ) ;
#30656 = VERTEX_POINT ( 'NONE', #13598 ) ;
#30657 = CARTESIAN_POINT ( 'NONE',  ( -14.93034385650551599, -9.794322478646142471, 51.19202720610083901 ) ) ;
#30658 = VECTOR ( 'NONE', #43843, 1000.000000000000000 ) ;
#30659 = LINE ( 'NONE', #12403, #5953 ) ;
#30660 = CARTESIAN_POINT ( 'NONE',  ( -21.80947544975385810, -9.353161466788067813, 63.19153755920122251 ) ) ;
#30661 = DIRECTION ( 'NONE',  ( -0.000000000000000000, -1.000000000000000000, -0.000000000000000000 ) ) ;
#30662 = CARTESIAN_POINT ( 'NONE',  ( -30.42409385541305156, -8.109206544744111511, 49.25000000000000000 ) ) ;
#30663 = VERTEX_POINT ( 'NONE', #45134 ) ;
#30664 = ORIENTED_EDGE ( 'NONE', *, *, #3386, .T. ) ;
#30665 = CARTESIAN_POINT ( 'NONE',  ( -22.63659385541304303, -8.995762431863214559, 51.38120296130585274 ) ) ;
#30666 = CARTESIAN_POINT ( 'NONE',  ( -16.94458633259734270, -7.374567983260779336, 74.14513688882354359 ) ) ;
#30667 = CARTESIAN_POINT ( 'NONE',  ( -18.98390459359973548, -7.933620001262258192, 66.91543923465640376 ) ) ;
#30668 = DIRECTION ( 'NONE',  ( -3.071710424422018668E-17, 6.404604876783312462E-16, 1.000000000000000000 ) ) ;
#30669 = CARTESIAN_POINT ( 'NONE',  ( -15.32672178808326535, -21.95796145784420261, 72.30221390644346968 ) ) ;
#30670 = CARTESIAN_POINT ( 'NONE',  ( -20.05785487306503256, -7.839488668639425839, 73.83441365354759967 ) ) ;
#30671 = CARTESIAN_POINT ( 'NONE',  ( -24.77723877343947478, -16.00713684962007122, 66.24820200538215431 ) ) ;
#30672 = ADVANCED_FACE ( 'NONE', ( #14791 ), #45020, .T. ) ;
#30673 = ORIENTED_EDGE ( 'NONE', *, *, #4312, .T. ) ;
#30674 = FACE_OUTER_BOUND ( 'NONE', #34387, .T. ) ;
#30675 = AXIS2_PLACEMENT_3D ( 'NONE', #20345, #12225, #20594 ) ;
#30676 = ORIENTED_EDGE ( 'NONE', *, *, #4562, .F. ) ;
#30677 = CARTESIAN_POINT ( 'NONE',  ( -17.42409385541299471, -14.80920654474434883, 62.02966884056656482 ) ) ;
#30678 = CARTESIAN_POINT ( 'NONE',  ( -24.39403702774331606, -17.44049340399234893, 69.52844358061491903 ) ) ;
#30679 = DIRECTION ( 'NONE',  ( 1.927470528863184130E-16, 1.434740771370715221E-29, -1.000000000000000000 ) ) ;
#30680 = ADVANCED_FACE ( 'NONE', ( #22465 ), #15618, .T. ) ;
#30681 = ORIENTED_EDGE ( 'NONE', *, *, #1877, .F. ) ;
#30682 = CARTESIAN_POINT ( 'NONE',  ( -10.33431758219403207, -12.52035302217920254, 60.98348881056122650 ) ) ;
#30683 = CARTESIAN_POINT ( 'NONE',  ( -14.68422391818051587, -7.881140326852841937, 60.48142765572568180 ) ) ;
#30684 = CARTESIAN_POINT ( 'NONE',  ( -23.30282330091471366, -18.60927750845715067, 69.29371984660140527 ) ) ;
#30685 = CARTESIAN_POINT ( 'NONE',  ( -24.46506320217640962, -17.24406362331221132, 72.99840605271779737 ) ) ;
#30686 = ORIENTED_EDGE ( 'NONE', *, *, #37842, .F. ) ;
#30687 = CARTESIAN_POINT ( 'NONE',  ( -10.33966868199281386, -17.11483672006214718, 57.84793901998011023 ) ) ;
#30688 = CARTESIAN_POINT ( 'NONE',  ( -6.424093855413055110, -25.10920654474410441, 81.99999999999998579 ) ) ;
#30689 = CARTESIAN_POINT ( 'NONE',  ( -13.71073213066623531, -18.52046572475129338, 49.52966884056656482 ) ) ;
#30690 = LINE ( 'NONE', #30931, #7725 ) ;
#30691 = CONTEXT_DEPENDENT_SHAPE_REPRESENTATION ( #32234, #3998 ) ;
#30692 = VERTEX_POINT ( 'NONE', #18764 ) ;
#30693 = CARTESIAN_POINT ( 'NONE',  ( -20.87011516470288797, -20.96386168028406871, 58.64475080180090316 ) ) ;
#30694 = DIRECTION ( 'NONE',  ( 0.2393415023380396356, -0.9709354485539014590, 6.438601123316498798E-08 ) ) ;
#30695 = AXIS2_PLACEMENT_3D ( 'NONE', #48467, #3173, #47746 ) ;
#30696 = FACE_OUTER_BOUND ( 'NONE', #40967, .T. ) ;
#30697 = EDGE_CURVE ( 'NONE', #42591, #6937, #35538, .T. ) ;
#30698 = LINE ( 'NONE', #42500, #28244 ) ;
#30699 = ORIENTED_EDGE ( 'NONE', *, *, #43521, .F. ) ;
#30700 = CARTESIAN_POINT ( 'NONE',  ( -10.10423179225323054, -16.19963241119870645, 71.63405780323361682 ) ) ;
#30701 = EDGE_CURVE ( 'NONE', #2071, #28807, #5591, .T. ) ;
#30702 = EDGE_LOOP ( 'NONE', ( #47333, #5164, #41881, #37299, #44572 ) ) ;
#30703 = CARTESIAN_POINT ( 'NONE',  ( -7.334870405450504727, -11.98365049024292972, 53.49999999999995026 ) ) ;
#30704 = LINE ( 'NONE', #27715, #28238 ) ;
#30705 = EDGE_LOOP ( 'NONE', ( #11878, #44289, #3112, #3239 ) ) ;
#30706 = EDGE_CURVE ( 'NONE', #18406, #17425, #10379, .T. ) ;
#30707 = CARTESIAN_POINT ( 'NONE',  ( -12.97364571557156232, -9.395203622806569399, 49.41430056510258595 ) ) ;
#30708 = EDGE_LOOP ( 'NONE', ( #36307, #37597, #11922, #24556, #29416 ) ) ;
#30709 = ORIENTED_EDGE ( 'NONE', *, *, #9149, .F. ) ;
#30710 = ORIENTED_EDGE ( 'NONE', *, *, #41183, .T. ) ;
#30711 = CARTESIAN_POINT ( 'NONE',  ( -40.92409385541305511, -14.80920654474410725, 74.99999999999998579 ) ) ;
#30712 = AXIS2_PLACEMENT_3D ( 'NONE', #37672, #21933, #10849 ) ;
#30713 = CARTESIAN_POINT ( 'NONE',  ( -13.71293426195967413, -21.26916566922604801, 68.64120525947689089 ) ) ;
#30715 = ADVANCED_FACE ( 'NONE', ( #30113 ), #7464, .T. ) ;
#30714 = DIRECTION ( 'NONE',  ( 0.9811758422909349076, 0.1931164583992469319, 7.863147543881890502E-08 ) ) ;
#30716 = CARTESIAN_POINT ( 'NONE',  ( -24.17271849214968071, -12.95015691860989371, 66.60246741689840633 ) ) ;
#30717 = CARTESIAN_POINT ( 'NONE',  ( -11.81163076501576015, -9.909691595435425882, 64.16767832365785296 ) ) ;
#30718 = AXIS2_PLACEMENT_3D ( 'NONE', #26283, #3627, #15668 ) ;
#30719 = VERTEX_POINT ( 'NONE', #37715 ) ;
#30720 = ORIENTED_EDGE ( 'NONE', *, *, #32261, .F. ) ;
#30721 = CARTESIAN_POINT ( 'NONE',  ( -24.83263366448169762, -15.59490076022755112, 73.18799035805197661 ) ) ;
#30722 = CARTESIAN_POINT ( 'NONE',  ( -10.37743716876973643, -14.51010320183636715, 64.27315137562472103 ) ) ;
#30723 = CARTESIAN_POINT ( 'NONE',  ( -24.14992822999210276, -18.01341164000503525, 59.11882993461590274 ) ) ;
#30724 = VECTOR ( 'NONE', #24483, 1000.000000000000227 ) ;
#30725 = CARTESIAN_POINT ( 'NONE',  ( -11.42622084110231029, -18.51434063454203738, 61.27710833181470917 ) ) ;
#30726 = VERTEX_POINT ( 'NONE', #11622 ) ;
#30727 = B_SPLINE_CURVE_WITH_KNOTS ( 'NONE', 3,
 ( #34248, #38183, #534, #45357, #15777, #33761, #19480, #45614, #46078, #22710 ),
 .UNSPECIFIED., .F., .F.,
 ( 4, 2, 2, 2, 4 ),
 ( 0.1272669073658455330, 0.2522669073463257861, 0.3772669073268060114, 0.5022669073072862922, 0.6272669072877665730 ),
 .UNSPECIFIED. ) ;
#30728 = CARTESIAN_POINT ( 'NONE',  ( -14.31159385650551741, -6.922745924619793101, 51.69366785382590024 ) ) ;
#30729 = VERTEX_POINT ( 'NONE', #22969 ) ;
#30730 = CARTESIAN_POINT ( 'NONE',  ( -10.01440787728688520, -14.03439562150409969, 61.03325889150411143 ) ) ;
#30731 = DIRECTION ( 'NONE',  ( -0.9687793358424819923, 0.2479245821708680464, 0.000000000000000000 ) ) ;
#30732 = FACE_OUTER_BOUND ( 'NONE', #4662, .T. ) ;
#30733 = EDGE_CURVE ( 'NONE', #41749, #14925, #4005, .T. ) ;
#30734 = ORIENTED_EDGE ( 'NONE', *, *, #28511, .T. ) ;
#30735 = CARTESIAN_POINT ( 'NONE',  ( -22.53429313110963506, -9.952421254863264011, 73.78161091678163075 ) ) ;
#30736 = CARTESIAN_POINT ( 'NONE',  ( -10.47425521701617157, -17.49314416303823450, 64.81234701634230078 ) ) ;
#30737 = CARTESIAN_POINT ( 'NONE',  ( -24.19967835704668246, -11.71176484350101354, 59.58261478314079795 ) ) ;
#30738 = AXIS2_PLACEMENT_3D ( 'NONE', #36343, #25512, #9784 ) ;
#30739 = VERTEX_POINT ( 'NONE', #22224 ) ;
#30740 = CARTESIAN_POINT ( 'NONE',  ( -10.39215600595210631, -14.30487551902977650, 64.38803863383273551 ) ) ;
#30741 =( BOUNDED_CURVE ( )  B_SPLINE_CURVE ( 3, ( #12974, #6328, #28000, #48170 ),
 .UNSPECIFIED., .F., .F. ) 
 B_SPLINE_CURVE_WITH_KNOTS ( ( 4, 4 ),
 ( 0.6435011087932844820, 1.570796326794896558 ),
 .UNSPECIFIED. ) 
 CURVE ( )  GEOMETRIC_REPRESENTATION_ITEM ( )  RATIONAL_B_SPLINE_CURVE ( ( 1.000000000000000000, 0.9296181273332770889, 0.9296181273332770889, 1.000000000000000000 ) ) 
 REPRESENTATION_ITEM ( '' )  );
#30742 = CARTESIAN_POINT ( 'NONE',  ( -17.29025345054776963, -7.359659516233258536, 67.13384346071842401 ) ) ;
#30743 = DIRECTION ( 'NONE',  ( -1.616182858256118783E-16, -0.003028072113822189229, 0.9999954153791275058 ) ) ;
#30744 = EDGE_LOOP ( 'NONE', ( #6834, #42805, #41589, #10206, #20730 ) ) ;
#30745 = CARTESIAN_POINT ( 'NONE',  ( -24.45201639769885205, -14.25170802724723451, 69.80275273439818307 ) ) ;
#30746 = AXIS2_PLACEMENT_3D ( 'NONE', #44715, #34092, #14616 ) ;
#30747 = ORIENTED_EDGE ( 'NONE', *, *, #5265, .F. ) ;
#30748 = CARTESIAN_POINT ( 'NONE',  ( -18.66311988809301425, -7.868636481342422329, 70.65595886192740238 ) ) ;
#30749 = ORIENTED_EDGE ( 'NONE', *, *, #30419, .T. ) ;
#30750 = CARTESIAN_POINT ( 'NONE',  ( -22.16045306466799403, -20.56002303229518446, 58.92589421280841577 ) ) ;
#30751 = LINE ( 'NONE', #45777, #16091 ) ;
#30752 = CARTESIAN_POINT ( 'NONE',  ( -11.61908885153752813, -23.53148341178916425, 53.49999999999995026 ) ) ;
#30753 = ADVANCED_FACE ( 'NONE', ( #40680 ), #12187, .T. ) ;
#30754 = ORIENTED_EDGE ( 'NONE', *, *, #27395, .F. ) ;
#30755 = CARTESIAN_POINT ( 'NONE',  ( -17.92193035392797285, -21.84160718002658541, 61.87535923543196503 ) ) ;
#30756 = AXIS2_PLACEMENT_3D ( 'NONE', #6543, #40035, #44231 ) ;
#30757 = EDGE_CURVE ( 'NONE', #41525, #26808, #15787, .T. ) ;
#30758 = CARTESIAN_POINT ( 'NONE',  ( -10.13055098088643646, -13.29041361134464516, 74.82817645606137091 ) ) ;
#30759 = CARTESIAN_POINT ( 'NONE',  ( -11.17827002090033339, -11.53132166989810337, 71.38860948999864320 ) ) ;
#30760 = VERTEX_POINT ( 'NONE', #16027 ) ;
#30761 = CARTESIAN_POINT ( 'NONE',  ( -12.10369346210734243, -9.594120923840563364, 57.27430859790474926 ) ) ;
#30762 =( BOUNDED_CURVE ( )  B_SPLINE_CURVE ( 3, ( #23172, #762, #15756, #26618 ),
 .UNSPECIFIED., .F., .F. ) 
 B_SPLINE_CURVE_WITH_KNOTS ( ( 4, 4 ),
 ( 0.9074455897393695070, 1.000000000000000000 ),
 .UNSPECIFIED. ) 
 CURVE ( )  GEOMETRIC_REPRESENTATION_ITEM ( )  RATIONAL_B_SPLINE_CURVE ( ( 0.6983129098261110501, 0.7760317562607137454, 0.8765941196520100620, 1.000000000000000000 ) ) 
 REPRESENTATION_ITEM ( '' )  );
#30763 = EDGE_CURVE ( 'NONE', #26171, #42055, #24429, .T. ) ;
#30764 = CARTESIAN_POINT ( 'NONE',  ( -12.64139926011484505, -9.624549101048229360, 74.31922783352578676 ) ) ;
#30766 = ORIENTED_EDGE ( 'NONE', *, *, #23237, .T. ) ;
#30765 = VECTOR ( 'NONE', #33857, 1000.000000000000000 ) ;
#30767 = VERTEX_POINT ( 'NONE', #34257 ) ;
#30768 = FACE_OUTER_BOUND ( 'NONE', #5064, .T. ) ;
#30769 = CARTESIAN_POINT ( 'NONE',  ( -13.71339271347209987, -20.80363700974685059, 65.28628881287177421 ) ) ;
#30770 = DIRECTION ( 'NONE',  ( 0.000000000000000000, -0.9999954153791273948, -0.003028072113819838245 ) ) ;
#30771 = ADVANCED_FACE ( 'NONE', ( #42400 ), #38693, .T. ) ;
#30772 = CARTESIAN_POINT ( 'NONE',  ( -22.52409385650551954, -6.426201560718812544, 50.50509628382439331 ) ) ;
#30773 = CARTESIAN_POINT ( 'NONE',  ( -20.31649760022732565, -7.943510736669368910, 70.43595667626200907 ) ) ;
#30774 = CARTESIAN_POINT ( 'NONE',  ( -12.49855684652675514, -19.85736664535339813, 68.75146050727752822 ) ) ;
#30775 = CARTESIAN_POINT ( 'NONE',  ( -23.30282546666849086, -18.60927426030231047, 69.59371984657600763 ) ) ;
#30776 = CARTESIAN_POINT ( 'NONE',  ( -20.37299750454370439, -8.405577324698720432, 66.78104082189589974 ) ) ;
#30777 = VERTEX_POINT ( 'NONE', #34755 ) ;
#30779 = CARTESIAN_POINT ( 'NONE',  ( -22.62394951084894146, -10.04809318868971424, 70.29706442286226320 ) ) ;
#30778 = AXIS2_PLACEMENT_3D ( 'NONE', #43559, #9820, #39113 ) ;
#30780 = SHAPE_REPRESENTATION_RELATIONSHIP ( 'NONE' , 'NONE' ,  #2486, #26163 ) ;
#30781 = CARTESIAN_POINT ( 'NONE',  ( -10.02907021082448225, -13.90480008044668381, 57.57012250139395348 ) ) ;
#30782 = CARTESIAN_POINT ( 'NONE',  ( -21.95939004544374740, -9.477125498926222136, 59.72171213236985921 ) ) ;
#30783 = EDGE_CURVE ( 'NONE', #35674, #38958, #27162, .T. ) ;
#30784 = CIRCLE ( 'NONE', #44067, 1.999999999999999556 ) ;
#30785 = ORIENTED_EDGE ( 'NONE', *, *, #32969, .F. ) ;
#30786 = EDGE_CURVE ( 'NONE', #21625, #30729, #138, .T. ) ;
#30787 = VERTEX_POINT ( 'NONE', #27613 ) ;
#30788 = EDGE_CURVE ( 'NONE', #26955, #17516, #16517, .T. ) ;
#30789 = CARTESIAN_POINT ( 'NONE',  ( -29.92409385541305156, -6.359206544744109735, 47.99999999999997868 ) ) ;
#30790 = CARTESIAN_POINT ( 'NONE',  ( -23.12302657392458016, -18.95946740514217765, 62.35406880581414413 ) ) ;
#30791 = CARTESIAN_POINT ( 'NONE',  ( -15.49415775405465823, -8.028509947901662613, 74.37985659017797957 ) ) ;
#30792 = CARTESIAN_POINT ( 'NONE',  ( -16.78411603780843464, -21.83009879966275690, 68.84560651669730191 ) ) ;
#30793 = EDGE_LOOP ( 'NONE', ( #22623, #16500, #10671, #4025, #42172 ) ) ;
#30794 = CARTESIAN_POINT ( 'NONE',  ( -13.02800473326296782, -9.361643555834115560, 70.84925385331725067 ) ) ;
#30795 = CARTESIAN_POINT ( 'NONE',  ( -6.424093855413055110, -25.10920654474410441, 81.99999999999998579 ) ) ;
#30796 = EDGE_LOOP ( 'NONE', ( #16269, #34902, #15109, #24768 ) ) ;
#30797 = CARTESIAN_POINT ( 'NONE',  ( -11.49500183448703083, -10.99442376238782337, 57.22375354680192316 ) ) ;
#30798 = CARTESIAN_POINT ( 'NONE',  ( -24.72409385541305582, -14.90920654474422058, 68.06470588235292496 ) ) ;
#30799 = ORIENTED_EDGE ( 'NONE', *, *, #27890, .T. ) ;
#30800 = FACE_OUTER_BOUND ( 'NONE', #45084, .T. ) ;
#30801 = ORIENTED_EDGE ( 'NONE', *, *, #9875, .F. ) ;
#30802 = DIRECTION ( 'NONE',  ( 0.2479245821708770392, 0.9687793358424796608, -9.885672099568309358E-17 ) ) ;
#30804 = CARTESIAN_POINT ( 'NONE',  ( 18.46573386768564973, 3.116243883476752963, 50.28399048308536123 ) ) ;
#30803 = AXIS2_PLACEMENT_3D ( 'NONE', #24894, #9877, #5709 ) ;
#30805 = B_SPLINE_CURVE_WITH_KNOTS ( 'NONE', 3,
 ( #25672, #37223, #18772, #29868, #21986, #44182, #29616, #36727, #18517, #3015 ),
 .UNSPECIFIED., .F., .F.,
 ( 4, 2, 2, 2, 4 ),
 ( 0.000000000000000000, 0.2500000000000000000, 0.5000000000000000000, 0.7500000000000000000, 1.000000000000000000 ),
 .UNSPECIFIED. ) ;
#30806 = ORIENTED_EDGE ( 'NONE', *, *, #45577, .T. ) ;
#30807 = CARTESIAN_POINT ( 'NONE',  ( -24.42608592195226080, -15.63182493645487803, 73.00863554951556011 ) ) ;
#30808 = FACE_OUTER_BOUND ( 'NONE', #39828, .T. ) ;
#30809 = CARTESIAN_POINT ( 'NONE',  ( -17.54909385650551812, -8.104110260919579645, 48.81699501597546487 ) ) ;
#30810 = VECTOR ( 'NONE', #8517, 1000.000000000000114 ) ;
#30811 = LINE ( 'NONE', #34228, #2390 ) ;
#30812 = B_SPLINE_CURVE_WITH_KNOTS ( 'NONE', 1,
 ( #29353, #36703 ),
 .UNSPECIFIED., .F., .F.,
 ( 2, 2 ),
 ( 0.000000000000000000, 1.000000000000000000 ),
 .UNSPECIFIED. ) ;
#30813 = LINE ( 'NONE', #34473, #41832 ) ;
#30814 = FACE_OUTER_BOUND ( 'NONE', #35467, .T. ) ;
#30815 = ORIENTED_EDGE ( 'NONE', *, *, #30870, .T. ) ;
#30816 = CARTESIAN_POINT ( 'NONE',  ( -23.74619244455239198, -11.68933966055485207, 63.25218278636740621 ) ) ;
#30817 = CARTESIAN_POINT ( 'NONE',  ( -16.33659385541304232, -8.995762431863216335, 51.38120296130585274 ) ) ;
#30818 = FACE_OUTER_BOUND ( 'NONE', #40613, .T. ) ;
#30819 = EDGE_CURVE ( 'NONE', #27387, #11362, #29438, .T. ) ;
#30820 = DIRECTION ( 'NONE',  ( -0.3478314405900307382, -0.9375570856950865561, 0.000000000000000000 ) ) ;
#30821 = PLANE ( 'NONE',  #21635 ) ;
#30822 = ORIENTED_EDGE ( 'NONE', *, *, #16669, .T. ) ;
#30823 = VERTEX_POINT ( 'NONE', #8416 ) ;
#30824 = EDGE_CURVE ( 'NONE', #26563, #4162, #43661, .T. ) ;
#30825 = CARTESIAN_POINT ( 'NONE',  ( -21.44791994599160034, -9.079744384496041931, 73.67299128577275269 ) ) ;
#30826 = CARTESIAN_POINT ( 'NONE',  ( -10.36101939589240573, -12.43898124111679948, 60.96000069308703928 ) ) ;
#30827 = ORIENTED_EDGE ( 'NONE', *, *, #35148, .F. ) ;
#30828 = CARTESIAN_POINT ( 'NONE',  ( -20.99769161626881697, -21.34631032816609064, 62.29284164739992491 ) ) ;
#30829 = CIRCLE ( 'NONE', #23765, 0.6570903894995150374 ) ;
#30830 = CARTESIAN_POINT ( 'NONE',  ( -16.29760673242258306, -22.17363489859456038, 61.87072740723333197 ) ) ;
#30831 = CARTESIAN_POINT ( 'NONE',  ( -20.86784385759799321, -9.357632978295830739, 49.97845033065684106 ) ) ;
#30832 = DIRECTION ( 'NONE',  ( 1.000000000000000000, 0.000000000000000000, 0.000000000000000000 ) ) ;
#30833 = CARTESIAN_POINT ( 'NONE',  ( -14.28913779072144230, -8.050817036395716997, 67.37479760520351135 ) ) ;
#30834 = CARTESIAN_POINT ( 'NONE',  ( -11.32173637914110742, -11.26291225165672927, 67.76297573134488061 ) ) ;
#30835 = DIRECTION ( 'NONE',  ( 0.000000000000000000, -0.9999954153791273948, -0.003028072113819836944 ) ) ;
#30836 = EDGE_LOOP ( 'NONE', ( #34365, #44081, #27833, #23 ) ) ;
#30837 = CARTESIAN_POINT ( 'NONE',  ( -24.39508262754368317, -15.44650746503438654, 73.07591740786084245 ) ) ;
#30838 = VECTOR ( 'NONE', #11177, 1000.000000000000114 ) ;
#30839 = CARTESIAN_POINT ( 'NONE',  ( -22.86572475812252847, -14.01004878893095196, 54.07175714974878389 ) ) ;
#30840 = CARTESIAN_POINT ( 'NONE',  ( -15.03931914688375571, -19.48631565075837457, 50.77966884056656482 ) ) ;
#30841 = CARTESIAN_POINT ( 'NONE',  ( -21.03507683653377924, -21.32559370058661585, 62.26471398792010348 ) ) ;
#30842 = CARTESIAN_POINT ( 'NONE',  ( -12.36648897341435749, -9.886239853951966694, 64.17347106801278755 ) ) ;
#30843 = CARTESIAN_POINT ( 'NONE',  ( -14.80261111872947133, -21.30118156454888734, 61.70770622945212125 ) ) ;
#30845 = ORIENTED_EDGE ( 'NONE', *, *, #47908, .T. ) ;
#30844 = EDGE_CURVE ( 'NONE', #31661, #37124, #42882, .T. ) ;
#30846 = ORIENTED_EDGE ( 'NONE', *, *, #5904, .F. ) ;
#30847 =( NAMED_UNIT ( * ) SI_UNIT ( $, .STERADIAN. ) SOLID_ANGLE_UNIT ( ) );
#30848 = ORIENTED_EDGE ( 'NONE', *, *, #48070, .F. ) ;
#30849 = EDGE_CURVE ( 'NONE', #40867, #23333, #17780, .T. ) ;
#30850 = ADVANCED_FACE ( 'NONE', ( #5459 ), #9391, .T. ) ;
#30851 = EDGE_CURVE ( 'NONE', #25136, #17454, #28817, .T. ) ;
#30852 = PLANE ( 'NONE',  #10697 ) ;
#30853 = AXIS2_PLACEMENT_3D ( 'NONE', #40992, #19309, #7274 ) ;
#30854 = CARTESIAN_POINT ( 'NONE',  ( -17.42409385541299471, -14.80920654474435594, 52.02966884056656482 ) ) ;
#30855 = ORIENTED_EDGE ( 'NONE', *, *, #38370, .T. ) ;
#30856 = CARTESIAN_POINT ( 'NONE',  ( -16.23868518553448936, -7.453991501053678803, 60.32311612641502307 ) ) ;
#30857 = CARTESIAN_POINT ( 'NONE',  ( -13.70631631145106155, -20.74045196213498343, 64.98628931290484445 ) ) ;
#30858 = CARTESIAN_POINT ( 'NONE',  ( -17.18480517372767125, -21.85814792571105514, 72.05054515682328997 ) ) ;
#30859 = ORIENTED_EDGE ( 'NONE', *, *, #45036, .T. ) ;
#30860 = CARTESIAN_POINT ( 'NONE',  ( -23.16117746674104438, -18.90708040007733359, 62.63934749780565880 ) ) ;
#30861 = CARTESIAN_POINT ( 'NONE',  ( -24.22092373047179947, -12.93688097883364208, 66.30246741375938768 ) ) ;
#30862 = ORIENTED_EDGE ( 'NONE', *, *, #8626, .F. ) ;
#30863 = CARTESIAN_POINT ( 'NONE',  ( -45.92409385541306932, -12.76354662275040042, 70.50000000000000000 ) ) ;
#30864 = CARTESIAN_POINT ( 'NONE',  ( -12.20856039377037128, -20.12912213554072238, 64.97400716046928437 ) ) ;
#30865 = EDGE_LOOP ( 'NONE', ( #11520, #10473 ) ) ;
#30866 = LINE ( 'NONE', #1051, #29164 ) ;
#30867 = CARTESIAN_POINT ( 'NONE',  ( -24.01421620325079331, -12.44888360987459741, 73.31513625682875102 ) ) ;
#30868 = ORIENTED_EDGE ( 'NONE', *, *, #8780, .T. ) ;
#30869 = CARTESIAN_POINT ( 'NONE',  ( -23.24383905832493014, -10.15805014756499070, 63.17211752265900060 ) ) ;
#30870 = EDGE_CURVE ( 'NONE', #7306, #27306, #47136, .T. ) ;
#30871 = CARTESIAN_POINT ( 'NONE',  ( -16.29155950929526497, -19.35680461458998636, 49.52966884056656482 ) ) ;
#30872 = FACE_OUTER_BOUND ( 'NONE', #34690, .T. ) ;
#30873 = CARTESIAN_POINT ( 'NONE',  ( -24.36630790243135181, -13.91161852910999031, 73.23157508594482579 ) ) ;
#30874 = CARTESIAN_POINT ( 'NONE',  ( -11.29134393598116937, -11.33126488396075260, 64.16354160640879911 ) ) ;
#30875 = CARTESIAN_POINT ( 'NONE',  ( -46.47622156840087371, -14.20920654474410760, 70.13000000000000966 ) ) ;
#30876 = DIRECTION ( 'NONE',  ( -3.071710424422018668E-17, 6.404604876783312462E-16, 1.000000000000000000 ) ) ;
#30877 = FACE_OUTER_BOUND ( 'NONE', #19208, .T. ) ;
#30878 = CARTESIAN_POINT ( 'NONE',  ( -18.41784385650552736, -9.790100578890868377, 49.79778022625163203 ) ) ;
#30879 = ORIENTED_EDGE ( 'NONE', *, *, #21294, .F. ) ;
#30880 = ADVANCED_FACE ( 'NONE', ( #35473 ), #2229, .F. ) ;
#30881 = LINE ( 'NONE', #45894, #24355 ) ;
#30882 = CARTESIAN_POINT ( 'NONE',  ( -10.47696978178682414, -17.50027494739433820, 64.80456292574326937 ) ) ;
#30883 = ORIENTED_EDGE ( 'NONE', *, *, #9495, .F. ) ;
#30884 = DIRECTION ( 'NONE',  ( -0.3303050442826436783, 0.9438742382973703826, 3.829623549872328964E-09 ) ) ;
#30885 = CARTESIAN_POINT ( 'NONE',  ( -10.62494255334146231, -17.85455924901271629, 71.76706980444858175 ) ) ;
#30886 = PLANE ( 'NONE',  #10908 ) ;
#30887 = CARTESIAN_POINT ( 'NONE',  ( -13.47245400663725690, -21.12492667118925382, 65.10133491818508844 ) ) ;
#30888 =( BOUNDED_CURVE ( )  B_SPLINE_CURVE ( 3, ( #44224, #2347, #25250, #17357 ),
 .UNSPECIFIED., .F., .F. ) 
 B_SPLINE_CURVE_WITH_KNOTS ( ( 4, 4 ),
 ( 0.4074455897393634562, 0.5000000000000000000 ),
 .UNSPECIFIED. ) 
 CURVE ( )  GEOMETRIC_REPRESENTATION_ITEM ( )  RATIONAL_B_SPLINE_CURVE ( ( 0.6983129098261030565, 0.7760317562607105257, 0.8765941196520107281, 1.000000000000005995 ) ) 
 REPRESENTATION_ITEM ( '' )  );
#30889 = EDGE_LOOP ( 'NONE', ( #45044, #26998 ) ) ;
#30890 = FACE_OUTER_BOUND ( 'NONE', #27184, .T. ) ;
#30891 = CARTESIAN_POINT ( 'NONE',  ( -11.96084906401204506, -9.743958800322932490, 60.74413413563605957 ) ) ;
#30892 = ORIENTED_EDGE ( 'NONE', *, *, #4007, .F. ) ;
#30893 = CARTESIAN_POINT ( 'NONE',  ( -24.17899325218984785, -11.66673737571591296, 59.66731058339561855 ) ) ;
#30894 = DIRECTION ( 'NONE',  ( 0.000000000000000000, 1.000000000000000000, -0.000000000000000000 ) ) ;
#30895 = B_SPLINE_CURVE_WITH_KNOTS ( 'NONE', 1,
 ( #29766, #40838 ),
 .UNSPECIFIED., .F., .F.,
 ( 2, 2 ),
 ( 0.000000000000000000, 1.000000000000000000 ),
 .UNSPECIFIED. ) ;
#30896 = CARTESIAN_POINT ( 'NONE',  ( -16.59284385759799108, -8.630756214087126565, 51.74842643355248129 ) ) ;
#30897 = DIRECTION ( 'NONE',  ( 1.224646799147353207E-16, 1.000000000000000000, -1.912410701131276611E-32 ) ) ;
#30898 =( BOUNDED_CURVE ( )  B_SPLINE_CURVE ( 3, ( #26647, #41908, #34254, #41662 ),
 .UNSPECIFIED., .F., .F. ) 
 B_SPLINE_CURVE_WITH_KNOTS ( ( 4, 4 ),
 ( 0.000000000000000000, 0.4074455897393689519 ),
 .UNSPECIFIED. ) 
 CURVE ( )  GEOMETRIC_REPRESENTATION_ITEM ( )  RATIONAL_B_SPLINE_CURVE ( ( 1.000000000000000000, 0.4567392136813275272, 0.3561768502900286570, 0.6983129098261033896 ) ) 
 REPRESENTATION_ITEM ( '' )  );
#30899 = VERTEX_POINT ( 'NONE', #13540 ) ;
#30900 = ORIENTED_EDGE ( 'NONE', *, *, #28571, .F. ) ;
#30901 = CARTESIAN_POINT ( 'NONE',  ( -22.86159385541304090, -7.228003583438117552, 51.38655588711986155 ) ) ;
#30902 = ADVANCED_FACE ( 'NONE', ( #9871 ), #32286, .T. ) ;
#30903 = EDGE_CURVE ( 'NONE', #6216, #36884, #17460, .T. ) ;
#30904 = CARTESIAN_POINT ( 'NONE',  ( -17.23552066371262725, -19.49191114800217406, 49.52966884056656482 ) ) ;
#30905 = CARTESIAN_POINT ( 'NONE',  ( -24.72409385541305582, -14.80920654474413745, 60.01764705882352047 ) ) ;
#30906 = CARTESIAN_POINT ( 'NONE',  ( -20.50783493979771421, -8.027295371342848540, 66.96599508560271374 ) ) ;
#30907 =( BOUNDED_SURFACE ( )  B_SPLINE_SURFACE ( 3, 1, ( 
 ( #3337, #11456 ),
 ( #34335, #41014 ),
 ( #33596, #15133 ),
 ( #387, #22057 ),
 ( #37290, #41495 ),
 ( #33347, #26479 ),
 ( #623, #7296 ) ),
 .UNSPECIFIED., .T., .F., .F. ) 
 B_SPLINE_SURFACE_WITH_KNOTS ( ( 4, 3, 4 ),
 ( 2, 2 ),
 ( 0.000000000000000000, 0.5000000000000000000, 1.000000000000000000 ),
 ( 0.000000000000000000, 1.000000000000000000 ),
 .UNSPECIFIED. ) 
 GEOMETRIC_REPRESENTATION_ITEM ( )  RATIONAL_B_SPLINE_SURFACE ( (
 ( 1.000000000000000000, 1.000000000000000000),
 ( 0.3333333333333335369, 0.3333333333333330373),
 ( 0.3333333333333335369, 0.3333333333333330373),
 ( 1.000000000000000000, 1.000000000000000000),
 ( 0.3333333333333333703, 0.3333333333333333703),
 ( 0.3333333333333333703, 0.3333333333333333703),
 ( 1.000000000000000000, 1.000000000000000000) ) ) 
 REPRESENTATION_ITEM ( '' )  SURFACE ( )  );
#30908 = EDGE_CURVE ( 'NONE', #37344, #21796, #3695, .T. ) ;
#30909 = ADVANCED_FACE ( 'NONE', ( #9644 ), #28586, .T. ) ;
#30910 = DIRECTION ( 'NONE',  ( 0.9986807914369957295, -0.05134858142905001505, 1.286972170232539807E-09 ) ) ;
#30911 = FACE_OUTER_BOUND ( 'NONE', #19702, .T. ) ;
#30912 = CARTESIAN_POINT ( 'NONE',  ( -20.06975372951847447, -8.274133229585533655, 73.73568642813194174 ) ) ;
#30913 = CARTESIAN_POINT ( 'NONE',  ( 18.87590614458706995, 1.878653161019418816, 52.23023769833749697 ) ) ;
#30914 = ORIENTED_EDGE ( 'NONE', *, *, #15800, .F. ) ;
#30915 = CARTESIAN_POINT ( 'NONE',  ( -22.34470984022960138, -19.78791505225649416, 69.17417989488706098 ) ) ;
#30916 = CARTESIAN_POINT ( 'NONE',  ( -24.26646706006808429, -13.09550643046007679, 59.36267627158827764 ) ) ;
#30917 = VERTEX_POINT ( 'NONE', #39660 ) ;
#30918 = DIRECTION ( 'NONE',  ( 0.000000000000000000, 1.000000000000000000, -0.000000000000000000 ) ) ;
#30919 = CARTESIAN_POINT ( 'NONE',  ( -17.42409385541299471, -14.80920654474434883, 62.02966884056656482 ) ) ;
#30920 = ORIENTED_EDGE ( 'NONE', *, *, #41119, .T. ) ;
#30921 = CARTESIAN_POINT ( 'NONE',  ( -12.40538999107997498, -20.31523868419091272, 68.52152871938794476 ) ) ;
#30922 = EDGE_CURVE ( 'NONE', #545, #13505, #43612, .T. ) ;
#30923 = EDGE_LOOP ( 'NONE', ( #37733, #30402, #21169, #35687 ) ) ;
#30924 = CARTESIAN_POINT ( 'NONE',  ( -18.25645571269274825, -21.81792545032241293, 62.03103110229211836 ) ) ;
#30925 = CARTESIAN_POINT ( 'NONE',  ( -20.17268404433175633, -8.371407854712250796, 70.55100341248845552 ) ) ;
#30926 = CARTESIAN_POINT ( 'NONE',  ( -20.86898800509773011, -8.203323387673732370, 59.97978722081754199 ) ) ;
#30927 = ORIENTED_EDGE ( 'NONE', *, *, #25971, .F. ) ;
#30928 = DIRECTION ( 'NONE',  ( -4.267285103686820140E-17, 1.935130192142698484E-16, 1.000000000000000000 ) ) ;
#30929 = CYLINDRICAL_SURFACE ( 'NONE', #678, 1.249999999999998668 ) ;
#30930 = CARTESIAN_POINT ( 'NONE',  ( -17.42409385541299471, -14.80920654474435771, 49.52966884056655772 ) ) ;
#30931 = CARTESIAN_POINT ( 'NONE',  ( -12.74698474939898318, -12.42443183621510094, 50.77966884056655772 ) ) ;
#30932 = PRODUCT_CONTEXT ( 'NONE', #8652, 'mechanical' ) ;
#30933 = CARTESIAN_POINT ( 'NONE',  ( -22.11655536972627090, -20.00359415806959618, 62.51973814734046186 ) ) ;
#30934 = CARTESIAN_POINT ( 'NONE',  ( -10.55057756800719737, -16.13619752454317791, 71.46367081720265446 ) ) ;
#30935 = AXIS2_PLACEMENT_3D ( 'NONE', #29874, #33283, #21992 ) ;
#30936 = DIRECTION ( 'NONE',  ( -2.515467001362780054E-08, -7.569581535656660169E-10, 0.9999999999999996669 ) ) ;
#30937 = ORIENTED_EDGE ( 'NONE', *, *, #39967, .F. ) ;
#30938 = FACE_OUTER_BOUND ( 'NONE', #22240, .T. ) ;
#30939 = ORIENTED_EDGE ( 'NONE', *, *, #19621, .F. ) ;
#30940 = FACE_OUTER_BOUND ( 'NONE', #8886, .T. ) ;
#30941 = CARTESIAN_POINT ( 'NONE',  ( -22.93319280244040570, -10.48995202115733605, 63.35569470095123279 ) ) ;
#30942 = ORIENTED_EDGE ( 'NONE', *, *, #24490, .F. ) ;
#30943 = DIRECTION ( 'NONE',  ( -0.000000000000000000, -1.000000000000000000, -0.000000000000000000 ) ) ;
#30944 = FACE_BOUND ( 'NONE', #33424, .T. ) ;
#30945 = ORIENTED_EDGE ( 'NONE', *, *, #24625, .F. ) ;
#30946 = ORIENTED_EDGE ( 'NONE', *, *, #14278, .T. ) ;
#30947 = ORIENTED_EDGE ( 'NONE', *, *, #13703, .T. ) ;
#30948 = CARTESIAN_POINT ( 'NONE',  ( -17.98584054083101691, -22.23808389992613499, 62.06031238270200845 ) ) ;
#30949 = LINE ( 'NONE', #19864, #27426 ) ;
#30950 = CARTESIAN_POINT ( 'NONE',  ( -20.48780003469585154, -11.24700778661463829, 49.52966884056655772 ) ) ;
#30951 = CARTESIAN_POINT ( 'NONE',  ( -14.48363552191318604, -8.456628570761285602, 67.25975083097569041 ) ) ;
#30952 = CARTESIAN_POINT ( 'NONE',  ( -11.86838291625971742, -9.845553222893467904, 64.14418898700822069 ) ) ;
#30953 = CARTESIAN_POINT ( 'NONE',  ( -19.36486170040678090, -8.083171235113246311, 60.24476463208835497 ) ) ;
#30954 = ORIENTED_EDGE ( 'NONE', *, *, #10376, .T. ) ;
#30955 = VERTEX_POINT ( 'NONE', #39901 ) ;
#30956 = CARTESIAN_POINT ( 'NONE',  ( -21.54284385650551670, -8.811426318492348031, 52.18089403414751359 ) ) ;
#30957 = EDGE_CURVE ( 'NONE', #2110, #41320, #47540, .T. ) ;
#30958 = CARTESIAN_POINT ( 'NONE',  ( -11.86269392149798207, -9.851982632420845931, 64.22252622837828540 ) ) ;
#30959 = DIRECTION ( 'NONE',  ( 0.2664710960620865210, -0.9638429098994647504, 4.833213314675751572E-08 ) ) ;
#30960 = CARTESIAN_POINT ( 'NONE',  ( -20.60788153932096023, -8.518722016582882972, 63.32593600985608617 ) ) ;
#30961 = EDGE_LOOP ( 'NONE', ( #296, #47310, #2773, #27034 ) ) ;
#30962 = CARTESIAN_POINT ( 'NONE',  ( -15.66159385650551705, -9.295667164867525756, 49.30633214617472504 ) ) ;
#30964 = ORIENTED_EDGE ( 'NONE', *, *, #44965, .F. ) ;
#30963 = EDGE_CURVE ( 'NONE', #16796, #41098, #20478, .T. ) ;
#30965 = FACE_OUTER_BOUND ( 'NONE', #34396, .T. ) ;
#30966 = CIRCLE ( 'NONE', #33279, 4.686499999999999666 ) ;
#30967 = EDGE_CURVE ( 'NONE', #45444, #44359, #4843, .T. ) ;
#30968 = DIRECTION ( 'NONE',  ( -5.731567514496413899E-31, -1.020425574103664789E-16, -1.000000000000000000 ) ) ;
#30969 = ADVANCED_FACE ( 'NONE', ( #18952 ), #41352, .T. ) ;
#30970 = ORIENTED_EDGE ( 'NONE', *, *, #25020, .F. ) ;
#30971 = FACE_OUTER_BOUND ( 'NONE', #23363, .T. ) ;
#30972 = CARTESIAN_POINT ( 'NONE',  ( -10.42773860147015519, -14.58150043490377179, 67.87302585467796234 ) ) ;
#30973 = DIRECTION ( 'NONE',  ( 0.9687793358424819923, -0.2479245821708678243, 0.000000000000000000 ) ) ;
#30974 = ORIENTED_EDGE ( 'NONE', *, *, #34639, .T. ) ;
#30975 = CARTESIAN_POINT ( 'NONE',  ( -15.15107538838304002, -21.43001499838511847, 65.40596678908117667 ) ) ;
#30976 = CARTESIAN_POINT ( 'NONE',  ( -17.06206538396918404, -7.760525543569854356, 67.17606901500077754 ) ) ;
#30977 = CARTESIAN_POINT ( 'NONE',  ( -11.39842353126723218, -18.37420439508194647, 61.50540784843255437 ) ) ;
#30978 = EDGE_LOOP ( 'NONE', ( #36556, #10389 ) ) ;
#30979 = FACE_OUTER_BOUND ( 'NONE', #33129, .T. ) ;
#30980 = ORIENTED_EDGE ( 'NONE', *, *, #44320, .T. ) ;
#30981 = CARTESIAN_POINT ( 'NONE',  ( -19.18081468460184524, -7.569236297829234239, 63.53750910235358873 ) ) ;
#30982 = CARTESIAN_POINT ( 'NONE',  ( -15.28630342961327138, -8.082779564739171363, 56.99432743296591042 ) ) ;
#30983 = ORIENTED_EDGE ( 'NONE', *, *, #48669, .F. ) ;
#30984 = CARTESIAN_POINT ( 'NONE',  ( -10.90759836534377492, -17.49952001658422063, 68.39721944423101263 ) ) ;
#30985 = DIRECTION ( 'NONE',  ( 1.000000000000000000, 2.866981220435666553E-17, 0.000000000000000000 ) ) ;
#30986 = CARTESIAN_POINT ( 'NONE',  ( -14.23218538299976643, -8.077567926792571740, 67.36636790937856745 ) ) ;
#30987 = ORIENTED_EDGE ( 'NONE', *, *, #46542, .F. ) ;
#30988 = CARTESIAN_POINT ( 'NONE',  ( -13.50190746284422794, -17.39609839546894676, 49.52966884056655772 ) ) ;
#30989 = CARTESIAN_POINT ( 'NONE',  ( -20.96474559848019226, -20.91483931500396309, 58.80042297414523489 ) ) ;
#30990 = CARTESIAN_POINT ( 'NONE',  ( -14.01118748589247964, -10.49619482288619565, 53.49899999999994549 ) ) ;
#30991 = CARTESIAN_POINT ( 'NONE',  ( -11.95607289622835978, -9.749060919267328984, 60.68105355187064021 ) ) ;
#30992 = VERTEX_POINT ( 'NONE', #3685 ) ;
#30993 = CARTESIAN_POINT ( 'NONE',  ( -11.43875873011815258, -18.53463696397233207, 61.57710806188755015 ) ) ;
#30994 = DIRECTION ( 'NONE',  ( -1.000000000000000000, 4.164305804376849172E-17, -1.614929280266638808E-16 ) ) ;
#30995 = ORIENTED_EDGE ( 'NONE', *, *, #26264, .F. ) ;
#30996 = ORIENTED_EDGE ( 'NONE', *, *, #46225, .F. ) ;
#30997 = CARTESIAN_POINT ( 'NONE',  ( -22.78465755717926555, -10.30744034590000346, 66.84182281441593432 ) ) ;
#30998 = CARTESIAN_POINT ( 'NONE',  ( -10.54994933093899867, -13.24305344519376959, 71.49356453765415154 ) ) ;
#30999 = CYLINDRICAL_SURFACE ( 'NONE', #3662, 0.4000000000000011879 ) ;
#31000 = CARTESIAN_POINT ( 'NONE',  ( -21.23034385650552025, -9.794322478646142471, 51.19202720610083901 ) ) ;
#31001 = CARTESIAN_POINT ( 'NONE',  ( -12.43058792219793141, -16.43013174195301218, 50.77966884056655772 ) ) ;
#31002 = EDGE_CURVE ( 'NONE', #48717, #31810, #3074, .T. ) ;
#31003 = CARTESIAN_POINT ( 'NONE',  ( -11.89178903705324863, -10.43929771899554737, 71.26893105542536944 ) ) ;
#31004 = PLANE ( 'NONE',  #47543 ) ;
#31005 = CARTESIAN_POINT ( 'NONE',  ( -10.53028993777715883, -16.28642212234895226, 71.73278239416407587 ) ) ;
#31006 = VERTEX_POINT ( 'NONE', #21911 ) ;
#31007 = ORIENTED_EDGE ( 'NONE', *, *, #10375, .T. ) ;
#31008 = CARTESIAN_POINT ( 'NONE',  ( -22.98758735661991892, -9.854289139077749837, 70.26824437992965500 ) ) ;
#31009 =( LENGTH_UNIT ( ) NAMED_UNIT ( * ) SI_UNIT ( .MILLI., .METRE. ) );
#31010 = CARTESIAN_POINT ( 'NONE',  ( -14.54176669294802693, -21.67913874359843973, 58.28122557424108408 ) ) ;
#31011 = CARTESIAN_POINT ( 'NONE',  ( -17.42409385541299471, -14.80920654474435771, 49.52966884056655772 ) ) ;
#31012 = CARTESIAN_POINT ( 'NONE',  ( -18.83428564917659287, -7.493810079819247072, 70.62713979963420741 ) ) ;
#31013 = VERTEX_POINT ( 'NONE', #44338 ) ;
#31014 = ORIENTED_EDGE ( 'NONE', *, *, #12454, .T. ) ;
#31015 = DIRECTION ( 'NONE',  ( 3.071710424422018668E-17, -6.404604876783312462E-16, -1.000000000000000000 ) ) ;
#31016 = CARTESIAN_POINT ( 'NONE',  ( -10.53692143227921818, -11.79390935372226323, 53.76227901944321985 ) ) ;
#31017 = EDGE_CURVE ( 'NONE', #32391, #37778, #46535, .T. ) ;
#31018 = CARTESIAN_POINT ( 'NONE',  ( -14.92237289681681034, -21.82673989507453882, 65.22879770143127587 ) ) ;
#31019 = DIRECTION ( 'NONE',  ( -0.9796876409582463419, 0.2005296141562636081, 7.890952370353029293E-08 ) ) ;
#31020 = ADVANCED_FACE ( 'NONE', ( #257 ), #33212, .T. ) ;
#31021 =( BOUNDED_CURVE ( )  B_SPLINE_CURVE ( 3, ( #25278, #20852, #1894, #35851 ),
 .UNSPECIFIED., .F., .F. ) 
 B_SPLINE_CURVE_WITH_KNOTS ( ( 4, 4 ),
 ( 0.9074455897393649551, 1.000000000000000000 ),
 .UNSPECIFIED. ) 
 CURVE ( )  GEOMETRIC_REPRESENTATION_ITEM ( )  RATIONAL_B_SPLINE_CURVE ( ( 0.6983129098260929535, 0.7760317562606982023, 0.8765941196520005141, 1.000000000000000000 ) ) 
 REPRESENTATION_ITEM ( '' )  );
#31022 = ORIENTED_EDGE ( 'NONE', *, *, #16207, .F. ) ;
#31023 = CARTESIAN_POINT ( 'NONE',  ( -10.55755145186731880, -16.16957250319292072, 68.16870912284423412 ) ) ;
#31024 = CIRCLE ( 'NONE', #34915, 2.000000000000000444 ) ;
#31025 = EDGE_CURVE ( 'NONE', #18851, #48127, #9041, .T. ) ;
#31026 = CARTESIAN_POINT ( 'NONE',  ( -17.42409385541299471, -14.80920654474435771, 49.52966884056655772 ) ) ;
#31027 = VECTOR ( 'NONE', #8888, 1000.000000000000000 ) ;
#31028 = ORIENTED_EDGE ( 'NONE', *, *, #30212, .T. ) ;
#31029 = FACE_OUTER_BOUND ( 'NONE', #39264, .T. ) ;
#31030 = EDGE_CURVE ( 'NONE', #44219, #6337, #45790, .T. ) ;
#31031 = CARTESIAN_POINT ( 'NONE',  ( -13.89433361489564156, -8.703010632355098863, 74.08466061421664506 ) ) ;
#31032 = ORIENTED_EDGE ( 'NONE', *, *, #15801, .T. ) ;
#31034 = ADVANCED_FACE ( 'NONE', ( #48017 ), #37149, .T. ) ;
#31033 = CARTESIAN_POINT ( 'NONE',  ( -23.65353884516659733, -18.89565076926976062, 69.43338659176652072 ) ) ;
#31035 =( BOUNDED_SURFACE ( )  B_SPLINE_SURFACE ( 3, 1, ( 
 ( #23378, #31249 ),
 ( #19688, #1444 ),
 ( #26838, #34699 ),
 ( #42337, #8858 ),
 ( #973, #46033 ),
 ( #38879, #31012 ),
 ( #15969, #12290 ) ),
 .UNSPECIFIED., .T., .F., .F. ) 
 B_SPLINE_SURFACE_WITH_KNOTS ( ( 4, 3, 4 ),
 ( 2, 2 ),
 ( 0.000000000000000000, 0.5000000000000000000, 1.000000000000000000 ),
 ( 0.000000000000000000, 1.000000000000000000 ),
 .UNSPECIFIED. ) 
 GEOMETRIC_REPRESENTATION_ITEM ( )  RATIONAL_B_SPLINE_SURFACE ( (
 ( 1.000000000000000000, 1.000000000000000000),
 ( 0.3333333333333335369, 0.3333333333333330373),
 ( 0.3333333333333335369, 0.3333333333333330373),
 ( 1.000000000000000000, 1.000000000000000000),
 ( 0.3333333333333333703, 0.3333333333333333703),
 ( 0.3333333333333333703, 0.3333333333333333703),
 ( 1.000000000000000000, 1.000000000000000000) ) ) 
 REPRESENTATION_ITEM ( '' )  SURFACE ( )  );
#31036 = ORIENTED_EDGE ( 'NONE', *, *, #45240, .T. ) ;
#31037 = FACE_OUTER_BOUND ( 'NONE', #6746, .T. ) ;
#31038 = DIRECTION ( 'NONE',  ( 0.9294853595766545684, 0.3688590060343616139, 0.000000000000000000 ) ) ;
#31039 = VERTEX_POINT ( 'NONE', #3437 ) ;
#31040 = CARTESIAN_POINT ( 'NONE',  ( -24.01844669341070926, -17.32505205508840262, 62.62928254837112974 ) ) ;
#31041 = CARTESIAN_POINT ( 'NONE',  ( -17.42409385541299471, -14.80920654474435594, 52.02966884056656482 ) ) ;
#31042 = CARTESIAN_POINT ( 'NONE',  ( -18.44909385650551670, -8.104110260919579645, 48.81699501597546487 ) ) ;
#31043 = CARTESIAN_POINT ( 'NONE',  ( -21.38436113231072966, -21.11942757641454094, 69.25461391254337684 ) ) ;
#31044 = CARTESIAN_POINT ( 'NONE',  ( -22.21294348278119912, -9.102026181049186704, 59.86024708057400545 ) ) ;
#31045 = CARTESIAN_POINT ( 'NONE',  ( -21.73662441638723308, -9.231682010981758779, 66.67622112302015580 ) ) ;
#31046 = ORIENTED_EDGE ( 'NONE', *, *, #11857, .F. ) ;
#31047 = DIRECTION ( 'NONE',  ( 0.8810891847886932471, 0.4615090133018354690, 0.1033986416233890065 ) ) ;
#31048 = CARTESIAN_POINT ( 'NONE',  ( -16.22409385541304871, -9.359200813967568422, 50.49621490985801842 ) ) ;
#31049 = CARTESIAN_POINT ( 'NONE',  ( -14.94170459844064780, -18.78425696289860269, 52.02966884056656482 ) ) ;
#31050 = CARTESIAN_POINT ( 'NONE',  ( -24.76413943691219899, -16.08518182373101624, 66.18608065020819708 ) ) ;
#31051 = ORIENTED_EDGE ( 'NONE', *, *, #43585, .F. ) ;
#31052 = VERTEX_POINT ( 'NONE', #48490 ) ;
#31053 = LINE ( 'NONE', #42636, #45595 ) ;
#31054 = CARTESIAN_POINT ( 'NONE',  ( -24.33896800083871526, -16.20181617365279791, 66.36325218972963569 ) ) ;
#31055 = VERTEX_POINT ( 'NONE', #18205 ) ;
#31056 = LINE ( 'NONE', #5199, #2120 ) ;
#31057 = DIRECTION ( 'NONE',  ( 0.9687793358424817702, -0.2479245821708684350, 0.000000000000000000 ) ) ;
#31058 = CARTESIAN_POINT ( 'NONE',  ( -10.28759036655602976, -12.67074725465185203, 64.36861864226402474 ) ) ;
#31059 = CARTESIAN_POINT ( 'NONE',  ( -18.72681101482837818, -7.880611649715417499, 70.37068030201731972 ) ) ;
#31060 = EDGE_CURVE ( 'NONE', #11637, #29328, #15918, .T. ) ;
#31061 = FACE_OUTER_BOUND ( 'NONE', #33964, .T. ) ;
#31062 = CARTESIAN_POINT ( 'NONE',  ( -15.82706267189338689, -7.992506172297358269, 70.83819797924105899 ) ) ;
#31063 = CARTESIAN_POINT ( 'NONE',  ( 10.57590614458695377, 1.890747609047612521, 50.53028072113853142 ) ) ;
#31064 = VECTOR ( 'NONE', #25312, 1000.000000000000000 ) ;
#31065 = EDGE_LOOP ( 'NONE', ( #12966, #23435 ) ) ;
#31066 = CARTESIAN_POINT ( 'NONE',  ( -22.48562329102781021, -19.71690596984645438, 72.64960304871698327 ) ) ;
#31067 = DIRECTION ( 'NONE',  ( -3.071710424422018668E-17, 6.404604876783312462E-16, 1.000000000000000000 ) ) ;
#31068 = CARTESIAN_POINT ( 'NONE',  ( -14.11566384109317873, -8.583543149139638118, 74.20514413324690395 ) ) ;
#31069 = ADVANCED_FACE ( 'NONE', ( #33701 ), #30053, .T. ) ;
#31070 = ORIENTED_EDGE ( 'NONE', *, *, #15183, .T. ) ;
#31071 = EDGE_LOOP ( 'NONE', ( #7175, #8346, #15840, #20562, #3377 ) ) ;
#31072 = B_SPLINE_CURVE_WITH_KNOTS ( 'NONE', 3,
 ( #15410, #22845, #42273, #431, #37838, #4132, #8537, #23566, #22583, #19869 ),
 .UNSPECIFIED., .F., .F.,
 ( 4, 2, 2, 2, 4 ),
 ( 0.1272669073658287964, 0.2522669073463161826, 0.3772669073268035689, 0.5022669073072909551, 0.6272669072877783414 ),
 .UNSPECIFIED. ) ;
#31073 = EDGE_LOOP ( 'NONE', ( #9214, #38659, #29801, #25334 ) ) ;
#31074 = CARTESIAN_POINT ( 'NONE',  ( -11.14016733508048240, -18.81244675540447631, 64.93362470803228348 ) ) ;
#31075 = VERTEX_POINT ( 'NONE', #25601 ) ;
#31076 = CARTESIAN_POINT ( 'NONE',  ( -10.43244321615298809, -14.46516663507775213, 68.15800133269522121 ) ) ;
#31077 = ADVANCED_FACE ( 'NONE', ( #45312 ), #14723, .T. ) ;
#31078 = DIRECTION ( 'NONE',  ( -0.3478314405900310158, -0.9375570856950865561, 1.977132801529374134E-16 ) ) ;
#31079 = ORIENTED_EDGE ( 'NONE', *, *, #24296, .F. ) ;
#31080 = EDGE_CURVE ( 'NONE', #46754, #2300, #4792, .T. ) ;
#31081 = CARTESIAN_POINT ( 'NONE',  ( -13.83108396514174565, -21.33561889020367630, 72.04112409899799729 ) ) ;
#31082 = EDGE_CURVE ( 'NONE', #39506, #17461, #27861, .T. ) ;
#31083 = CARTESIAN_POINT ( 'NONE',  ( -21.63336539757928634, -9.153348366551478321, 66.94677872351418557 ) ) ;
#31084 = ORIENTED_EDGE ( 'NONE', *, *, #13017, .T. ) ;
#31085 = DIRECTION ( 'NONE',  ( 1.927470528863184130E-16, 1.434740771370715221E-29, -1.000000000000000000 ) ) ;
#31086 = B_SPLINE_CURVE_WITH_KNOTS ( 'NONE', 3,
 ( #45945, #12205, #27226, #5308, #42252, #8512, #27466, #42498, #4339, #23544 ),
 .UNSPECIFIED., .F., .F.,
 ( 4, 2, 2, 2, 4 ),
 ( 0.000000000000000000, 0.2500000000000000000, 0.5000000000000000000, 0.7500000000000000000, 1.000000000000000000 ),
 .UNSPECIFIED. ) ;
#31087 = VECTOR ( 'NONE', #43490, 1000.000000000000000 ) ;
#31088 = ORIENTED_EDGE ( 'NONE', *, *, #20495, .F. ) ;
#31089 = CARTESIAN_POINT ( 'NONE',  ( -24.53780051168580911, -12.59584816521350348, 69.95738404390658616 ) ) ;
#31090 = CARTESIAN_POINT ( 'NONE',  ( -17.17561717955991085, -7.363342535065456218, 70.69024626294222458 ) ) ;
#31091 = EDGE_LOOP ( 'NONE', ( #11969, #31446, #6907, #19398, #39399 ) ) ;
#31092 = CARTESIAN_POINT ( 'NONE',  ( -10.43125849979191955, -13.91324152291312188, 57.74825034919034294 ) ) ;
#31093 = AXIS2_PLACEMENT_3D ( 'NONE', #2209, #17219, #39881 ) ;
#31094 = CARTESIAN_POINT ( 'NONE',  ( -13.92409385541305511, -10.10920654474410618, 80.49999999999998579 ) ) ;
#31095 = EDGE_CURVE ( 'NONE', #17746, #21028, #4191, .T. ) ;
#31096 = CARTESIAN_POINT ( 'NONE',  ( -11.60006209888454443, -10.16330164164447325, 71.08397698276321819 ) ) ;
#31097 = CARTESIAN_POINT ( 'NONE',  ( -20.95545100651803594, -20.91135505560678709, 65.59926067308570907 ) ) ;
#31098 = DIRECTION ( 'NONE',  ( 0.8447509909909733938, -0.5351595679979650466, 0.000000000000000000 ) ) ;
#31099 = LINE ( 'NONE', #38724, #15218 ) ;
#31100 = EDGE_CURVE ( 'NONE', #15096, #4739, #23877, .T. ) ;
#31101 = CARTESIAN_POINT ( 'NONE',  ( -14.37682202087475680, -19.38786730597468022, 54.07175714974878389 ) ) ;
#31102 = DIRECTION ( 'NONE',  ( 2.671295499615842957E-06, 1.272698189891367967E-05, 0.9999999999154439712 ) ) ;
#31103 = CARTESIAN_POINT ( 'NONE',  ( -21.01123855637963089, -20.87838213191899683, 65.58453944497207999 ) ) ;
#31104 = EDGE_CURVE ( 'NONE', #43248, #47012, #20961, .T. ) ;
#31105 = EDGE_CURVE ( 'NONE', #8440, #14865, #840, .T. ) ;
#31106 = CARTESIAN_POINT ( 'NONE',  ( -14.53659385650551705, -6.915538690918075382, 49.31353937987644542 ) ) ;
#31107 = ORIENTED_EDGE ( 'NONE', *, *, #18273, .T. ) ;
#31108 = CARTESIAN_POINT ( 'NONE',  ( -21.66487278515026915, -9.172785956992999701, 63.39973619028431528 ) ) ;
#31109 = CARTESIAN_POINT ( 'NONE',  ( -10.45152819156127144, -17.43344342502064848, 64.73465214939118084 ) ) ;
#31110 = ORIENTED_EDGE ( 'NONE', *, *, #3753, .F. ) ;
#31111 = B_SPLINE_CURVE_WITH_KNOTS ( 'NONE', 3,
 ( #20035, #9694, #24711, #12396, #19803, #16074, #34805, #1075, #24475, #5259 ),
 .UNSPECIFIED., .F., .F.,
 ( 4, 2, 2, 2, 4 ),
 ( 0.000000000000000000, 0.2500000000000000000, 0.5000000000000000000, 0.7500000000000000000, 1.000000000000000000 ),
 .UNSPECIFIED. ) ;
#31112 = LINE ( 'NONE', #24213, #14240 ) ;
#31113 = CARTESIAN_POINT ( 'NONE',  ( -21.59804090337381410, -20.98026344205569771, 72.70941702861115630 ) ) ;
#31114 = CARTESIAN_POINT ( 'NONE',  ( -23.26195008415477972, -10.18062560903149638, 63.24998768291849416 ) ) ;
#31115 = DIRECTION ( 'NONE',  ( 1.000000000000000000, 2.866981220435666553E-17, 0.000000000000000000 ) ) ;
#31116 = VERTEX_POINT ( 'NONE', #35173 ) ;
#31117 = CARTESIAN_POINT ( 'NONE',  ( -23.76773515637538736, -11.84597937754909935, 63.06291311429629332 ) ) ;
#31118 = B_SPLINE_CURVE_WITH_KNOTS ( 'NONE', 3,
 ( #39363, #20419, #17171, #27555, #31247, #42595, #31972, #8856, #46989, #39842 ),
 .UNSPECIFIED., .F., .F.,
 ( 4, 2, 2, 2, 4 ),
 ( 0.000000000000000000, 0.2500000000000000000, 0.5000000000000000000, 0.7500000000000000000, 1.000000000000000000 ),
 .UNSPECIFIED. ) ;
#31119 = CARTESIAN_POINT ( 'NONE',  ( -23.99312268326606201, -11.29471679256767125, 66.60709928216182618 ) ) ;
#31120 = VERTEX_POINT ( 'NONE', #20164 ) ;
#31121 = CARTESIAN_POINT ( 'NONE',  ( -17.13503149044196405, -7.764836982087095052, 70.77563787455143540 ) ) ;
#31122 = CARTESIAN_POINT ( 'NONE',  ( -17.42409385541299471, -14.80920654474435771, 49.52966884056655772 ) ) ;
#31123 = CARTESIAN_POINT ( 'NONE',  ( -10.00731251637046881, -14.10555026099538978, 61.10316585833331260 ) ) ;
#31124 = CARTESIAN_POINT ( 'NONE',  ( -16.64909385759798965, -8.112991634885936776, 51.74999426922421719 ) ) ;
#31125 = VERTEX_POINT ( 'NONE', #22911 ) ;
#31126 = EDGE_LOOP ( 'NONE', ( #42745, #46753, #34279, #38086, #24920 ) ) ;
#31127 = CARTESIAN_POINT ( 'NONE',  ( -20.49909385541304374, -8.105421454601382081, 49.25000573077640098 ) ) ;
#31128 = ADVANCED_FACE ( 'NONE', ( #27310 ), #31035, .T. ) ;
#31129 = CARTESIAN_POINT ( 'NONE',  ( -22.99825578621637590, -9.866157890886050552, 70.15145146949444666 ) ) ;
#31130 = CARTESIAN_POINT ( 'NONE',  ( -15.48628188820593543, -7.614865071177022493, 74.26641013817956605 ) ) ;
#31131 = EDGE_CURVE ( 'NONE', #19773, #10407, #21316, .T. ) ;
#31132 = DIRECTION ( 'NONE',  ( 1.224646799147353207E-16, 1.000000000000000000, -1.912410701131276611E-32 ) ) ;
#31133 = CARTESIAN_POINT ( 'NONE',  ( -20.47364665458772848, -8.506973655552112490, 67.00933899976185160 ) ) ;
#31134 = ADVANCED_FACE ( 'NONE', ( #8131 ), #19929, .T. ) ;
#31135 = CARTESIAN_POINT ( 'NONE',  ( -18.85724798917316392, -7.906108138700305155, 67.18599644112759961 ) ) ;
#31136 = CARTESIAN_POINT ( 'NONE',  ( -24.39403741458288266, -17.44049236422942784, 69.52844466935830781 ) ) ;
#31137 = ORIENTED_EDGE ( 'NONE', *, *, #3796, .T. ) ;
#31138 = CARTESIAN_POINT ( 'NONE',  ( -21.25294243521737059, -20.66975681891597816, 72.80829934587789865 ) ) ;
#31139 = CARTESIAN_POINT ( 'NONE',  ( -24.31482381427648676, -13.31912605980313735, 59.36267924676594987 ) ) ;
#31140 = ORIENTED_EDGE ( 'NONE', *, *, #17147, .F. ) ;
#31141 = CARTESIAN_POINT ( 'NONE',  ( -13.31679730094617575, -21.02473588039183028, 61.61672084944926553 ) ) ;
#31142 = CARTESIAN_POINT ( 'NONE',  ( -24.25171796977671335, -16.35308120058899206, 59.42332432118549690 ) ) ;
#31143 = ORIENTED_EDGE ( 'NONE', *, *, #33585, .F. ) ;
#31144 = CARTESIAN_POINT ( 'NONE',  ( -15.39536932222403287, -19.92137602241599836, 53.49899999999994549 ) ) ;
#31145 = CARTESIAN_POINT ( 'NONE',  ( -19.68659385759799108, -7.222650657624104298, 49.61879703869476543 ) ) ;
#31146 =( BOUNDED_CURVE ( )  B_SPLINE_CURVE ( 3, ( #35781, #31861, #46881, #39248 ),
 .UNSPECIFIED., .F., .F. ) 
 B_SPLINE_CURVE_WITH_KNOTS ( ( 4, 4 ),
 ( 1.570796326794896780, 1.675516081914553590 ),
 .UNSPECIFIED. ) 
 CURVE ( )  GEOMETRIC_REPRESENTATION_ITEM ( )  RATIONAL_B_SPLINE_CURVE ( ( 1.000000000000000000, 0.9990863565030492222, 0.9990863565030492222, 1.000000000000000000 ) ) 
 REPRESENTATION_ITEM ( '' )  );
#31147 = CARTESIAN_POINT ( 'NONE',  ( -10.33213862838506891, -12.52699322434005680, 60.92040820086095465 ) ) ;
#31148 = CARTESIAN_POINT ( 'NONE',  ( -10.43125849979191955, -13.91324152291312366, 57.74825034919034294 ) ) ;
#31149 = ORIENTED_EDGE ( 'NONE', *, *, #29602, .F. ) ;
#31150 = CARTESIAN_POINT ( 'NONE',  ( -17.42409385541299471, -14.80920654474435771, 49.52966884056655772 ) ) ;
#31151 = CARTESIAN_POINT ( 'NONE',  ( -20.87508512492161472, -21.41177400750635229, 58.75136860439389608 ) ) ;
#31152 = CARTESIAN_POINT ( 'NONE',  ( -10.89696847888502163, -11.21756741187531681, 64.25543717716909953 ) ) ;
#31153 = EDGE_CURVE ( 'NONE', #25531, #41086, #27767, .T. ) ;
#31154 = VECTOR ( 'NONE', #46882, 1000.000000000000000 ) ;
#31155 = AXIS2_PLACEMENT_3D ( 'NONE', #14427, #36608, #7093 ) ;
#31156 = FACE_BOUND ( 'NONE', #43535, .T. ) ;
#31157 = APPLICATION_PROTOCOL_DEFINITION ( 'draft international standard', 'automotive_design', 1998, #12094 ) ;
#31158 = EDGE_CURVE ( 'NONE', #19353, #40794, #19193, .T. ) ;
#31159 = ADVANCED_FACE ( 'NONE', ( #30538 ), #20680, .T. ) ;
#31160 = LINE ( 'NONE', #16368, #16381 ) ;
#31161 = CARTESIAN_POINT ( 'NONE',  ( -11.40126873537406205, -11.24191379345135999, 60.97885781058090515 ) ) ;
#31162 = B_SPLINE_CURVE_WITH_KNOTS ( 'NONE', 1,
 ( #26535, #7841 ),
 .UNSPECIFIED., .F., .F.,
 ( 2, 2 ),
 ( 0.000000000000000000, 1.000000000000000000 ),
 .UNSPECIFIED. ) ;
#31163 = CARTESIAN_POINT ( 'NONE',  ( -20.01098570613759975, -18.73139293731311383, 49.52966884056656482 ) ) ;
#31164 = ORIENTED_EDGE ( 'NONE', *, *, #5542, .T. ) ;
#31165 = DIRECTION ( 'NONE',  ( 5.551115123125782702E-17, 1.232595164407830946E-32, 1.000000000000000000 ) ) ;
#31166 = VERTEX_POINT ( 'NONE', #43799 ) ;
#31167 = DIRECTION ( 'NONE',  ( 0.8603395911234833493, 0.5097212845717526974, 0.000000000000000000 ) ) ;
#31168 = DIRECTION ( 'NONE',  ( 1.000000000000000000, 0.000000000000000000, -8.260587980841940012E-17 ) ) ;
#31169 = ORIENTED_EDGE ( 'NONE', *, *, #23059, .F. ) ;
#31170 =( BOUNDED_SURFACE ( )  B_SPLINE_SURFACE ( 3, 1, ( 
 ( #41898, #4233 ),
 ( #19974, #37947 ),
 ( #12099, #34975 ),
 ( #11862, #34491 ),
 ( #302, #23429 ),
 ( #778, #15774 ),
 ( #19242, #15521 ) ),
 .UNSPECIFIED., .T., .F., .F. ) 
 B_SPLINE_SURFACE_WITH_KNOTS ( ( 4, 3, 4 ),
 ( 2, 2 ),
 ( 0.000000000000000000, 0.5000000000000000000, 1.000000000000000000 ),
 ( 0.000000000000000000, 1.000000000000000000 ),
 .UNSPECIFIED. ) 
 GEOMETRIC_REPRESENTATION_ITEM ( )  RATIONAL_B_SPLINE_SURFACE ( (
 ( 1.000000000000000000, 1.000000000000000000),
 ( 0.3333333333333335369, 0.3333333333333330373),
 ( 0.3333333333333335369, 0.3333333333333330373),
 ( 1.000000000000000000, 1.000000000000000000),
 ( 0.3333333333333333703, 0.3333333333333333703),
 ( 0.3333333333333333703, 0.3333333333333333703),
 ( 1.000000000000000000, 1.000000000000000000) ) ) 
 REPRESENTATION_ITEM ( '' )  SURFACE ( )  );
#31171 = CARTESIAN_POINT ( 'NONE',  ( -41.03659385541305937, -14.80920654474428666, 74.09999999999998010 ) ) ;
#31172 = ADVANCED_FACE ( 'NONE', ( #39366 ), #1934, .T. ) ;
#31173 = EDGE_CURVE ( 'NONE', #10695, #19831, #16592, .T. ) ;
#31174 = FACE_BOUND ( 'NONE', #18934, .T. ) ;
#31175 = ORIENTED_EDGE ( 'NONE', *, *, #5878, .T. ) ;
#31176 = ORIENTED_EDGE ( 'NONE', *, *, #23504, .F. ) ;
#31177 = EDGE_LOOP ( 'NONE', ( #34044, #20138, #23307, #931 ) ) ;
#31178 = CARTESIAN_POINT ( 'NONE',  ( -17.91451304303208403, -22.24313331792350112, 61.99040607801043734 ) ) ;
#31179 = SURFACE_STYLE_FILL_AREA ( #32350 ) ;
#31180 = CARTESIAN_POINT ( 'NONE',  ( -36.42409385541304800, -9.359200813967566646, 50.49621490985803263 ) ) ;
#31181 = CARTESIAN_POINT ( 'NONE',  ( -22.71059208588729561, -10.14448404190931186, 70.02650598627910483 ) ) ;
#31182 = CARTESIAN_POINT ( 'NONE',  ( -10.72572792941078212, -12.60087465324735945, 64.68324854050578665 ) ) ;
#31183 = CARTESIAN_POINT ( 'NONE',  ( -16.36834455927873222, -22.18410795223847387, 61.94063518049016182 ) ) ;
#31184 =( BOUNDED_CURVE ( )  B_SPLINE_CURVE ( 3, ( #24554, #3081, #39788, #32869 ),
 .UNSPECIFIED., .F., .F. ) 
 B_SPLINE_CURVE_WITH_KNOTS ( ( 4, 4 ),
 ( 0.9074455897393642889, 1.000000000000000000 ),
 .UNSPECIFIED. ) 
 CURVE ( )  GEOMETRIC_REPRESENTATION_ITEM ( )  RATIONAL_B_SPLINE_CURVE ( ( 0.6983129098261030565, 0.7760317562607068620, 0.8765941196520058432, 1.000000000000000000 ) ) 
 REPRESENTATION_ITEM ( '' )  );
#31185 = ORIENTED_EDGE ( 'NONE', *, *, #18456, .T. ) ;
#31186 = ORIENTED_EDGE ( 'NONE', *, *, #32917, .T. ) ;
#31187 = CARTESIAN_POINT ( 'NONE',  ( -21.14909385650551599, -8.104110260919577868, 48.81699501597546487 ) ) ;
#31188 = EDGE_CURVE ( 'NONE', #19518, #18739, #5397, .T. ) ;
#31189 = CARTESIAN_POINT ( 'NONE',  ( -21.06713455244400635, -20.85430592508659586, 72.66879606033384675 ) ) ;
#31190 = CARTESIAN_POINT ( 'NONE',  ( -17.42409385541305511, -14.80920654474410725, 52.21286476528345588 ) ) ;
#31191 = CARTESIAN_POINT ( 'NONE',  ( -42.05571150247187973, -14.80920654474419074, 65.94705882352940307 ) ) ;
#31192 = EDGE_LOOP ( 'NONE', ( #13958, #36348, #45262, #18870 ) ) ;
#31193 = CARTESIAN_POINT ( 'NONE',  ( -22.27409385650551243, -9.792211528768504536, 50.49490371617623197 ) ) ;
#31194 = VECTOR ( 'NONE', #10041, 1000.000000000000000 ) ;
#31195 = AXIS2_PLACEMENT_3D ( 'NONE', #26106, #14992, #45082 ) ;
#31196 = VERTEX_POINT ( 'NONE', #6360 ) ;
#31197 = LINE ( 'NONE', #34878, #13068 ) ;
#31198 = CARTESIAN_POINT ( 'NONE',  ( -24.46260454045723520, -17.25128545673921465, 73.00619124008264293 ) ) ;
#31199 = AXIS2_PLACEMENT_3D ( 'NONE', #36085, #10000, #22055 ) ;
#31200 = EDGE_LOOP ( 'NONE', ( #45752, #27852 ) ) ;
#31201 = CYLINDRICAL_SURFACE ( 'NONE', #18590, 0.1500000000000057676 ) ;
#31202 = FACE_OUTER_BOUND ( 'NONE', #8505, .T. ) ;
#31203 = DIRECTION ( 'NONE',  ( -0.09855345062332551698, -0.9951317587989214619, -3.188559572103130227E-08 ) ) ;
#31204 = CARTESIAN_POINT ( 'NONE',  ( -22.83095840648717711, -19.93459376977450859, 72.82895984417613988 ) ) ;
#31205 = EDGE_LOOP ( 'NONE', ( #4913, #43460 ) ) ;
#31206 = CARTESIAN_POINT ( 'NONE',  ( -50.42409385541304800, -27.10920654474410796, 63.99999999999998579 ) ) ;
#31207 = CARTESIAN_POINT ( 'NONE',  ( -22.91699213338677055, -19.14904519381134307, 58.90027305065820684 ) ) ;
#31208 = CARTESIAN_POINT ( 'NONE',  ( -12.38818700662999994, -20.29940648439967887, 68.43633818813384551 ) ) ;
#31209 = ORIENTED_EDGE ( 'NONE', *, *, #44602, .T. ) ;
#31210 = CARTESIAN_POINT ( 'NONE',  ( -10.37560970945560967, -14.44337087574636769, 61.07388280500082800 ) ) ;
#31211 = VERTEX_POINT ( 'NONE', #16700 ) ;
#31212 = CARTESIAN_POINT ( 'NONE',  ( -9.974233412304723601, -14.74161775280529341, 71.46636207693717324 ) ) ;
#31213 = CARTESIAN_POINT ( 'NONE',  ( -24.35389707626741185, -16.10709931453381216, 62.87856533165624029 ) ) ;
#31214 = ORIENTED_EDGE ( 'NONE', *, *, #14832, .T. ) ;
#31215 = ADVANCED_FACE ( 'NONE', ( #35419 ), #28765, .T. ) ;
#31216 = CARTESIAN_POINT ( 'NONE',  ( -16.45566506110110083, -21.79267588865899086, 62.04095995016087528 ) ) ;
#31217 = CARTESIAN_POINT ( 'NONE',  ( -24.64841560034816936, -12.98888891688536695, 63.00981035192142343 ) ) ;
#31218 = DIRECTION ( 'NONE',  ( -0.7506333037770538397, 0.6607190350373941534, 0.000000000000000000 ) ) ;
#31219 = DIRECTION ( 'NONE',  ( 0.7171836970970659753, -0.6968841687240311389, 4.479616660400600567E-09 ) ) ;
#31220 = ORIENTED_EDGE ( 'NONE', *, *, #3038, .F. ) ;
#31221 = CARTESIAN_POINT ( 'NONE',  ( -9.991168605297003680, -14.30431744343353628, 64.58078014788073062 ) ) ;
#31222 = UNCERTAINTY_MEASURE_WITH_UNIT (LENGTH_MEASURE( 1.000000000000000082E-05 ), #11692, 'distance_accuracy_value', 'NONE');
#31223 = CARTESIAN_POINT ( 'NONE',  ( -20.66207843469866745, -8.601311859664747317, 63.42194587956323204 ) ) ;
#31224 = CARTESIAN_POINT ( 'NONE',  ( -23.58616457878146377, -18.99640866789479432, 66.00884704819274873 ) ) ;
#31225 = CARTESIAN_POINT ( 'NONE',  ( -46.33910710821349710, -14.20920654474410760, 70.87000000000000455 ) ) ;
#31226 = VERTEX_POINT ( 'NONE', #36378 ) ;
#31227 = AXIS2_PLACEMENT_3D ( 'NONE', #19745, #46083, #18756 ) ;
#31228 = CIRCLE ( 'NONE', #5291, 2.000000000000002220 ) ;
#31229 = EDGE_CURVE ( 'NONE', #4206, #13279, #37023, .T. ) ;
#31230 = ADVANCED_FACE ( 'NONE', ( #28534 ), #2660, .T. ) ;
#31231 = CARTESIAN_POINT ( 'NONE',  ( -24.72547442936383888, -16.29049779397720243, 62.71611815716154581 ) ) ;
#31232 = ORIENTED_EDGE ( 'NONE', *, *, #42356, .F. ) ;
#31233 = VERTEX_POINT ( 'NONE', #35655 ) ;
#31234 = EDGE_CURVE ( 'NONE', #16837, #16407, #11076, .T. ) ;
#31235 = CARTESIAN_POINT ( 'NONE',  ( -24.85359113602694237, -14.25571898851532460, 69.76779851910008290 ) ) ;
#31236 = CARTESIAN_POINT ( 'NONE',  ( -10.15133553508400510, -13.19036488398009510, 71.32173201719281508 ) ) ;
#31237 = LINE ( 'NONE', #42584, #33517 ) ;
#31238 = CARTESIAN_POINT ( 'NONE',  ( -20.16159385650551883, -9.295667164867525756, 49.30633214617472504 ) ) ;
#31239 = EDGE_CURVE ( 'NONE', #21913, #34260, #32692, .T. ) ;
#31240 = CARTESIAN_POINT ( 'NONE',  ( -11.08714103679422713, -19.29340435200039394, 54.49999999999995026 ) ) ;
#31241 = CARTESIAN_POINT ( 'NONE',  ( -19.75213962495824305, -21.88613070990731302, 65.56462585307971835 ) ) ;
#31242 = ORIENTED_EDGE ( 'NONE', *, *, #11483, .F. ) ;
#31243 = ORIENTED_EDGE ( 'NONE', *, *, #7788, .F. ) ;
#31244 = CARTESIAN_POINT ( 'NONE',  ( -12.39977816794586829, -20.31007402754922353, 68.52931606572398948 ) ) ;
#31245 = EDGE_CURVE ( 'NONE', #38697, #8171, #24836, .T. ) ;
#31246 = CARTESIAN_POINT ( 'NONE',  ( 0.000000000000000000, 0.000000000000000000, 0.000000000000000000 ) ) ;
#31247 = CARTESIAN_POINT ( 'NONE',  ( -23.68216657795769109, -11.66929788463824202, 66.53287594076890343 ) ) ;
#31248 = CARTESIAN_POINT ( 'NONE',  ( 18.82590614458706924, 1.878297441959757785, 52.28023643296099010 ) ) ;
#31249 = CARTESIAN_POINT ( 'NONE',  ( -18.76558392140857023, -7.480892851696864021, 70.55563303198719893 ) ) ;
#31250 = ORIENTED_EDGE ( 'NONE', *, *, #36176, .T. ) ;
#31251 = CARTESIAN_POINT ( 'NONE',  ( -14.17409385759798823, -6.859212275519751323, 50.50378509014259265 ) ) ;
#31252 = CARTESIAN_POINT ( 'NONE',  ( -24.09792882696954663, -17.08130396874204138, 73.03336032035906555 ) ) ;
#31253 = CARTESIAN_POINT ( 'NONE',  ( -15.48424252676649182, -21.53505049348036948, 72.34575460973682937 ) ) ;
#31254 = CARTESIAN_POINT ( 'NONE',  ( -13.86159385541286326, -7.228003583437902613, 51.38655588712008182 ) ) ;
#31255 = ORIENTED_EDGE ( 'NONE', *, *, #47868, .F. ) ;
#31256 = AXIS2_PLACEMENT_3D ( 'NONE', #14721, #30049, #970 ) ;
#31257 = AXIS2_PLACEMENT_3D ( 'NONE', #18709, #7909, #29814 ) ;
#31258 = CARTESIAN_POINT ( 'NONE',  ( -50.42609385541305755, -14.90920654474420104, 66.05294117647058272 ) ) ;
#31259 = ORIENTED_EDGE ( 'NONE', *, *, #45484, .F. ) ;
#31260 = AXIS2_PLACEMENT_3D ( 'NONE', #32063, #47798, #14039 ) ;
#31261 = CARTESIAN_POINT ( 'NONE',  ( -14.72778360411233045, -21.32322305517535099, 58.31617885012778402 ) ) ;
#31262 = CARTESIAN_POINT ( 'NONE',  ( -24.21863450226962300, -16.49938964532870145, 59.23405620101143398 ) ) ;
#31263 = EDGE_CURVE ( 'NONE', #18577, #9916, #38207, .T. ) ;
#31264 = ORIENTED_EDGE ( 'NONE', *, *, #31742, .T. ) ;
#31265 = FACE_BOUND ( 'NONE', #33275, .T. ) ;
#31266 = AXIS2_PLACEMENT_3D ( 'NONE', #42689, #8956, #27410 ) ;
#31267 = ORIENTED_EDGE ( 'NONE', *, *, #24895, .T. ) ;
#31268 = CARTESIAN_POINT ( 'NONE',  ( -15.68503146357154776, -7.977064754671971514, 70.75989839959960648 ) ) ;
#31269 = FACE_OUTER_BOUND ( 'NONE', #16068, .T. ) ;
#31270 = ORIENTED_EDGE ( 'NONE', *, *, #19708, .T. ) ;
#31271 = CARTESIAN_POINT ( 'NONE',  ( -23.91010245674826251, -17.57297063409389537, 62.75888927877479517 ) ) ;
#31272 = ADVANCED_FACE ( 'NONE', ( #46759 ), #28034, .T. ) ;
#31273 = LINE ( 'NONE', #16230, #1405 ) ;
#31274 = CARTESIAN_POINT ( 'NONE',  ( -16.25534385650551528, -7.417179338643134834, 52.18511593390279302 ) ) ;
#31275 = LINE ( 'NONE', #27584, #18115 ) ;
#31276 = CARTESIAN_POINT ( 'NONE',  ( -19.31122959855452237, -8.013358182787271744, 63.84578077065769719 ) ) ;
#31277 = CARTESIAN_POINT ( 'NONE',  ( -10.93683055674727633, -17.43892421286904337, 64.73625468762544699 ) ) ;
#31278 = VERTEX_POINT ( 'NONE', #10774 ) ;
#31279 = FACE_OUTER_BOUND ( 'NONE', #42893, .T. ) ;
#31280 = CARTESIAN_POINT ( 'NONE',  ( -11.63680200852674496, -10.77675165258979284, 74.64704609179688077 ) ) ;
#31281 = CARTESIAN_POINT ( 'NONE',  ( -24.59520773924778325, -12.78944134693112744, 66.42433958033493013 ) ) ;
#31282 = CARTESIAN_POINT ( 'NONE',  ( -40.64308517176574753, -25.10920654474410441, 77.24806946917840378 ) ) ;
#31283 = ORIENTED_EDGE ( 'NONE', *, *, #14686, .T. ) ;
#31284 = ORIENTED_EDGE ( 'NONE', *, *, #39573, .T. ) ;
#31285 = ADVANCED_FACE ( 'NONE', ( #25548 ), #29988, .T. ) ;
#31286 = CARTESIAN_POINT ( 'NONE',  ( -11.16720068213728467, -11.56054720508597455, 67.76864607954532005 ) ) ;
#31287 = CARTESIAN_POINT ( 'NONE',  ( -24.36611147337434957, -16.04009697885371111, 66.07797069094537790 ) ) ;
#31288 = VERTEX_POINT ( 'NONE', #2891 ) ;
#31290 = CARTESIAN_POINT ( 'NONE',  ( -28.42409385541305511, -6.359206544744109735, 45.99999999999998579 ) ) ;
#31289 = AXIS2_PLACEMENT_3D ( 'NONE', #2568, #36036, #46662 ) ;
#31291 = FACE_OUTER_BOUND ( 'NONE', #21134, .T. ) ;
#31292 = CARTESIAN_POINT ( 'NONE',  ( -13.40955617598886995, -17.25032161083215954, 49.52966884056655772 ) ) ;
#31293 = EDGE_CURVE ( 'NONE', #14076, #8151, #41298, .T. ) ;
#31294 = CARTESIAN_POINT ( 'NONE',  ( -24.41419987208840325, -15.75358948762744760, 66.27144644829634501 ) ) ;
#31295 = PLANE ( 'NONE',  #9403 ) ;
#31296 = CARTESIAN_POINT ( 'NONE',  ( -12.17647495751581133, -14.96730746957505076, 52.02966884056656482 ) ) ;
#31297 = AXIS2_PLACEMENT_3D ( 'NONE', #20322, #42250, #42972 ) ;
#31298 = CARTESIAN_POINT ( 'NONE',  ( -23.72641715273374530, -11.63183476396761407, 70.03643756225406491 ) ) ;
#31299 = VECTOR ( 'NONE', #13799, 1000.000000000000000 ) ;
#31300 = EDGE_LOOP ( 'NONE', ( #46734, #38564 ) ) ;
#31301 = EDGE_CURVE ( 'NONE', #7468, #26935, #2972, .T. ) ;
#31302 = CARTESIAN_POINT ( 'NONE',  ( -22.23351441301664622, -19.96811234597608120, 69.58906588434240348 ) ) ;
#31303 = DIRECTION ( 'NONE',  ( -0.000000000000000000, -1.000000000000000000, -0.000000000000000000 ) ) ;
#31304 = CARTESIAN_POINT ( 'NONE',  ( -12.86353962931362283, -9.432586330540292607, 74.33395128836551180 ) ) ;
#31305 = VECTOR ( 'NONE', #40533, 999.9999999999998863 ) ;
#31306 = CARTESIAN_POINT ( 'NONE',  ( -17.63137589695670471, -7.812166007416677438, 63.85057029281470875 ) ) ;
#31307 = CARTESIAN_POINT ( 'NONE',  ( -21.37553466301574190, -9.031134576986278972, 70.24018460668924035 ) ) ;
#31308 = ADVANCED_FACE ( 'NONE', ( #6840 ), #11025, .T. ) ;
#31309 =( BOUNDED_CURVE ( )  B_SPLINE_CURVE ( 3, ( #19467, #41642, #30089, #7193 ),
 .UNSPECIFIED., .F., .F. ) 
 B_SPLINE_CURVE_WITH_KNOTS ( ( 4, 4 ),
 ( 0.9074455897393561843, 1.000000000000000000 ),
 .UNSPECIFIED. ) 
 CURVE ( )  GEOMETRIC_REPRESENTATION_ITEM ( )  RATIONAL_B_SPLINE_CURVE ( ( 0.6983129098260747458, 0.7760317562606824371, 0.8765941196519908551, 1.000000000000000000 ) ) 
 REPRESENTATION_ITEM ( '' )  );
#31310 = AXIS2_PLACEMENT_3D ( 'NONE', #17757, #9915, #39221 ) ;
#31311 = VERTEX_POINT ( 'NONE', #22344 ) ;
#31312 = VERTEX_POINT ( 'NONE', #44288 ) ;
#31313 = VERTEX_POINT ( 'NONE', #33911 ) ;
#31314 = CARTESIAN_POINT ( 'NONE',  ( -11.00364514860770271, -18.58846920323082585, 57.94568058987277936 ) ) ;
#31315 = ORIENTED_EDGE ( 'NONE', *, *, #4122, .T. ) ;
#31316 =( BOUNDED_CURVE ( )  B_SPLINE_CURVE ( 3, ( #19228, #34474, #22685, #31045 ),
 .UNSPECIFIED., .F., .F. ) 
 B_SPLINE_CURVE_WITH_KNOTS ( ( 4, 4 ),
 ( 0.4074455897393665094, 0.5000000000000000000 ),
 .UNSPECIFIED. ) 
 CURVE ( )  GEOMETRIC_REPRESENTATION_ITEM ( )  RATIONAL_B_SPLINE_CURVE ( ( 0.6983129098260970613, 0.7760317562606922071, 0.8765941196519905221, 0.9999999999999851230 ) ) 
 REPRESENTATION_ITEM ( '' )  );
#31317 = DIRECTION ( 'NONE',  ( 0.000000000000000000, 0.000000000000000000, 1.000000000000000000 ) ) ;
#31318 = CARTESIAN_POINT ( 'NONE',  ( -17.56322643164902431, -15.18422937902243142, 56.49999999999994316 ) ) ;
#31319 = EDGE_LOOP ( 'NONE', ( #43228, #10378 ) ) ;
#31320 = VECTOR ( 'NONE', #7547, 1000.000000000000114 ) ;
#31321 = CARTESIAN_POINT ( 'NONE',  ( -10.46488639952936950, -14.05403152202256223, 57.67498297385893125 ) ) ;
#31322 = VECTOR ( 'NONE', #20648, 1000.000000000000227 ) ;
#31323 = ORIENTED_EDGE ( 'NONE', *, *, #27445, .T. ) ;
#31324 = CARTESIAN_POINT ( 'NONE',  ( -20.03744868119640898, -21.78660147720172802, 69.04827188316701836 ) ) ;
#31325 = EDGE_CURVE ( 'NONE', #35729, #5074, #40809, .T. ) ;
#31326 = CARTESIAN_POINT ( 'NONE',  ( -17.56947109021050224, -7.760665246103527259, 63.85057029441095011 ) ) ;
#31327 = VECTOR ( 'NONE', #12925, 1000.000000000000000 ) ;
#31328 = ORIENTED_EDGE ( 'NONE', *, *, #15396, .T. ) ;
#31329 = FACE_OUTER_BOUND ( 'NONE', #36742, .T. ) ;
#31330 = CARTESIAN_POINT ( 'NONE',  ( -16.64258257546838138, -22.21885596081591174, 68.88215988439684168 ) ) ;
#31331 = CARTESIAN_POINT ( 'NONE',  ( -10.41342670640989176, -14.06412934096922562, 60.92381095562976867 ) ) ;
#31332 = ORIENTED_EDGE ( 'NONE', *, *, #29122, .T. ) ;
#31333 = DIRECTION ( 'NONE',  ( 1.000000000000000000, 0.000000000000000000, 0.000000000000000000 ) ) ;
#31334 = DIRECTION ( 'NONE',  ( 3.413470714839332458E-33, -1.190614954331866791E-16, 1.000000000000000000 ) ) ;
#31335 = VECTOR ( 'NONE', #5792, 1000.000000000000000 ) ;
#31336 = CARTESIAN_POINT ( 'NONE',  ( -18.33724152424255394, -21.79985958048214556, 69.11514682450841462 ) ) ;
#31337 = CARTESIAN_POINT ( 'NONE',  ( -10.77962265614084814, -17.18953632050836333, 68.24154640182683806 ) ) ;
#31338 = CARTESIAN_POINT ( 'NONE',  ( -14.91112529534803066, -8.221969756899694559, 57.13527940342243028 ) ) ;
#31339 = CARTESIAN_POINT ( 'NONE',  ( -17.51497182922874174, -7.809736700347588823, 63.56559502915499849 ) ) ;
#31340 = CARTESIAN_POINT ( 'NONE',  ( -17.92409385541305511, -14.80920654474410725, 52.21286476528345588 ) ) ;
#31341 = CARTESIAN_POINT ( 'NONE',  ( -10.76763535483202539, -17.13171813241336494, 61.30743118825921556 ) ) ;
#31342 = DIRECTION ( 'NONE',  ( -1.000000000000000000, 0.000000000000000000, 3.652049423109068320E-16 ) ) ;
#31343 = CARTESIAN_POINT ( 'NONE',  ( -16.89909385650551599, -8.114302828567740988, 52.18300498402516041 ) ) ;
#31344 = ORIENTED_EDGE ( 'NONE', *, *, #30501, .F. ) ;
#31345 = EDGE_CURVE ( 'NONE', #15104, #28108, #37922, .T. ) ;
#31346 = DIRECTION ( 'NONE',  ( 0.9687793358424821033, -0.2479245821708677133, 0.000000000000000000 ) ) ;
#31347 = LINE ( 'NONE', #23741, #11624 ) ;
#31348 = VERTEX_POINT ( 'NONE', #48436 ) ;
#31350 = CARTESIAN_POINT ( 'NONE',  ( -13.89389072038462025, -21.36980434119256600, 72.11103101793651149 ) ) ;
#31349 = B_SPLINE_CURVE_WITH_KNOTS ( 'NONE', 3,
 ( #13714, #5873, #13478, #9813, #28279, #24599, #24827, #28526, #20888, #35412 ),
 .UNSPECIFIED., .F., .F.,
 ( 4, 2, 2, 2, 4 ),
 ( 0.1272669073658556915, 0.2522669073488191804, 0.3772669073317826971, 0.5022669073147462138, 0.6272669072977097304 ),
 .UNSPECIFIED. ) ;
#31351 = CARTESIAN_POINT ( 'NONE',  ( -14.66630222544868900, -8.320656262913127321, 63.80450889863892172 ) ) ;
#31352 = CARTESIAN_POINT ( 'NONE',  ( -24.23636277187043220, -17.82529184948975498, 62.58865552117998021 ) ) ;
#31353 = CARTESIAN_POINT ( 'NONE',  ( -12.68381401182790569, -19.95991009262169413, 68.33657438305763776 ) ) ;
#31354 = CARTESIAN_POINT ( 'NONE',  ( -14.71062220868414805, -21.26200545334448222, 58.16617879205879404 ) ) ;
#31355 = VERTEX_POINT ( 'NONE', #45022 ) ;
#31356 = CARTESIAN_POINT ( 'NONE',  ( -23.73600461991442501, -11.78168063161743362, 62.96834887429472616 ) ) ;
#31357 = CARTESIAN_POINT ( 'NONE',  ( -19.86569447268030686, -19.73755174630646536, 53.49899999999994549 ) ) ;
#31358 = EDGE_CURVE ( 'NONE', #7797, #33382, #22111, .T. ) ;
#31359 = CARTESIAN_POINT ( 'NONE',  ( -19.09949158415725634, -8.012660229328147921, 63.43089235425713923 ) ) ;
#31360 = VERTEX_POINT ( 'NONE', #29003 ) ;
#31361 = CYLINDRICAL_SURFACE ( 'NONE', #14031, 0.1500000000000004385 ) ;
#31362 = AXIS2_PLACEMENT_3D ( 'NONE', #24919, #39933, #17018 ) ;
#31363 = EDGE_CURVE ( 'NONE', #17355, #23884, #37586, .T. ) ;
#31364 = DIRECTION ( 'NONE',  ( 0.9687793358424817702, -0.2479245821708684905, 0.000000000000000000 ) ) ;
#31365 = VECTOR ( 'NONE', #36126, 1000.000000000000227 ) ;
#31366 = CARTESIAN_POINT ( 'NONE',  ( -21.78293781325145773, -8.767371536720848013, 70.23858402064847439 ) ) ;
#31367 = CARTESIAN_POINT ( 'NONE',  ( -45.90217435822630421, -14.20017296387473138, 71.05663168951063824 ) ) ;
#31368 = AXIS2_PLACEMENT_3D ( 'NONE', #42630, #2208, #20199 ) ;
#31369 = AXIS2_PLACEMENT_3D ( 'NONE', #26932, #15826, #34294 ) ;
#31370 = ORIENTED_EDGE ( 'NONE', *, *, #45560, .F. ) ;
#31371 = EDGE_LOOP ( 'NONE', ( #37692, #45500, #31731, #15156 ) ) ;
#31372 = CARTESIAN_POINT ( 'NONE',  ( -22.58034385541304445, -9.360768649639302552, 51.01397948905921709 ) ) ;
#31373 = DIRECTION ( 'NONE',  ( 3.549360974554993999E-17, -6.371834667797928663E-18, -1.000000000000000000 ) ) ;
#31374 = CARTESIAN_POINT ( 'NONE',  ( -15.35181094580836358, -7.653138554841501850, 74.12339718037890179 ) ) ;
#31375 = AXIS2_PLACEMENT_3D ( 'NONE', #42742, #9010, #20328 ) ;
#31376 = ADVANCED_FACE ( 'NONE', ( #33161 ), #3629, .F. ) ;
#31377 = EDGE_CURVE ( 'NONE', #12986, #27864, #38585, .T. ) ;
#31378 = CARTESIAN_POINT ( 'NONE',  ( -14.27319436148695431, -8.558459998996717388, 71.02957628730779049 ) ) ;
#31379 = EDGE_CURVE ( 'NONE', #33892, #1223, #18231, .T. ) ;
#31380 = DIRECTION ( 'NONE',  ( 0.1240347345892083841, 0.000000000000000000, 0.9922778767136676281 ) ) ;
#31381 = CARTESIAN_POINT ( 'NONE',  ( -9.979603264230430426, -14.52052340097724148, 68.04295441848455539 ) ) ;
#31382 = CARTESIAN_POINT ( 'NONE',  ( -24.26194381736407735, -17.76675604995504543, 62.66635152724034441 ) ) ;
#31383 = ORIENTED_EDGE ( 'NONE', *, *, #48514, .F. ) ;
#31384 = DIRECTION ( 'NONE',  ( -1.000000000000000000, 4.164305804376849172E-17, -1.614929280266638808E-16 ) ) ;
#31385 = ORIENTED_EDGE ( 'NONE', *, *, #33889, .T. ) ;
#31386 = CARTESIAN_POINT ( 'NONE',  ( -10.13784000599894597, -13.25541019000276499, 74.79322239981686948 ) ) ;
#31387 = CARTESIAN_POINT ( 'NONE',  ( -9.974321184477874525, -14.87343388147542100, 74.99117216852748413 ) ) ;
#31388 = ORIENTED_EDGE ( 'NONE', *, *, #30957, .T. ) ;
#31389 = CYLINDRICAL_SURFACE ( 'NONE', #41923, 0.1500000000000031863 ) ;
#31390 = FACE_OUTER_BOUND ( 'NONE', #34003, .T. ) ;
#31391 = AXIS2_PLACEMENT_3D ( 'NONE', #48176, #6336, #21834 ) ;
#31392 =( BOUNDED_CURVE ( )  B_SPLINE_CURVE ( 3, ( #43369, #32283, #21195, #5456 ),
 .UNSPECIFIED., .F., .F. ) 
 B_SPLINE_CURVE_WITH_KNOTS ( ( 4, 4 ),
 ( 0.4074455897393643444, 0.5000000000000000000 ),
 .UNSPECIFIED. ) 
 CURVE ( )  GEOMETRIC_REPRESENTATION_ITEM ( )  RATIONAL_B_SPLINE_CURVE ( ( 0.6983129098261118273, 0.7760317562607139674, 0.8765941196520097289, 0.9999999999999991118 ) ) 
 REPRESENTATION_ITEM ( '' )  );
#31393 = PRODUCT_DEFINITION_FORMATION_WITH_SPECIFIED_SOURCE ( 'ANY', '', #8746, .NOT_KNOWN. ) ;
#31394 = DIRECTION ( 'NONE',  ( 0.000000000000000000, 0.000000000000000000, -1.000000000000000000 ) ) ;
#31395 = ORIENTED_EDGE ( 'NONE', *, *, #14146, .F. ) ;
#31396 = CARTESIAN_POINT ( 'NONE',  ( -18.57335281209669375, -21.76520412651811043, 72.57038810541313012 ) ) ;
#31397 = DIRECTION ( 'NONE',  ( -0.4182840851231335866, 0.9083162577718750796, -8.112345261760041810E-09 ) ) ;
#31398 = AXIS2_PLACEMENT_3D ( 'NONE', #7701, #48554, #22462 ) ;
#31400 = DIRECTION ( 'NONE',  ( -6.291559624462811924E-07, 1.530398240482465057E-06, -0.9999999999986309840 ) ) ;
#31399 = CIRCLE ( 'NONE', #10185, 4.686499999999998778 ) ;
#31401 = FACE_BOUND ( 'NONE', #16915, .T. ) ;
#31402 = CARTESIAN_POINT ( 'NONE',  ( -20.72450927900464634, -21.03929139025762751, 58.93003081252663833 ) ) ;
#31403 = CARTESIAN_POINT ( 'NONE',  ( -17.46222794319647775, -7.759011850482251837, 67.03511641684839617 ) ) ;
#31404 = CARTESIAN_POINT ( 'NONE',  ( -22.57893663749957369, -9.999394138389961384, 73.49633153340955971 ) ) ;
#31405 = ORIENTED_EDGE ( 'NONE', *, *, #34946, .T. ) ;
#31406 = CARTESIAN_POINT ( 'NONE',  ( -21.84079957929829874, -9.314189696129256291, 63.19153755727188582 ) ) ;
#31407 = VECTOR ( 'NONE', #29347, 1000.000000000000000 ) ;
#31408 = ORIENTED_EDGE ( 'NONE', *, *, #20171, .F. ) ;
#31409 = DIRECTION ( 'NONE',  ( -5.731567514496413899E-31, -1.020425574103664789E-16, -1.000000000000000000 ) ) ;
#31410 = DIRECTION ( 'NONE',  ( 0.02400335114476204526, -0.9997118780597843424, -1.529429985666831130E-10 ) ) ;
#31411 = ORIENTED_EDGE ( 'NONE', *, *, #16234, .F. ) ;
#31412 = CARTESIAN_POINT ( 'NONE',  ( -17.42409385541299471, -14.80920654474435771, 49.52966884056655772 ) ) ;
#31413 = CARTESIAN_POINT ( 'NONE',  ( -11.60006209888454443, -10.16330164164447325, 71.08397698276321819 ) ) ;
#31414 = EDGE_CURVE ( 'NONE', #3376, #48249, #17352, .T. ) ;
#31415 = VERTEX_POINT ( 'NONE', #33645 ) ;
#31416 = EDGE_LOOP ( 'NONE', ( #42295, #24143, #31328, #6879 ) ) ;
#31417 = ORIENTED_EDGE ( 'NONE', *, *, #47060, .F. ) ;
#31418 = EDGE_CURVE ( 'NONE', #23554, #45950, #20619, .T. ) ;
#31419 = CARTESIAN_POINT ( 'NONE',  ( -10.41569439578338496, -15.57669382292980131, 61.05261153187079515 ) ) ;
#31420 = CYLINDRICAL_SURFACE ( 'NONE', #7521, 0.1500000000000042133 ) ;
#31421 = DIRECTION ( 'NONE',  ( 1.224646799147353207E-16, 1.000000000000000000, -1.912410701131276611E-32 ) ) ;
#31422 = ORIENTED_EDGE ( 'NONE', *, *, #22044, .T. ) ;
#31423 = ORIENTED_EDGE ( 'NONE', *, *, #16898, .T. ) ;
#31424 = CARTESIAN_POINT ( 'NONE',  ( -20.64284385650552167, -8.811426318492348031, 52.18089403414751359 ) ) ;
#31425 = CARTESIAN_POINT ( 'NONE',  ( -22.68532657142340980, -20.08396690885253477, 69.21772085510332317 ) ) ;
#31426 = CIRCLE ( 'NONE', #16468, 1.949999999999999956 ) ;
#31427 = CARTESIAN_POINT ( 'NONE',  ( -22.41668094288463919, -16.43295965837073780, 49.52966884056655772 ) ) ;
#31428 = CARTESIAN_POINT ( 'NONE',  ( -7.424093855413048892, -25.10920654474410441, 77.00000000000000000 ) ) ;
#31429 = CARTESIAN_POINT ( 'NONE',  ( -13.35534385650551492, -7.417179338643134834, 52.18511593390279302 ) ) ;
#31430 = AXIS2_PLACEMENT_3D ( 'NONE', #6877, #48229, #14466 ) ;
#31431 = EDGE_CURVE ( 'NONE', #25227, #23300, #30050, .T. ) ;
#31432 = EDGE_LOOP ( 'NONE', ( #25375, #46660, #15029, #6 ) ) ;
#31433 = EDGE_CURVE ( 'NONE', #30016, #37344, #21856, .T. ) ;
#31434 = EDGE_CURVE ( 'NONE', #39530, #35725, #24128, .T. ) ;
#31435 = CARTESIAN_POINT ( 'NONE',  ( -14.72662834380375685, -21.75384922062382032, 61.75883521239082086 ) ) ;
#31436 = EDGE_CURVE ( 'NONE', #8033, #35067, #19138, .T. ) ;
#31437 = CARTESIAN_POINT ( 'NONE',  ( -15.33756252250768881, -21.49113013396807403, 68.57592903490986203 ) ) ;
#31438 = CARTESIAN_POINT ( 'NONE',  ( -17.32080883166002039, -7.809907297400525472, 67.30574285593853290 ) ) ;
#31439 = AXIS2_PLACEMENT_3D ( 'NONE', #6856, #13504, #28548 ) ;
#31440 =( BOUNDED_CURVE ( )  B_SPLINE_CURVE ( 3, ( #44576, #18211, #35959, #33217 ),
 .UNSPECIFIED., .F., .F. ) 
 B_SPLINE_CURVE_WITH_KNOTS ( ( 4, 4 ),
 ( 0.9074455897393632897, 1.000000000000000000 ),
 .UNSPECIFIED. ) 
 CURVE ( )  GEOMETRIC_REPRESENTATION_ITEM ( )  RATIONAL_B_SPLINE_CURVE ( ( 0.6983129098260834056, 0.7760317562606898756, 0.8765941196519954071, 1.000000000000000000 ) ) 
 REPRESENTATION_ITEM ( '' )  );
#31441 = ORIENTED_EDGE ( 'NONE', *, *, #15946, .T. ) ;
#31442 = CARTESIAN_POINT ( 'NONE',  ( -11.68335768792166185, -18.81469630946190819, 68.51689631952916670 ) ) ;
#31443 = CARTESIAN_POINT ( 'NONE',  ( -10.83541799943766293, -17.32598710976732903, 61.04254427365582103 ) ) ;
#31444 = DIRECTION ( 'NONE',  ( -0.000000000000000000, -1.000000000000000000, -0.000000000000000000 ) ) ;
#31445 = CARTESIAN_POINT ( 'NONE',  ( -24.17309265654468931, -11.65389292077413685, 59.62089248282786969 ) ) ;
#31446 = ORIENTED_EDGE ( 'NONE', *, *, #41539, .T. ) ;
#31447 = CARTESIAN_POINT ( 'NONE',  ( -21.02292652713908794, -10.98678540089889744, 52.02966884056656482 ) ) ;
#31448 = CARTESIAN_POINT ( 'NONE',  ( -35.32409385541306079, -2.423472813913224222, 52.29999999999998295 ) ) ;
#31449 = CARTESIAN_POINT ( 'NONE',  ( -11.39842260918292638, -18.37420288192462792, 61.34881185081356847 ) ) ;
#31450 = VERTEX_POINT ( 'NONE', #42281 ) ;
#31451 = CARTESIAN_POINT ( 'NONE',  ( -16.01882192674287708, -7.492892668753452945, 63.86349355235967806 ) ) ;
#31452 =( BOUNDED_CURVE ( )  B_SPLINE_CURVE ( 3, ( #32442, #47465, #13700, #15837 ),
 .UNSPECIFIED., .F., .F. ) 
 B_SPLINE_CURVE_WITH_KNOTS ( ( 4, 4 ),
 ( 0.000000000000000000, 0.4074455897393696180 ),
 .UNSPECIFIED. ) 
 CURVE ( )  GEOMETRIC_REPRESENTATION_ITEM ( )  RATIONAL_B_SPLINE_CURVE ( ( 1.000000000000000000, 0.4567392136813263059, 0.3561768502900282130, 0.6983129098261057210 ) ) 
 REPRESENTATION_ITEM ( '' )  );
#31453 = ORIENTED_EDGE ( 'NONE', *, *, #46174, .T. ) ;
#31454 = CARTESIAN_POINT ( 'NONE',  ( -21.47456293661849713, -9.038556783377254433, 70.41660404402310292 ) ) ;
#31455 = CARTESIAN_POINT ( 'NONE',  ( -10.37714865501246564, -15.10143083228766159, 74.68290095780284332 ) ) ;
#31456 = ORIENTED_EDGE ( 'NONE', *, *, #48142, .T. ) ;
#31457 = CARTESIAN_POINT ( 'NONE',  ( -22.16028090469329825, -20.56016676735646698, 58.90409545820185144 ) ) ;
#31459 = EDGE_CURVE ( 'NONE', #39406, #45116, #41769, .T. ) ;
#31458 = FACE_OUTER_BOUND ( 'NONE', #22652, .T. ) ;
#31460 = CARTESIAN_POINT ( 'NONE',  ( -24.22177711603362482, -13.13842781680106420, 62.83264177645653348 ) ) ;
#31461 = CIRCLE ( 'NONE', #14916, 1.999999999999994893 ) ;
#31462 = DIRECTION ( 'NONE',  ( -0.8810891847886966888, -0.4615090133018290852, 0.1033986416233891037 ) ) ;
#31463 = VERTEX_POINT ( 'NONE', #12001 ) ;
#31464 = FACE_OUTER_BOUND ( 'NONE', #26652, .T. ) ;
#31465 = AXIS2_PLACEMENT_3D ( 'NONE', #45096, #41373, #26125 ) ;
#31466 = CARTESIAN_POINT ( 'NONE',  ( -10.89280251029460622, -11.22507333849785027, 64.33377325762776877 ) ) ;
#31467 = CARTESIAN_POINT ( 'NONE',  ( -22.24221110980738558, -9.126920263178931236, 59.92159993762222570 ) ) ;
#31468 = EDGE_LOOP ( 'NONE', ( #43378, #47711, #2499, #38944 ) ) ;
#31469 = CARTESIAN_POINT ( 'NONE',  ( -15.75283698213507755, -7.548994588147243334, 67.32502552484606895 ) ) ;
#31470 = CIRCLE ( 'NONE', #19670, 0.5560000000000009379 ) ;
#31471 =( BOUNDED_SURFACE ( )  B_SPLINE_SURFACE ( 3, 1, ( 
 ( #4545, #27441 ),
 ( #8983, #41985 ),
 ( #31632, #20301 ),
 ( #38257, #20058 ),
 ( #39255, #1325 ),
 ( #27200, #34328 ),
 ( #862, #31381 ) ),
 .UNSPECIFIED., .T., .F., .F. ) 
 B_SPLINE_SURFACE_WITH_KNOTS ( ( 4, 3, 4 ),
 ( 2, 2 ),
 ( 0.000000000000000000, 0.5000000000000000000, 1.000000000000000000 ),
 ( 0.000000000000000000, 1.000000000000000000 ),
 .UNSPECIFIED. ) 
 GEOMETRIC_REPRESENTATION_ITEM ( )  RATIONAL_B_SPLINE_SURFACE ( (
 ( 1.000000000000000000, 1.000000000000000000),
 ( 0.3333333333333335369, 0.3333333333333330373),
 ( 0.3333333333333335369, 0.3333333333333330373),
 ( 1.000000000000000000, 1.000000000000000000),
 ( 0.3333333333333333703, 0.3333333333333333703),
 ( 0.3333333333333333703, 0.3333333333333333703),
 ( 1.000000000000000000, 1.000000000000000000) ) ) 
 REPRESENTATION_ITEM ( '' )  SURFACE ( )  );
#31472 = ORIENTED_EDGE ( 'NONE', *, *, #10906, .T. ) ;
#31473 = EDGE_LOOP ( 'NONE', ( #1074, #11849 ) ) ;
#31474 = CARTESIAN_POINT ( 'NONE',  ( -10.44881481234349252, -17.42631575494719698, 64.74243950200344955 ) ) ;
#31475 = CARTESIAN_POINT ( 'NONE',  ( -13.01353397724842154, -8.804979801064929390, 64.09441804368185558 ) ) ;
#31476 = ADVANCED_FACE ( 'NONE', ( #4858, #917 ), #41550, .T. ) ;
#31477 = CARTESIAN_POINT ( 'NONE',  ( -10.37541943412130863, -14.96049300415475614, 75.08306784598362071 ) ) ;
#31478 = CIRCLE ( 'NONE', #2407, 0.3999999999999978018 ) ;
#31479 = CARTESIAN_POINT ( 'NONE',  ( -17.51784385650551812, -9.790100578890868377, 49.79778022625163203 ) ) ;
#31480 = CARTESIAN_POINT ( 'NONE',  ( -42.79688797306011594, -14.80920654474410547, 60.01764705882351336 ) ) ;
#31481 = B_SPLINE_CURVE_WITH_KNOTS ( 'NONE', 3,
 ( #15987, #39385, #31033, #5666, #46049, #20679, #27329, #1219, #16222, #27576 ),
 .UNSPECIFIED., .F., .F.,
 ( 4, 2, 2, 2, 4 ),
 ( 0.1272669073658583838, 0.2522669073439522958, 0.3772669073220461522, 0.5022669073001400086, 0.6272669072782339761 ),
 .UNSPECIFIED. ) ;
#31482 = CARTESIAN_POINT ( 'NONE',  ( -23.41616298382994898, -18.52428493080399363, 72.77840375779385340 ) ) ;
#31483 = CARTESIAN_POINT ( 'NONE',  ( -23.26031807999110157, -18.67503349580112015, 69.30988682986618699 ) ) ;
#31484 = CARTESIAN_POINT ( 'NONE',  ( -11.13733870171179596, -11.61806121328042174, 67.90392505421056057 ) ) ;
#31485 = VERTEX_POINT ( 'NONE', #27497 ) ;
#31486 = ORIENTED_EDGE ( 'NONE', *, *, #30141, .F. ) ;
#31487 = CARTESIAN_POINT ( 'NONE',  ( -11.18734459328334907, -11.50497870355291319, 60.83452645039198359 ) ) ;
#31488 =( NAMED_UNIT ( * ) SI_UNIT ( $, .STERADIAN. ) SOLID_ANGLE_UNIT ( ) );
#31489 = CARTESIAN_POINT ( 'NONE',  ( -22.97409385541299542, -6.859212275519753099, 50.50378509014307582 ) ) ;
#31490 = CARTESIAN_POINT ( 'NONE',  ( -13.18362795047878144, -8.683667697493742565, 60.62445659250467145 ) ) ;
#31491 = CARTESIAN_POINT ( 'NONE',  ( -21.85574357498200015, -9.390598081573159561, 59.79459286646363836 ) ) ;
#31492 = B_SPLINE_CURVE_WITH_KNOTS ( 'NONE', 3,
 ( #46785, #43083, #24383, #39393, #20687, #44544, #48462, #10799, #37876, #21882 ),
 .UNSPECIFIED., .F., .F.,
 ( 4, 2, 2, 2, 4 ),
 ( 0.6272669072877963270, 0.7522669073073113832, 0.8772669073268264395, 1.002266907346341496, 1.127266907365856552 ),
 .UNSPECIFIED. ) ;
#31493 = ORIENTED_EDGE ( 'NONE', *, *, #46729, .F. ) ;
#31494 = EDGE_CURVE ( 'NONE', #47561, #32087, #24728, .T. ) ;
#31495 = EDGE_CURVE ( 'NONE', #29913, #1662, #8308, .T. ) ;
#31496 = LINE ( 'NONE', #5653, #20964 ) ;
#31497 = CARTESIAN_POINT ( 'NONE',  ( -24.48201381491371009, -14.78211897600973934, 66.32725479646262556 ) ) ;
#31498 = VECTOR ( 'NONE', #46669, 1000.000000000000000 ) ;
#31499 = CARTESIAN_POINT ( 'NONE',  ( -14.92957361138602579, -21.82925975653312278, 65.22101252026929785 ) ) ;
#31500 = CARTESIAN_POINT ( 'NONE',  ( -13.97409385541301496, -6.859212275519754876, 50.50378509014287687 ) ) ;
#31501 = ORIENTED_EDGE ( 'NONE', *, *, #13014, .F. ) ;
#31502 = AXIS2_PLACEMENT_3D ( 'NONE', #7831, #37584, #15415 ) ;
#31503 = CARTESIAN_POINT ( 'NONE',  ( -10.55452786565646228, -16.15453179965403763, 68.05055783647944168 ) ) ;
#31504 = EDGE_CURVE ( 'NONE', #26563, #4162, #28295, .T. ) ;
#31505 = EDGE_CURVE ( 'NONE', #30656, #23723, #26780, .T. ) ;
#31506 = CARTESIAN_POINT ( 'NONE',  ( -24.03160980685186843, -17.26750534774173929, 69.41339792588560442 ) ) ;
#31507 = ORIENTED_EDGE ( 'NONE', *, *, #18933, .T. ) ;
#31508 = EDGE_CURVE ( 'NONE', #29774, #24601, #30242, .T. ) ;
#31509 = AXIS2_PLACEMENT_3D ( 'NONE', #441, #18897, #23572 ) ;
#31510 = PLANE ( 'NONE',  #29676 ) ;
#31511 = CARTESIAN_POINT ( 'NONE',  ( -24.24305604114050539, -16.39138756491875171, 59.12332478929949531 ) ) ;
#31512 = EDGE_LOOP ( 'NONE', ( #38544, #2009 ) ) ;
#31513 = DIRECTION ( 'NONE',  ( 0.000000000000000000, 0.000000000000000000, -1.000000000000000000 ) ) ;
#31514 = ORIENTED_EDGE ( 'NONE', *, *, #7460, .T. ) ;
#31515 = LINE ( 'NONE', #11837, #22838 ) ;
#31516 = CARTESIAN_POINT ( 'NONE',  ( -18.71262049920375503, -21.74350751539899562, 72.17022092985547488 ) ) ;
#31517 = ORIENTED_EDGE ( 'NONE', *, *, #27895, .F. ) ;
#31518 = DIRECTION ( 'NONE',  ( 0.8467008005855412023, -0.3141239757129647425, -0.4294460177601887585 ) ) ;
#31519 = DIRECTION ( 'NONE',  ( 0.5881408891789771110, 0.8087584895849666555, -7.565907429265703656E-08 ) ) ;
#31520 = ADVANCED_FACE ( 'NONE', ( #7833 ), #44281, .T. ) ;
#31521 = PRESENTATION_LAYER_ASSIGNMENT (  '', '', ( #2418 ) ) ;
#31522 = CARTESIAN_POINT ( 'NONE',  ( -16.93034385650551954, -9.794322478646142471, 51.19202720610083190 ) ) ;
#31523 = ORIENTED_EDGE ( 'NONE', *, *, #32376, .T. ) ;
#31524 = CARTESIAN_POINT ( 'NONE',  ( -14.80072874354800305, -7.836285926156586257, 56.89354091526551116 ) ) ;
#31525 = CARTESIAN_POINT ( 'NONE',  ( -24.45577199812615632, -12.20047074031916168, 47.99999999999994316 ) ) ;
#31526 = VERTEX_POINT ( 'NONE', #40036 ) ;
#31527 = CARTESIAN_POINT ( 'NONE',  ( -16.13676401591364140, -7.928535094101303748, 60.42701728694442664 ) ) ;
#31528 = CARTESIAN_POINT ( 'NONE',  ( -11.64873123714592396, -10.76074834137913960, 74.32396018297762907 ) ) ;
#31529 = FACE_OUTER_BOUND ( 'NONE', #17623, .T. ) ;
#31530 = CARTESIAN_POINT ( 'NONE',  ( -22.10255287824656989, -12.42708119714673565, 52.02966884056656482 ) ) ;
#31531 = VECTOR ( 'NONE', #15179, 1000.000000000000000 ) ;
#31532 = CARTESIAN_POINT ( 'NONE',  ( -12.25319814409069252, -20.17255476956438542, 64.91028984507975963 ) ) ;
#31533 = ORIENTED_EDGE ( 'NONE', *, *, #32715, .T. ) ;
#31534 = ORIENTED_EDGE ( 'NONE', *, *, #39126, .F. ) ;
#31535 = AXIS2_PLACEMENT_3D ( 'NONE', #1120, #16854, #1355 ) ;
#31536 = CARTESIAN_POINT ( 'NONE',  ( -36.42409385541304800, -7.059211358595575803, 50.50317947571981847 ) ) ;
#31537 = CARTESIAN_POINT ( 'NONE',  ( -24.31724253335826447, -16.02795960786995977, 62.82001908927701805 ) ) ;
#31538 = ORIENTED_EDGE ( 'NONE', *, *, #45709, .F. ) ;
#31539 = LINE ( 'NONE', #31290, #13868 ) ;
#31540 = CARTESIAN_POINT ( 'NONE',  ( -19.41474841345058522, -21.52018966427049307, 62.29503644830997189 ) ) ;
#31541 = CARTESIAN_POINT ( 'NONE',  ( -23.01604236747990839, -10.51564102213499474, 59.89643612291379071 ) ) ;
#31542 = LINE ( 'NONE', #42870, #4578 ) ;
#31543 = DIRECTION ( 'NONE',  ( -1.000000000000000000, -2.866981220435666553E-17, 0.000000000000000000 ) ) ;
#31544 = CARTESIAN_POINT ( 'NONE',  ( -27.42409385541305156, -15.80920654474410725, 74.99999999999998579 ) ) ;
#31545 = ORIENTED_EDGE ( 'NONE', *, *, #32916, .T. ) ;
#31546 = CARTESIAN_POINT ( 'NONE',  ( -16.92050523043788957, -21.84918965566402704, 65.38131313066115524 ) ) ;
#31547 = CARTESIAN_POINT ( 'NONE',  ( -19.17247957453286844, -7.567181637230756763, 63.61584517348745038 ) ) ;
#31548 = AXIS2_PLACEMENT_3D ( 'NONE', #15301, #30366, #22474 ) ;
#31549 = CARTESIAN_POINT ( 'NONE',  ( -12.58002213166789041, -9.148928514680237711, 74.43427606957253317 ) ) ;
#31550 = CARTESIAN_POINT ( 'NONE',  ( -12.57881008754452345, -9.149975892475048056, 74.57568945445216002 ) ) ;
#31551 = CARTESIAN_POINT ( 'NONE',  ( -21.18000576974785787, -20.77541348745421246, 69.35450184739246993 ) ) ;
#31552 = EDGE_CURVE ( 'NONE', #27678, #9892, #22856, .T. ) ;
#31553 = ORIENTED_EDGE ( 'NONE', *, *, #2167, .F. ) ;
#31554 = VERTEX_POINT ( 'NONE', #17114 ) ;
#31555 = EDGE_LOOP ( 'NONE', ( #21684, #18809, #47675, #30509, #39450 ) ) ;
#31556 = EDGE_CURVE ( 'NONE', #6043, #33004, #24548, .T. ) ;
#31557 = CARTESIAN_POINT ( 'NONE',  ( -17.79901357976508791, -7.766176623049141803, 63.96545652844361740 ) ) ;
#31558 = TOROIDAL_SURFACE ( 'NONE', #19792, 1.500000000000000000, 0.5000000000000000000 ) ;
#31559 = CARTESIAN_POINT ( 'NONE',  ( -20.01035006975242680, -21.36773898636727509, 72.70478738042278621 ) ) ;
#31560 = ORIENTED_EDGE ( 'NONE', *, *, #8269, .T. ) ;
#31561 = CARTESIAN_POINT ( 'NONE',  ( -21.73662441638722953, -9.231682010981758779, 66.67622112302015580 ) ) ;
#31562 = EDGE_CURVE ( 'NONE', #35234, #39678, #17369, .T. ) ;
#31563 = ORIENTED_EDGE ( 'NONE', *, *, #21097, .F. ) ;
#31564 = EDGE_CURVE ( 'NONE', #47492, #24829, #9465, .T. ) ;
#31565 = VECTOR ( 'NONE', #47102, 1000.000000000000000 ) ;
#31566 = CARTESIAN_POINT ( 'NONE',  ( -10.63133999448158384, -17.86890150755132822, 71.67379904062892138 ) ) ;
#31567 = CARTESIAN_POINT ( 'NONE',  ( -19.30128557755455176, -21.60500301973953086, 58.81035253397666196 ) ) ;
#31568 = ADVANCED_FACE ( 'NONE', ( #16876 ), #13175, .T. ) ;
#31569 = ORIENTED_EDGE ( 'NONE', *, *, #21942, .T. ) ;
#31570 = CYLINDRICAL_SURFACE ( 'NONE', #25737, 2.500000000000000444 ) ;
#31571 = CIRCLE ( 'NONE', #26840, 2.000000000000008882 ) ;
#31572 = CARTESIAN_POINT ( 'NONE',  ( -10.58054468882281363, -13.33752895606068201, 71.31714512707709730 ) ) ;
#31573 = ORIENTED_EDGE ( 'NONE', *, *, #41350, .T. ) ;
#31574 = CARTESIAN_POINT ( 'NONE',  ( -41.04982914953070861, -14.80920654474427600, 73.99411764705880046 ) ) ;
#31575 = CARTESIAN_POINT ( 'NONE',  ( -22.47381490279794036, -20.28691852675989793, 65.84388348312960204 ) ) ;
#31576 = DIRECTION ( 'NONE',  ( 0.000000000000000000, -0.9999954153791273948, -0.003028072113819838245 ) ) ;
#31577 = ORIENTED_EDGE ( 'NONE', *, *, #8386, .T. ) ;
#31578 = DIRECTION ( 'NONE',  ( -1.000000000000000000, -2.866981220435666553E-17, -0.000000000000000000 ) ) ;
#31579 = FACE_OUTER_BOUND ( 'NONE', #9447, .T. ) ;
#31580 = CARTESIAN_POINT ( 'NONE',  ( -22.17253171379126897, -20.54993857985014216, 59.02088830234949057 ) ) ;
#31581 = AXIS2_PLACEMENT_3D ( 'NONE', #40104, #47495, #29260 ) ;
#31582 = EDGE_CURVE ( 'NONE', #2353, #41372, #16504, .T. ) ;
#31583 =( BOUNDED_CURVE ( )  B_SPLINE_CURVE ( 3, ( #27957, #4836, #11985, #16382 ),
 .UNSPECIFIED., .F., .F. ) 
 B_SPLINE_CURVE_WITH_KNOTS ( ( 4, 4 ),
 ( 0.000000000000000000, 0.4074455897393663428 ),
 .UNSPECIFIED. ) 
 CURVE ( )  GEOMETRIC_REPRESENTATION_ITEM ( )  RATIONAL_B_SPLINE_CURVE ( ( 1.000000000000000000, 0.4567392136813290815, 0.3561768502900292122, 0.6983129098261003920 ) ) 
 REPRESENTATION_ITEM ( '' )  );
#31584 = CARTESIAN_POINT ( 'NONE',  ( -15.62101046192594289, -7.580605815997546237, 70.72494447658496597 ) ) ;
#31585 = DIRECTION ( 'NONE',  ( -6.258914682829359833E-07, 5.777405174637831559E-07, 0.9999999999996371791 ) ) ;
#31586 = CARTESIAN_POINT ( 'NONE',  ( -20.60910058366379616, -21.04276686425195919, 58.94475179565701950 ) ) ;
#31587 = EDGE_LOOP ( 'NONE', ( #29492, #26636, #46942, #36564, #11386 ) ) ;
#31588 = FACE_OUTER_BOUND ( 'NONE', #5358, .T. ) ;
#31589 = CARTESIAN_POINT ( 'NONE',  ( -36.42409385541304800, -6.859212275519750435, 50.50378509014258555 ) ) ;
#31590 = CARTESIAN_POINT ( 'NONE',  ( -16.20950590255762691, -7.458868724970470154, 60.30054238772634534 ) ) ;
#31591 = B_SPLINE_CURVE_WITH_KNOTS ( 'NONE', 3,
 ( #24542, #20098, #20828, #47174, #5582, #46205, #42991, #42521, #16868, #31183 ),
 .UNSPECIFIED., .F., .F.,
 ( 4, 2, 2, 2, 4 ),
 ( 0.1272669073658357908, 0.2522669073463156275, 0.3772669073267955198, 0.5022669073072754120, 0.6272669072877552487 ),
 .UNSPECIFIED. ) ;
#31592 = DIRECTION ( 'NONE',  ( -0.1464579420318390945, 0.9892168979631277281, 7.284849527811297202E-08 ) ) ;
#31593 = CARTESIAN_POINT ( 'NONE',  ( -14.14556133858745390, -20.99403164004895217, 71.94110109989711077 ) ) ;
#31594 = CARTESIAN_POINT ( 'NONE',  ( -17.46159385650551599, -9.295667164867525756, 49.30633214617472504 ) ) ;
#31595 = PRODUCT_RELATED_PRODUCT_CATEGORY ( 'part', '', ( #23692 ) ) ;
#31596 = VECTOR ( 'NONE', #4697, 1000.000000000000000 ) ;
#31597 = EDGE_LOOP ( 'NONE', ( #19494, #21735, #16528, #44980, #20692 ) ) ;
#31598 = DIRECTION ( 'NONE',  ( -3.071710424422018668E-17, 6.404604876783312462E-16, 1.000000000000000000 ) ) ;
#31599 = FACE_OUTER_BOUND ( 'NONE', #45169, .T. ) ;
#31600 = ORIENTED_EDGE ( 'NONE', *, *, #38960, .F. ) ;
#31601 = CARTESIAN_POINT ( 'NONE',  ( -24.37683887807358474, -15.97618392648307584, 66.36324926629207255 ) ) ;
#31602 = CARTESIAN_POINT ( 'NONE',  ( -15.49415775405465645, -8.028509947901662613, 74.37985659017799378 ) ) ;
#31603 = CARTESIAN_POINT ( 'NONE',  ( -12.74071780128996423, -9.015264284427722430, 70.96430057504635158 ) ) ;
#31604 = CARTESIAN_POINT ( 'NONE',  ( -11.03124120290388532, -17.66077365132053956, 71.86718193465377169 ) ) ;
#31605 = FACE_OUTER_BOUND ( 'NONE', #34941, .T. ) ;
#31606 =( BOUNDED_SURFACE ( )  B_SPLINE_SURFACE ( 3, 1, ( 
 ( #18710, #37667 ),
 ( #11098, #41133 ),
 ( #22417, #44590 ),
 ( #33721, #10845 ),
 ( #7664, #25867 ),
 ( #37411, #29322 ),
 ( #40884, #7415 ) ),
 .UNSPECIFIED., .T., .F., .F. ) 
 B_SPLINE_SURFACE_WITH_KNOTS ( ( 4, 3, 4 ),
 ( 2, 2 ),
 ( 0.000000000000000000, 0.5000000000000000000, 1.000000000000000000 ),
 ( 0.000000000000000000, 1.000000000000000000 ),
 .UNSPECIFIED. ) 
 GEOMETRIC_REPRESENTATION_ITEM ( )  RATIONAL_B_SPLINE_SURFACE ( (
 ( 1.000000000000000000, 1.000000000000000000),
 ( 0.3333333333333335369, 0.3333333333333330373),
 ( 0.3333333333333335369, 0.3333333333333330373),
 ( 1.000000000000000000, 1.000000000000000000),
 ( 0.3333333333333333703, 0.3333333333333333703),
 ( 0.3333333333333333703, 0.3333333333333333703),
 ( 1.000000000000000000, 1.000000000000000000) ) ) 
 REPRESENTATION_ITEM ( '' )  SURFACE ( )  );
#31607 = ORIENTED_EDGE ( 'NONE', *, *, #31025, .T. ) ;
#31608 =( BOUNDED_CURVE ( )  B_SPLINE_CURVE ( 3, ( #8469, #23750, #19804, #41719 ),
 .UNSPECIFIED., .F., .F. ) 
 B_SPLINE_CURVE_WITH_KNOTS ( ( 4, 4 ),
 ( 0.4074455897393575166, 0.5000000000000000000 ),
 .UNSPECIFIED. ) 
 CURVE ( )  GEOMETRIC_REPRESENTATION_ITEM ( )  RATIONAL_B_SPLINE_CURVE ( ( 0.6983129098260714152, 0.7760317562606667829, 0.8765941196519724254, 0.9999999999999796829 ) ) 
 REPRESENTATION_ITEM ( '' )  );
#31609 = CARTESIAN_POINT ( 'NONE',  ( -24.47401588645412573, -14.84236399432835540, 59.39300237059229914 ) ) ;
#31610 = CARTESIAN_POINT ( 'NONE',  ( -10.85841931818429629, -17.37798394237198707, 64.91267318220633342 ) ) ;
#31611 = VECTOR ( 'NONE', #7102, 1000.000000000000000 ) ;
#31612 = CARTESIAN_POINT ( 'NONE',  ( -18.96810653497118437, -7.981552352277012652, 63.50377208636563608 ) ) ;
#31613 = ORIENTED_EDGE ( 'NONE', *, *, #13484, .T. ) ;
#31614 = CARTESIAN_POINT ( 'NONE',  ( -18.58222256244375714, -22.16864733340743143, 72.48499710573040034 ) ) ;
#31615 = AXIS2_PLACEMENT_3D ( 'NONE', #11379, #41413, #22718 ) ;
#31616 = CARTESIAN_POINT ( 'NONE',  ( -13.42842659190323751, -9.059672259974458797, 64.09873707138190468 ) ) ;
#31617 = CARTESIAN_POINT ( 'NONE',  ( -17.42409385541299471, -14.80920654474435771, 49.52966884056655772 ) ) ;
#31618 = ADVANCED_FACE ( 'NONE', ( #35833 ), #35113, .T. ) ;
#31619 = CARTESIAN_POINT ( 'NONE',  ( -15.55171241031346696, -7.598245096497682205, 70.79485117658632021 ) ) ;
#31620 = B_SPLINE_CURVE_WITH_KNOTS ( 'NONE', 3,
 ( #18802, #108, #15093, #11413, #20986, #43649, #27887, #31590, #17022, #1542 ),
 .UNSPECIFIED., .F., .F.,
 ( 4, 2, 2, 2, 4 ),
 ( 0.6272669072877363750, 0.7522669073072645318, 0.8772669073267927997, 1.002266907346321068, 1.127266907365849224 ),
 .UNSPECIFIED. ) ;
#31621 = FACE_OUTER_BOUND ( 'NONE', #2916, .T. ) ;
#31622 =( BOUNDED_CURVE ( )  B_SPLINE_CURVE ( 3, ( #11656, #34051, #16297, #5009 ),
 .UNSPECIFIED., .F., .F. ) 
 B_SPLINE_CURVE_WITH_KNOTS ( ( 4, 4 ),
 ( 0.9074455897393666204, 1.000000000000000000 ),
 .UNSPECIFIED. ) 
 CURVE ( )  GEOMETRIC_REPRESENTATION_ITEM ( )  RATIONAL_B_SPLINE_CURVE ( ( 0.6983129098260977274, 0.7760317562607021991, 0.8765941196520029566, 1.000000000000000000 ) ) 
 REPRESENTATION_ITEM ( '' )  );
#31623 = ORIENTED_EDGE ( 'NONE', *, *, #4235, .T. ) ;
#31624 = ORIENTED_EDGE ( 'NONE', *, *, #3993, .F. ) ;
#31625 = CARTESIAN_POINT ( 'NONE',  ( -23.31159385541304019, -8.990409506049200417, 49.61344411288074951 ) ) ;
#31626 = CARTESIAN_POINT ( 'NONE',  ( -19.15588758283814386, -7.975065456818123621, 63.43649048405502811 ) ) ;
#31627 = CARTESIAN_POINT ( 'NONE',  ( -11.76425449931685030, -10.60075661872682140, 70.85404331479517737 ) ) ;
#31628 = FACE_OUTER_BOUND ( 'NONE', #30705, .T. ) ;
#31629 = CARTESIAN_POINT ( 'NONE',  ( -24.31294276048392078, -17.64623836558455494, 66.10503720318618548 ) ) ;
#31630 = EDGE_CURVE ( 'NONE', #5074, #17144, #16399, .T. ) ;
#31632 = CARTESIAN_POINT ( 'NONE',  ( -10.37182134788606369, -14.70778158825885207, 67.74311464738552502 ) ) ;
#31631 = B_SPLINE_CURVE_WITH_KNOTS ( 'NONE', 3,
 ( #48556, #20827, #2108, #22222, #25913, #21068 ),
 .UNSPECIFIED., .F., .F.,
 ( 4, 2, 4 ),
 ( 0.2909959651135547443, 0.4999962229283157478, 0.7089964807430767513 ),
 .UNSPECIFIED. ) ;
#31633 = CARTESIAN_POINT ( 'NONE',  ( -24.41897112398753933, -17.37347453850100720, 69.59835118672229726 ) ) ;
#31634 = ADVANCED_FACE ( 'NONE', ( #46701 ), #16646, .T. ) ;
#31635 = EDGE_LOOP ( 'NONE', ( #11582, #31707 ) ) ;
#31636 = CARTESIAN_POINT ( 'NONE',  ( -24.15060978519040091, -18.01196315242050261, 59.26024333157867119 ) ) ;
#31637 = CARTESIAN_POINT ( 'NONE',  ( -17.04628442466378502, -7.819299381639010171, 74.26018289601994127 ) ) ;
#31638 = B_SPLINE_CURVE_WITH_KNOTS ( 'NONE', 3,
 ( #45497, #202, #4137, #4603, #7343, #22342, #11754, #33643, #11270, #7582 ),
 .UNSPECIFIED., .F., .F.,
 ( 4, 2, 2, 2, 4 ),
 ( 0.6272669072877816721, 0.7522669073072908441, 0.8772669073268000162, 1.002266907346309299, 1.127266907365818360 ),
 .UNSPECIFIED. ) ;
#31639 = ORIENTED_EDGE ( 'NONE', *, *, #4077, .F. ) ;
#31640 = ADVANCED_FACE ( 'NONE', ( #35363 ), #12946, .T. ) ;
#31641 = CARTESIAN_POINT ( 'NONE',  ( -10.44916082259176093, -15.83527127794237543, 64.80771589743309846 ) ) ;
#31642 = ORIENTED_EDGE ( 'NONE', *, *, #21287, .F. ) ;
#31643 = CARTESIAN_POINT ( 'NONE',  ( -17.70936732686351789, -22.25382107568847800, 58.66199285276312025 ) ) ;
#31644 = CARTESIAN_POINT ( 'NONE',  ( -10.00315453233114305, -15.46673966334550521, 57.66818560559547535 ) ) ;
#31645 = EDGE_CURVE ( 'NONE', #7173, #40988, #34462, .T. ) ;
#31646 = CARTESIAN_POINT ( 'NONE',  ( -10.34160677812053208, -12.49813974654896320, 60.89829944146450913 ) ) ;
#31647 = CARTESIAN_POINT ( 'NONE',  ( -13.99679447977218061, -20.97040113148658591, 71.94079819673058296 ) ) ;
#31648 = VERTEX_POINT ( 'NONE', #1875 ) ;
#31649 = CARTESIAN_POINT ( 'NONE',  ( -13.88631413956031579, -11.73554473314222157, 49.52966884056655772 ) ) ;
#31650 = LINE ( 'NONE', #47633, #43932 ) ;
#31651 = ADVANCED_FACE ( 'NONE', ( #10244 ), #25259, .T. ) ;
#31652 = CARTESIAN_POINT ( 'NONE',  ( -17.04413539470110095, -21.84925844046378174, 72.45071136019464575 ) ) ;
#31653 = DIRECTION ( 'NONE',  ( -9.941263206155103325E-06, -7.040377910290660294E-06, 0.9999999999258021299 ) ) ;
#31654 = CARTESIAN_POINT ( 'NONE',  ( -21.00733138479494855, -11.77013360165372013, 49.52966884056655772 ) ) ;
#31655 = DIRECTION ( 'NONE',  ( 0.9687793358424821033, -0.2479245821708677133, 0.000000000000000000 ) ) ;
#31656 = CARTESIAN_POINT ( 'NONE',  ( -23.80321479583337307, -17.81075880182941873, 59.30378417737343710 ) ) ;
#31657 = VERTEX_POINT ( 'NONE', #14608 ) ;
#31658 = LINE ( 'NONE', #38545, #8741 ) ;
#31659 = CARTESIAN_POINT ( 'NONE',  ( -11.55820670847359821, -18.73429759261662397, 71.83119032172525920 ) ) ;
#31660 = LINE ( 'NONE', #24275, #32178 ) ;
#31661 = VERTEX_POINT ( 'NONE', #22284 ) ;
#31662 = CARTESIAN_POINT ( 'NONE',  ( -19.92776479198160189, -21.39998277484045275, 72.41950795000725805 ) ) ;
#31663 = FACE_BOUND ( 'NONE', #13716, .T. ) ;
#31664 = ORIENTED_EDGE ( 'NONE', *, *, #7328, .F. ) ;
#31665 = ORIENTED_EDGE ( 'NONE', *, *, #13065, .T. ) ;
#31666 = VERTEX_POINT ( 'NONE', #3077 ) ;
#31667 = CARTESIAN_POINT ( 'NONE',  ( -28.42409385541305511, -6.359206544744109735, 52.99999999999997158 ) ) ;
#31668 = LINE ( 'NONE', #43242, #20857 ) ;
#31669 = EDGE_CURVE ( 'NONE', #36512, #11228, #2831, .T. ) ;
#31670 = CARTESIAN_POINT ( 'NONE',  ( -45.92409385541306222, -14.20920654474410760, 70.50000000000000000 ) ) ;
#31671 = CARTESIAN_POINT ( 'NONE',  ( -12.62620107223973243, -19.90688791973824578, 68.62040837454712516 ) ) ;
#31672 = ORIENTED_EDGE ( 'NONE', *, *, #9153, .T. ) ;
#31673 = ORIENTED_EDGE ( 'NONE', *, *, #4985, .F. ) ;
#31674 = B_SPLINE_CURVE_WITH_KNOTS ( 'NONE', 3,
 ( #8755, #39743, #32370, #39505, #16832, #47388, #8988, #47141, #9721, #39012 ),
 .UNSPECIFIED., .F., .F.,
 ( 4, 2, 2, 2, 4 ),
 ( 0.000000000000000000, 0.2500000000000000000, 0.5000000000000000000, 0.7500000000000000000, 1.000000000000000000 ),
 .UNSPECIFIED. ) ;
#31675 = CARTESIAN_POINT ( 'NONE',  ( -23.17409385650551457, -9.792211528768504536, 50.49490371617623197 ) ) ;
#31676 = CARTESIAN_POINT ( 'NONE',  ( -21.39967327233876659, -20.63170314183283693, 72.80974286114339122 ) ) ;
#31677 = CARTESIAN_POINT ( 'NONE',  ( -24.87377682536729750, -14.89413262103416002, 59.40446719508604190 ) ) ;
#31678 = CARTESIAN_POINT ( 'NONE',  ( -23.27832888692776336, -18.64690537560570860, 65.93275336871789705 ) ) ;
#31679 = CARTESIAN_POINT ( 'NONE',  ( -21.43034385650551954, -9.794322478646142471, 51.19202720610083901 ) ) ;
#31680 = EDGE_CURVE ( 'NONE', #31825, #29639, #40943, .T. ) ;
#31681 = ORIENTED_EDGE ( 'NONE', *, *, #21206, .T. ) ;
#31682 = CARTESIAN_POINT ( 'NONE',  ( -41.79100562011894482, -14.80920654474410547, 68.06470588235292496 ) ) ;
#31683 = CARTESIAN_POINT ( 'NONE',  ( -33.95962776134579286, -8.109206544744111511, 49.25000000000000000 ) ) ;
#31684 = CARTESIAN_POINT ( 'NONE',  ( -17.35617175722243744, -7.809413396383948935, 67.32039598645116030 ) ) ;
#31685 =( BOUNDED_CURVE ( )  B_SPLINE_CURVE ( 3, ( #47988, #14226, #21880, #36880 ),
 .UNSPECIFIED., .F., .F. ) 
 B_SPLINE_CURVE_WITH_KNOTS ( ( 4, 4 ),
 ( 0.9074455897393720605, 1.000000000000000000 ),
 .UNSPECIFIED. ) 
 CURVE ( )  GEOMETRIC_REPRESENTATION_ITEM ( )  RATIONAL_B_SPLINE_CURVE ( ( 0.6983129098261073864, 0.7760317562607105257, 0.8765941196520080636, 1.000000000000000000 ) ) 
 REPRESENTATION_ITEM ( '' )  );
#31686 = VERTEX_POINT ( 'NONE', #3324 ) ;
#31687 = LINE ( 'NONE', #5833, #30442 ) ;
#31688 = ADVANCED_FACE ( 'NONE', ( #25981 ), #36786, .T. ) ;
#31689 = CARTESIAN_POINT ( 'NONE',  ( -10.37172597770583415, -14.90377323363781414, 71.21294082064301278 ) ) ;
#31690 = CARTESIAN_POINT ( 'NONE',  ( -18.71951286714620011, -7.876189896296080128, 66.78582905748461940 ) ) ;
#31691 = CIRCLE ( 'NONE', #10475, 0.3999999999999975797 ) ;
#31692 = EDGE_CURVE ( 'NONE', #12494, #35872, #18866, .T. ) ;
#31693 = ORIENTED_EDGE ( 'NONE', *, *, #8954, .T. ) ;
#31694 = CARTESIAN_POINT ( 'NONE',  ( -14.84764829735760827, -8.246537290690364230, 60.33468334944129197 ) ) ;
#31695 = CARTESIAN_POINT ( 'NONE',  ( -22.88305391114024800, -19.19300254727433597, 59.11240555529296614 ) ) ;
#31696 = CARTESIAN_POINT ( 'NONE',  ( -11.44812231001245095, -18.45465661085254538, 61.57710877958685103 ) ) ;
#31697 = ORIENTED_EDGE ( 'NONE', *, *, #19073, .T. ) ;
#31698 = FACE_OUTER_BOUND ( 'NONE', #40146, .T. ) ;
#31699 = ORIENTED_EDGE ( 'NONE', *, *, #13124, .T. ) ;
#31700 = CARTESIAN_POINT ( 'NONE',  ( -24.42398663107514523, -15.65075326911586906, 73.01775867260030850 ) ) ;
#31701 = DIRECTION ( 'NONE',  ( 2.866981220435666553E-17, -1.000000000000000000, -1.190614954331866791E-16 ) ) ;
#31702 = EDGE_LOOP ( 'NONE', ( #21083, #39885, #32268, #6010, #10830 ) ) ;
#31703 = CARTESIAN_POINT ( 'NONE',  ( -22.17130234749883044, -20.55096496926394778, 58.87947491310501391 ) ) ;
#31704 = CYLINDRICAL_SURFACE ( 'NONE', #43650, 5.249999999999998224 ) ;
#31705 = CARTESIAN_POINT ( 'NONE',  ( -17.06879511326789611, -7.767867012253359071, 73.97490359703523666 ) ) ;
#31706 = FACE_BOUND ( 'NONE', #26987, .T. ) ;
#31707 = ORIENTED_EDGE ( 'NONE', *, *, #39968, .T. ) ;
#31708 = FACE_OUTER_BOUND ( 'NONE', #39033, .T. ) ;
#31709 = UNCERTAINTY_MEASURE_WITH_UNIT (LENGTH_MEASURE( 1.000000000000000082E-05 ), #26344, 'distance_accuracy_value', 'NONE');
#31710 = DIRECTION ( 'NONE',  ( -3.071710424422018668E-17, 6.404604876783312462E-16, 1.000000000000000000 ) ) ;
#31712 = EDGE_CURVE ( 'NONE', #17470, #891, #6544, .T. ) ;
#31711 = CARTESIAN_POINT ( 'NONE',  ( -23.41687109752707840, -19.23545012094337991, 62.49373545795776863 ) ) ;
#31713 = ORIENTED_EDGE ( 'NONE', *, *, #12149, .F. ) ;
#31714 = CARTESIAN_POINT ( 'NONE',  ( -15.81235419205221859, -7.945607373518419614, 67.42535135806457447 ) ) ;
#31715 = EDGE_CURVE ( 'NONE', #44810, #39108, #35487, .T. ) ;
#31716 = DIRECTION ( 'NONE',  ( 3.413470714839332458E-33, -1.190614954331866791E-16, 1.000000000000000000 ) ) ;
#31717 = EDGE_CURVE ( 'NONE', #11465, #39185, #37040, .T. ) ;
#31718 = EDGE_CURVE ( 'NONE', #5083, #46221, #544, .T. ) ;
#31719 = ADVANCED_FACE ( 'NONE', ( #29191 ), #44232, .T. ) ;
#31720 = VERTEX_POINT ( 'NONE', #11214 ) ;
#31721 = ORIENTED_EDGE ( 'NONE', *, *, #35044, .F. ) ;
#31722 = CARTESIAN_POINT ( 'NONE',  ( -14.25195992805637246, -21.10928659929985685, 72.13427513627219412 ) ) ;
#31723 = DIRECTION ( 'NONE',  ( 2.866981220435666553E-17, -1.000000000000000000, -1.190614954331866791E-16 ) ) ;
#31724 = FACE_OUTER_BOUND ( 'NONE', #30166, .T. ) ;
#31725 = B_SPLINE_CURVE_WITH_KNOTS ( 'NONE', 3,
 ( #43108, #27604, #5698, #16510, #1982, #12340, #1022, #38430, #27359, #4718 ),
 .UNSPECIFIED., .F., .F.,
 ( 4, 2, 2, 2, 4 ),
 ( 0.000000000000000000, 0.2500000000000000000, 0.5000000000000000000, 0.7500000000000000000, 1.000000000000000000 ),
 .UNSPECIFIED. ) ;
#31726 = CARTESIAN_POINT ( 'NONE',  ( -18.36159385650551812, -9.295667164867525756, 49.30633214617472504 ) ) ;
#31727 = CARTESIAN_POINT ( 'NONE',  ( -16.19813999035177332, -21.75179513556690480, 58.28585572029250983 ) ) ;
#31728 = LINE ( 'NONE', #12992, #10248 ) ;
#31729 = CARTESIAN_POINT ( 'NONE',  ( -18.34288178775629419, -10.21365315202000446, 49.52966884056655772 ) ) ;
#31730 = CARTESIAN_POINT ( 'NONE',  ( -22.79947183316497217, -19.38307604245925475, 59.02843669344121480 ) ) ;
#31731 = ORIENTED_EDGE ( 'NONE', *, *, #36083, .F. ) ;
#31732 = ORIENTED_EDGE ( 'NONE', *, *, #32261, .T. ) ;
#31733 = FACE_OUTER_BOUND ( 'NONE', #17781, .T. ) ;
#31734 =( LENGTH_UNIT ( ) NAMED_UNIT ( * ) SI_UNIT ( .MILLI., .METRE. ) );
#31735 = AXIS2_PLACEMENT_3D ( 'NONE', #36513, #2799, #47866 ) ;
#31736 = CARTESIAN_POINT ( 'NONE',  ( -21.70267066777908838, -12.86772875551264050, 49.52966884056655772 ) ) ;
#31737 = CARTESIAN_POINT ( 'NONE',  ( -19.70791841144649581, -21.90059652173849969, 65.72132139802793915 ) ) ;
#31738 = PLANE ( 'NONE',  #7591 ) ;
#31739 = CARTESIAN_POINT ( 'NONE',  ( -20.60942684424193772, -21.09890871138989965, 58.65947248567252359 ) ) ;
#31740 =( BOUNDED_CURVE ( )  B_SPLINE_CURVE ( 3, ( #1513, #31559, #12836, #13063 ),
 .UNSPECIFIED., .F., .F. ) 
 B_SPLINE_CURVE_WITH_KNOTS ( ( 4, 4 ),
 ( 0.9074455897393626236, 1.000000000000000000 ),
 .UNSPECIFIED. ) 
 CURVE ( )  GEOMETRIC_REPRESENTATION_ITEM ( )  RATIONAL_B_SPLINE_CURVE ( ( 0.6983129098260858481, 0.7760317562606919850, 0.8765941196519967393, 1.000000000000000000 ) ) 
 REPRESENTATION_ITEM ( '' )  );
#31741 = ORIENTED_EDGE ( 'NONE', *, *, #13484, .F. ) ;
#31742 = EDGE_CURVE ( 'NONE', #21230, #44055, #10602, .T. ) ;
#31743 = CARTESIAN_POINT ( 'NONE',  ( -15.06802786744574085, -21.40078853851168716, 61.74486554635382163 ) ) ;
#31744 = CARTESIAN_POINT ( 'NONE',  ( -24.00405284133622175, -11.31538449050870021, 66.52190887339411063 ) ) ;
#31745 = CARTESIAN_POINT ( 'NONE',  ( -14.92297820767285543, -21.82695172143102624, 65.28409420478728009 ) ) ;
#31746 = CARTESIAN_POINT ( 'NONE',  ( -24.48810873059073856, -17.17637193698283582, 73.06831349224263761 ) ) ;
#31747 = EDGE_LOOP ( 'NONE', ( #38675, #41626, #29971, #46109 ) ) ;
#31748 =( BOUNDED_CURVE ( )  B_SPLINE_CURVE ( 3, ( #43411, #38968, #16789, #8946 ),
 .UNSPECIFIED., .F., .F. ) 
 B_SPLINE_CURVE_WITH_KNOTS ( ( 4, 4 ),
 ( 0.000000000000000000, 0.4074455897393660653 ),
 .UNSPECIFIED. ) 
 CURVE ( )  GEOMETRIC_REPRESENTATION_ITEM ( )  RATIONAL_B_SPLINE_CURVE ( ( 1.000000000000000000, 0.4567392136813301917, 0.3561768502900296562, 0.6983129098260982826 ) ) 
 REPRESENTATION_ITEM ( '' )  );
#31749 = CARTESIAN_POINT ( 'NONE',  ( -24.40836465796088106, -14.33371513455089641, 69.66891893576270434 ) ) ;
#31750 = CARTESIAN_POINT ( 'NONE',  ( -24.79803955827340545, -15.87155823828966561, 69.78953433284350183 ) ) ;
#31751 = EDGE_CURVE ( 'NONE', #29409, #30363, #40503, .T. ) ;
#31752 = CARTESIAN_POINT ( 'NONE',  ( -10.15209110106313695, -13.18697342404853146, 74.86472985364514443 ) ) ;
#31753 = FACE_OUTER_BOUND ( 'NONE', #40193, .T. ) ;
#31754 = CARTESIAN_POINT ( 'NONE',  ( -22.33034385759799179, -6.857644439848018969, 49.98602051094138687 ) ) ;
#31755 = VERTEX_POINT ( 'NONE', #41003 ) ;
#31756 = CARTESIAN_POINT ( 'NONE',  ( -14.91112529534803066, -8.221969756899694559, 57.13527940342243028 ) ) ;
#31757 = VERTEX_POINT ( 'NONE', #29427 ) ;
#31758 = CARTESIAN_POINT ( 'NONE',  ( -10.01516485041080884, -14.02680443569644098, 61.04104412929918055 ) ) ;
#31759 = CARTESIAN_POINT ( 'NONE',  ( -10.42420408449255476, -14.84849159528415541, 71.43668796657122755 ) ) ;
#31760 = VERTEX_POINT ( 'NONE', #25729 ) ;
#31761 = CARTESIAN_POINT ( 'NONE',  ( -16.31151605585062825, -19.37404237808139484, 49.52966884056656482 ) ) ;
#31762 = VECTOR ( 'NONE', #36046, 1000.000000000000000 ) ;
#31763 = CARTESIAN_POINT ( 'NONE',  ( -17.43659385650551741, -6.915538690918075382, 49.31353937987644542 ) ) ;
#31764 = ORIENTED_EDGE ( 'NONE', *, *, #35914, .F. ) ;
#31765 = DIRECTION ( 'NONE',  ( 0.9986807914369958405, -0.05134858142905002198, 1.286972170232540014E-09 ) ) ;
#31766 = CARTESIAN_POINT ( 'NONE',  ( -14.91112529534803066, -8.221969756899694559, 57.13527940342243028 ) ) ;
#31767 = CARTESIAN_POINT ( 'NONE',  ( -13.62794895237762027, -8.864113615554126469, 60.73950575333512347 ) ) ;
#31768 = EDGE_LOOP ( 'NONE', ( #37337, #1426, #34773, #33665 ) ) ;
#31769 = CARTESIAN_POINT ( 'NONE',  ( -16.27008067537174796, -7.904986561263926959, 60.50028479261354875 ) ) ;
#31770 = CARTESIAN_POINT ( 'NONE',  ( -10.71605034603323148, -17.00400043661996108, 64.77172137060364321 ) ) ;
#31771 = B_SPLINE_CURVE_WITH_KNOTS ( 'NONE', 1,
 ( #33071, #352 ),
 .UNSPECIFIED., .F., .F.,
 ( 2, 2 ),
 ( 0.000000000000000000, 1.000000000000000000 ),
 .UNSPECIFIED. ) ;
#31772 = CARTESIAN_POINT ( 'NONE',  ( -12.94748490290780829, -9.362827855744063399, 71.14925333309587074 ) ) ;
#31773 = ADVANCED_FACE ( 'NONE', ( #7028 ), #22046, .T. ) ;
#31774 = EDGE_CURVE ( 'NONE', #15165, #47561, #8483, .T. ) ;
#31775 = ORIENTED_EDGE ( 'NONE', *, *, #28360, .F. ) ;
#31776 = VERTEX_POINT ( 'NONE', #35481 ) ;
#31777 = CARTESIAN_POINT ( 'NONE',  ( -17.59331747086620368, -7.761237804118463757, 63.85057029381062677 ) ) ;
#31778 = CARTESIAN_POINT ( 'NONE',  ( -13.09267315849321456, -9.242013884934323187, 63.90946244383246011 ) ) ;
#31779 = EDGE_LOOP ( 'NONE', ( #26754, #11124, #31672, #765, #2254 ) ) ;
#31780 = DIRECTION ( 'NONE',  ( -0.000000000000000000, -1.000000000000000000, -0.000000000000000000 ) ) ;
#31781 = DIRECTION ( 'NONE',  ( -1.000000000000000000, -2.866981220435666553E-17, 0.000000000000000000 ) ) ;
#31782 = CARTESIAN_POINT ( 'NONE',  ( -17.71784385759799108, -6.860780111191487229, 51.02154966934377001 ) ) ;
#31783 = CARTESIAN_POINT ( 'NONE',  ( -13.07701721570114373, -8.758813871092014480, 64.08759315826752356 ) ) ;
#31784 = CARTESIAN_POINT ( 'NONE',  ( -9.424093855413055110, -27.10920654474410796, 54.99999999999997868 ) ) ;
#31785 = DIRECTION ( 'NONE',  ( -1.069388061899112173E-05, 2.778940573026428581E-06, 0.9999999999389591609 ) ) ;
#31786 = ORIENTED_EDGE ( 'NONE', *, *, #44375, .F. ) ;
#31787 = ADVANCED_FACE ( 'NONE', ( #1764 ), #12687, .T. ) ;
#31788 = EDGE_CURVE ( 'NONE', #41843, #42966, #31801, .T. ) ;
#31789 = DIRECTION ( 'NONE',  ( -0.000000000000000000, -1.000000000000000000, -0.000000000000000000 ) ) ;
#31790 = CARTESIAN_POINT ( 'NONE',  ( -13.00736322368352305, -8.809467263174131091, 64.08663386113011029 ) ) ;
#31791 = CARTESIAN_POINT ( 'NONE',  ( -10.45263246496396370, -15.85887054471568014, 64.80771565453923699 ) ) ;
#31792 = CARTESIAN_POINT ( 'NONE',  ( -23.71751471349159601, -11.63122711669449494, 63.23746208799618529 ) ) ;
#31793 = CARTESIAN_POINT ( 'NONE',  ( -10.79968008669509594, -11.40033872506984203, 67.72526294861705765 ) ) ;
#31794 = VERTEX_POINT ( 'NONE', #12177 ) ;
#31795 = VERTEX_POINT ( 'NONE', #41480 ) ;
#31796 = AXIS2_PLACEMENT_3D ( 'NONE', #31609, #27666, #28151 ) ;
#31797 = VERTEX_POINT ( 'NONE', #15610 ) ;
#31798 = EDGE_CURVE ( 'NONE', #38648, #24162, #23589, .T. ) ;
#31799 = CARTESIAN_POINT ( 'NONE',  ( -20.37299732318518508, -8.405577239842552117, 66.93104082189577753 ) ) ;
#31800 = TOROIDAL_SURFACE ( 'NONE', #18416, 1.000000000000001332, 0.5000000000000000000 ) ;
#31801 = LINE ( 'NONE', #34573, #39436 ) ;
#31802 = CARTESIAN_POINT ( 'NONE',  ( -24.11794058161805054, -12.76166764465371628, 69.77243002474142486 ) ) ;
#31803 = ORIENTED_EDGE ( 'NONE', *, *, #27340, .T. ) ;
#31804 = CARTESIAN_POINT ( 'NONE',  ( -22.01092588021961660, -8.937695967300268052, 66.84805351483468883 ) ) ;
#31805 = CARTESIAN_POINT ( 'NONE',  ( -10.00117635412376593, -15.44487469174752903, 57.68297500625912733 ) ) ;
#31807 = EDGE_LOOP ( 'NONE', ( #30202, #47679 ) ) ;
#31806 = MANIFOLD_SOLID_BREP ( 'Stock-MAS-175-1', #14937 ) ;
#31808 = DIRECTION ( 'NONE',  ( 0.9687793358424821033, -0.2479245821708680464, 0.000000000000000000 ) ) ;
#31809 = CARTESIAN_POINT ( 'NONE',  ( -18.91460061187875397, -21.70800071742875303, 58.66940498489888256 ) ) ;
#31810 = VERTEX_POINT ( 'NONE', #37783 ) ;
#31811 = FACE_OUTER_BOUND ( 'NONE', #12798, .T. ) ;
#31812 = VERTEX_POINT ( 'NONE', #19566 ) ;
#31813 = CARTESIAN_POINT ( 'NONE',  ( -10.12183752415379168, -13.33225746603075024, 74.80004878148187686 ) ) ;
#31814 = ORIENTED_EDGE ( 'NONE', *, *, #24281, .F. ) ;
#31815 = FACE_BOUND ( 'NONE', #36263, .T. ) ;
#31816 = DIRECTION ( 'NONE',  ( 1.000000000000000000, -0.000000000000000000, 2.081668171172170091E-15 ) ) ;
#31817 = CARTESIAN_POINT ( 'NONE',  ( -19.30128557755455532, -21.60500301973953086, 58.81035253397666196 ) ) ;
#31818 = EDGE_LOOP ( 'NONE', ( #1490, #36402, #30340, #9014, #36798 ) ) ;
#31819 = CYLINDRICAL_SURFACE ( 'NONE', #8157, 1.250000000000001110 ) ;
#31820 = CARTESIAN_POINT ( 'NONE',  ( -24.70020460095737391, -16.41001677332389619, 59.30049291089687102 ) ) ;
#31821 = CARTESIAN_POINT ( 'NONE',  ( -20.18941624216641273, -7.891347737435665977, 73.83601159825586535 ) ) ;
#31822 = CARTESIAN_POINT ( 'NONE',  ( -13.66248979885904724, -8.905658713984221819, 56.96967804944289071 ) ) ;
#31823 = CARTESIAN_POINT ( 'NONE',  ( -17.79108452803360763, -21.84994637594637368, 58.69081321602850920 ) ) ;
#31824 = CARTESIAN_POINT ( 'NONE',  ( -14.97188219925329378, -8.199429090594037461, 57.14999999999994884 ) ) ;
#31825 = VERTEX_POINT ( 'NONE', #4310 ) ;
#31826 = LINE ( 'NONE', #39936, #40395 ) ;
#31827 = CARTESIAN_POINT ( 'NONE',  ( -24.66897215040500768, -13.07252427436380238, 63.01076963004065590 ) ) ;
#31828 = DIRECTION ( 'NONE',  ( -1.420801289120338746E-06, -1.008342286982562053E-05, 0.9999999999481529178 ) ) ;
#31829 = CIRCLE ( 'NONE', #23967, 0.6570903894995150374 ) ;
#31830 = CARTESIAN_POINT ( 'NONE',  ( -14.39999285742539392, -8.436745619719848932, 63.99798883827455143 ) ) ;
#31831 = CARTESIAN_POINT ( 'NONE',  ( -18.16784385759799036, -9.357632978295827186, 49.97845033065683396 ) ) ;
#31832 = CARTESIAN_POINT ( 'NONE',  ( -17.01159385650551670, -6.922745924619793101, 51.69366785382590024 ) ) ;
#31833 = EDGE_CURVE ( 'NONE', #41418, #15882, #3599, .T. ) ;
#31834 = VECTOR ( 'NONE', #20580, 1000.000000000000000 ) ;
#31835 = ORIENTED_EDGE ( 'NONE', *, *, #30757, .T. ) ;
#31836 = CARTESIAN_POINT ( 'NONE',  ( -16.32575768948312600, -7.844986739114469643, 60.21500614002425777 ) ) ;
#31837 = CARTESIAN_POINT ( 'NONE',  ( -20.88147576600584543, -8.209942340109883219, 60.02620652709861560 ) ) ;
#31838 = ORIENTED_EDGE ( 'NONE', *, *, #14219, .T. ) ;
#31839 = DIRECTION ( 'NONE',  ( -1.616182858256118783E-16, -0.003028072113822189229, 0.9999954153791275058 ) ) ;
#31840 = CARTESIAN_POINT ( 'NONE',  ( -10.64211600630794585, -13.07553005057556739, 68.02366961159727055 ) ) ;
#31841 = CARTESIAN_POINT ( 'NONE',  ( -12.68656345882633296, -9.059469911947932275, 70.89279414395181789 ) ) ;
#31842 = CARTESIAN_POINT ( 'NONE',  ( -12.79725860806972904, -20.12850118792689358, 71.95653676770096752 ) ) ;
#31843 = CARTESIAN_POINT ( 'NONE',  ( -21.17518949801557682, -8.835587824813147861, 73.60128454375318086 ) ) ;
#31844 = ORIENTED_EDGE ( 'NONE', *, *, #31913, .T. ) ;
#31845 = CARTESIAN_POINT ( 'NONE',  ( -24.80874383141511430, -15.79476513899138368, 69.71024349780060447 ) ) ;
#31846 = CARTESIAN_POINT ( 'NONE',  ( -17.01436944207222624, -7.370403393205478437, 74.21664194825545735 ) ) ;
#31847 = EDGE_CURVE ( 'NONE', #20066, #43487, #885, .T. ) ;
#31848 = CARTESIAN_POINT ( 'NONE',  ( -23.69410989900737263, -17.92519740713284548, 59.19305441470095985 ) ) ;
#31849 = ORIENTED_EDGE ( 'NONE', *, *, #26187, .T. ) ;
#31850 = EDGE_CURVE ( 'NONE', #10797, #36678, #26717, .T. ) ;
#31851 = EDGE_CURVE ( 'NONE', #25517, #14949, #2119, .T. ) ;
#31852 = FACE_OUTER_BOUND ( 'NONE', #35240, .T. ) ;
#31853 = CARTESIAN_POINT ( 'NONE',  ( -24.56291696005103375, -12.67795903866814733, 69.91209651719337614 ) ) ;
#31854 = CARTESIAN_POINT ( 'NONE',  ( -16.42409385759798823, -9.359200813967568422, 50.49621490985803263 ) ) ;
#31855 = DIRECTION ( 'NONE',  ( 0.9687793358424817702, -0.2479245821708688791, 0.000000000000000000 ) ) ;
#31856 = VERTEX_POINT ( 'NONE', #8023 ) ;
#31857 = ORIENTED_EDGE ( 'NONE', *, *, #9886, .T. ) ;
#31858 = CARTESIAN_POINT ( 'NONE',  ( -17.18034385541304232, -9.360768649639302552, 51.01397948905922419 ) ) ;
#31859 = EDGE_CURVE ( 'NONE', #43190, #11955, #608, .T. ) ;
#31860 = CARTESIAN_POINT ( 'NONE',  ( -16.91478550490786859, -21.84108428878278119, 72.18015306840750611 ) ) ;
#31861 = CARTESIAN_POINT ( 'NONE',  ( -15.31091769494271837, -7.608297704863611344, 53.63095954094025331 ) ) ;
#31862 = CARTESIAN_POINT ( 'NONE',  ( -11.85162103594838001, -10.49015045520576983, 71.25420998615621215 ) ) ;
#31863 = AXIS2_PLACEMENT_3D ( 'NONE', #45616, #11868, #11371 ) ;
#31864 = LINE ( 'NONE', #13614, #16632 ) ;
#31865 = CARTESIAN_POINT ( 'NONE',  ( -14.25068793291388225, -8.513811817964199946, 71.02957628655769895 ) ) ;
#31866 = AXIS2_PLACEMENT_3D ( 'NONE', #9855, #32954, #17699 ) ;
#31867 = VERTEX_POINT ( 'NONE', #22527 ) ;
#31868 = FACE_OUTER_BOUND ( 'NONE', #21430, .T. ) ;
#31869 = CARTESIAN_POINT ( 'NONE',  ( -24.84449963183508459, -13.71944596863515464, 53.49999999999994316 ) ) ;
#31870 =( BOUNDED_SURFACE ( )  B_SPLINE_SURFACE ( 3, 1, ( 
 ( #28618, #5964 ),
 ( #43648, #36232 ),
 ( #24204, #46618 ),
 ( #10147, #42914 ),
 ( #28851, #35743 ),
 ( #2515, #17519 ),
 ( #12861, #25167 ) ),
 .UNSPECIFIED., .T., .F., .F. ) 
 B_SPLINE_SURFACE_WITH_KNOTS ( ( 4, 3, 4 ),
 ( 2, 2 ),
 ( 0.000000000000000000, 0.5000000000000000000, 1.000000000000000000 ),
 ( 0.000000000000000000, 1.000000000000000000 ),
 .UNSPECIFIED. ) 
 GEOMETRIC_REPRESENTATION_ITEM ( )  RATIONAL_B_SPLINE_SURFACE ( (
 ( 1.000000000000000000, 1.000000000000000000),
 ( 0.3333333333333335369, 0.3333333333333330373),
 ( 0.3333333333333335369, 0.3333333333333330373),
 ( 1.000000000000000000, 1.000000000000000000),
 ( 0.3333333333333333703, 0.3333333333333333703),
 ( 0.3333333333333333703, 0.3333333333333333703),
 ( 1.000000000000000000, 1.000000000000000000) ) ) 
 REPRESENTATION_ITEM ( '' )  SURFACE ( )  );
#31871 = ORIENTED_EDGE ( 'NONE', *, *, #18591, .F. ) ;
#31872 = CARTESIAN_POINT ( 'NONE',  ( -15.77409385541301035, -6.859212275519753099, 50.50378509014291240 ) ) ;
#31873 = DIRECTION ( 'NONE',  ( 0.000000000000000000, 1.000000000000000000, -0.000000000000000000 ) ) ;
#31874 = EDGE_LOOP ( 'NONE', ( #2894, #34434, #19082, #28154, #46728 ) ) ;
#31875 = CARTESIAN_POINT ( 'NONE',  ( -23.29918339618657086, -19.39037464299967439, 58.99915238703562181 ) ) ;
#31876 = FACE_OUTER_BOUND ( 'NONE', #47165, .T. ) ;
#31877 = ORIENTED_EDGE ( 'NONE', *, *, #4136, .T. ) ;
#31878 = CARTESIAN_POINT ( 'NONE',  ( -18.06139463723319949, -21.83834701327926808, 58.56120650458878174 ) ) ;
#31879 = FACE_OUTER_BOUND ( 'NONE', #44378, .T. ) ;
#31880 = EDGE_CURVE ( 'NONE', #4125, #11393, #18976, .T. ) ;
#31881 =( BOUNDED_CURVE ( )  B_SPLINE_CURVE ( 3, ( #47621, #47139, #10442, #13853 ),
 .UNSPECIFIED., .F., .F. ) 
 B_SPLINE_CURVE_WITH_KNOTS ( ( 4, 4 ),
 ( 0.5000000000000000000, 0.9074455897393649551 ),
 .UNSPECIFIED. ) 
 CURVE ( )  GEOMETRIC_REPRESENTATION_ITEM ( )  RATIONAL_B_SPLINE_CURVE ( ( 0.9999999999999747979, 0.4567392136813269166, 0.3561768502900459210, 0.6983129098261047218 ) ) 
 REPRESENTATION_ITEM ( '' )  );
#31882 = CARTESIAN_POINT ( 'NONE',  ( -12.82854046268865034, -13.89041861240101206, 49.52966884056655772 ) ) ;
#31883 = DIRECTION ( 'NONE',  ( 0.9477661110324760996, -0.3189661404888857188, 2.738326501554841424E-08 ) ) ;
#31884 = ORIENTED_EDGE ( 'NONE', *, *, #16620, .T. ) ;
#31885 = CARTESIAN_POINT ( 'NONE',  ( -10.66137368835686416, -12.80659570974005668, 60.68364890423993785 ) ) ;
#31886 = CARTESIAN_POINT ( 'NONE',  ( -17.79490377976783932, -14.65920654474411045, 52.21286476528345588 ) ) ;
#31887 =( BOUNDED_CURVE ( )  B_SPLINE_CURVE ( 3, ( #14946, #19153, #30255, #3397 ),
 .UNSPECIFIED., .F., .F. ) 
 B_SPLINE_CURVE_WITH_KNOTS ( ( 4, 4 ),
 ( 0.000000000000000000, 0.4074455897393697290 ),
 .UNSPECIFIED. ) 
 CURVE ( )  GEOMETRIC_REPRESENTATION_ITEM ( )  RATIONAL_B_SPLINE_CURVE ( ( 1.000000000000000000, 0.4567392136813214210, 0.3561768502900264366, 0.6983129098261150469 ) ) 
 REPRESENTATION_ITEM ( '' )  );
#31888 = CARTESIAN_POINT ( 'NONE',  ( -24.14679772577363437, -12.68507108172156883, 70.05770892828130059 ) ) ;
#31889 = CARTESIAN_POINT ( 'NONE',  ( -12.09300774956044755, -19.42703681131052562, 58.34171032836335513 ) ) ;
#31890 = B_SPLINE_CURVE_WITH_KNOTS ( 'NONE', 1,
 ( #24843, #43565 ),
 .UNSPECIFIED., .F., .F.,
 ( 2, 2 ),
 ( 0.000000000000000000, 1.000000000000000000 ),
 .UNSPECIFIED. ) ;
#31891 = CARTESIAN_POINT ( 'NONE',  ( -17.36015951656348832, -7.359395083792595216, 67.20534920880687935 ) ) ;
#31892 = CARTESIAN_POINT ( 'NONE',  ( -22.41759978862804914, -13.18828134753566417, 49.52966884056655772 ) ) ;
#31893 = ORIENTED_EDGE ( 'NONE', *, *, #18161, .F. ) ;
#31894 = DIRECTION ( 'NONE',  ( -0.2189141945955536961, 0.9757441136919967617, 0.000000000000000000 ) ) ;
#31895 = CARTESIAN_POINT ( 'NONE',  ( -11.14403518423954509, -11.71714199058991568, 67.72750603396154645 ) ) ;
#31896 = CARTESIAN_POINT ( 'NONE',  ( -24.09024125277505490, -17.10388469556238533, 72.88336035478459962 ) ) ;
#31897 = ORIENTED_EDGE ( 'NONE', *, *, #5113, .T. ) ;
#31898 = FACE_OUTER_BOUND ( 'NONE', #37941, .T. ) ;
#31899 =( BOUNDED_CURVE ( )  B_SPLINE_CURVE ( 3, ( #4553, #12426, #30916, #31139 ),
 .UNSPECIFIED., .F., .F. ) 
 B_SPLINE_CURVE_WITH_KNOTS ( ( 4, 4 ),
 ( 0.000000000000000000, 0.4074455897393652881 ),
 .UNSPECIFIED. ) 
 CURVE ( )  GEOMETRIC_REPRESENTATION_ITEM ( )  RATIONAL_B_SPLINE_CURVE ( ( 1.000000000000000000, 0.4567392136813347991, 0.3561768502900313216, 0.6983129098260896228 ) ) 
 REPRESENTATION_ITEM ( '' )  );
#31900 = CIRCLE ( 'NONE', #34234, 1.050000000000002265 ) ;
#31901 = VERTEX_POINT ( 'NONE', #45919 ) ;
#31902 = VERTEX_POINT ( 'NONE', #27197 ) ;
#31903 = ORIENTED_EDGE ( 'NONE', *, *, #30903, .F. ) ;
#31904 = EDGE_CURVE ( 'NONE', #30602, #37234, #9583, .T. ) ;
#31905 = CARTESIAN_POINT ( 'NONE',  ( -14.04312441377786946, -20.93869165529285681, 71.92607738043835752 ) ) ;
#31906 = EDGE_CURVE ( 'NONE', #47012, #39245, #7161, .T. ) ;
#31907 = CARTESIAN_POINT ( 'NONE',  ( -11.46028008028683942, -18.56947564720590194, 61.56238700194530367 ) ) ;
#31908 = CARTESIAN_POINT ( 'NONE',  ( -21.21137848157293249, -8.922231491198125752, 73.79231820712855949 ) ) ;
#31909 = CARTESIAN_POINT ( 'NONE',  ( -15.24284385759798965, -7.587656875400192291, 49.25157356644813689 ) ) ;
#31910 = CARTESIAN_POINT ( 'NONE',  ( -13.40403435948632094, -9.078590645922671953, 60.45452650781103898 ) ) ;
#31911 = ORIENTED_EDGE ( 'NONE', *, *, #11267, .F. ) ;
#31912 = EDGE_LOOP ( 'NONE', ( #18170, #40032, #31936 ) ) ;
#31913 = EDGE_CURVE ( 'NONE', #13312, #6974, #16991, .T. ) ;
#31914 = CARTESIAN_POINT ( 'NONE',  ( -10.74573065459234478, -12.54952415110468422, 60.81325645027152405 ) ) ;
#31915 = DIRECTION ( 'NONE',  ( -0.000000000000000000, 0.000000000000000000, 1.000000000000000000 ) ) ;
#31916 = CARTESIAN_POINT ( 'NONE',  ( -21.06494968540953749, -21.30903997076690359, 62.15825466738357363 ) ) ;
#31917 = CARTESIAN_POINT ( 'NONE',  ( -23.66220297886838964, -18.88224728823589160, 69.55017934013164904 ) ) ;
#31918 = EDGE_CURVE ( 'NONE', #13753, #14422, #41102, .T. ) ;
#31919 = CARTESIAN_POINT ( 'NONE',  ( -13.02466687598806239, -9.790356633151166221, 49.88233999786937289 ) ) ;
#31920 = ORIENTED_EDGE ( 'NONE', *, *, #26076, .T. ) ;
#31921 = CYLINDRICAL_SURFACE ( 'NONE', #47735, 0.1499999999999975242 ) ;
#31922 = CARTESIAN_POINT ( 'NONE',  ( -20.32907747881911575, -11.13165948213016776, 52.02966884056656482 ) ) ;
#31923 = CARTESIAN_POINT ( 'NONE',  ( -12.51438907681678536, -19.79882988928595822, 64.86674880260875398 ) ) ;
#31924 = ORIENTED_EDGE ( 'NONE', *, *, #25377, .F. ) ;
#31925 = DIRECTION ( 'NONE',  ( 1.011289380940303784E-05, -7.260693215641691253E-06, 0.9999999999225058778 ) ) ;
#31926 = AXIS2_PLACEMENT_3D ( 'NONE', #22977, #45374, #46341 ) ;
#31927 = CARTESIAN_POINT ( 'NONE',  ( -10.37394849890712401, -14.76283852923608464, 71.61310637325181006 ) ) ;
#31928 = CARTESIAN_POINT ( 'NONE',  ( -16.35517392334946152, -21.72711159609176690, 58.47688641158507039 ) ) ;
#31929 = CARTESIAN_POINT ( 'NONE',  ( -14.47284097950645432, -7.968636565268744754, 63.89704670002799247 ) ) ;
#31930 = ORIENTED_EDGE ( 'NONE', *, *, #43854, .T. ) ;
#31931 = FACE_OUTER_BOUND ( 'NONE', #39553, .T. ) ;
#31932 = EDGE_CURVE ( 'NONE', #31812, #30116, #40388, .T. ) ;
#31933 = B_SPLINE_CURVE_WITH_KNOTS ( 'NONE', 1,
 ( #4762, #12144 ),
 .UNSPECIFIED., .F., .F.,
 ( 2, 2 ),
 ( 0.000000000000000000, 1.000000000000000000 ),
 .UNSPECIFIED. ) ;
#31934 = CARTESIAN_POINT ( 'NONE',  ( -23.07906255732286738, -9.958937815627702861, 66.72677557046061736 ) ) ;
#31935 = CARTESIAN_POINT ( 'NONE',  ( -10.48067351556794158, -16.03044098841782628, 68.27767830705533925 ) ) ;
#31936 = ORIENTED_EDGE ( 'NONE', *, *, #10359, .T. ) ;
#31937 = CARTESIAN_POINT ( 'NONE',  ( -8.424093855413053333, -25.10920654474410441, 47.99999999999998579 ) ) ;
#31938 = ORIENTED_EDGE ( 'NONE', *, *, #698, .F. ) ;
#31939 = DIRECTION ( 'NONE',  ( -3.071710424422018668E-17, 6.404604876783312462E-16, 1.000000000000000000 ) ) ;
#31940 = CARTESIAN_POINT ( 'NONE',  ( -12.23849770038826534, -15.62901903366650380, 50.77966884056655772 ) ) ;
#31941 = VERTEX_POINT ( 'NONE', #39432 ) ;
#31942 = DIRECTION ( 'NONE',  ( 1.069446452691264255E-06, -1.103879811633194674E-06, 0.9999999999988189447 ) ) ;
#31943 = CARTESIAN_POINT ( 'NONE',  ( -21.80761170843182128, -20.26838994411330219, 58.99272793439983076 ) ) ;
#31944 = CARTESIAN_POINT ( 'NONE',  ( -24.07704370891653767, -17.14264987453632827, 72.89808101046212130 ) ) ;
#31945 = CARTESIAN_POINT ( 'NONE',  ( -22.09287085128708839, -15.21639644245407297, 49.52966884056655772 ) ) ;
#31946 = ORIENTED_EDGE ( 'NONE', *, *, #2736, .F. ) ;
#31947 = CARTESIAN_POINT ( 'NONE',  ( -17.42409385541300892, -14.80920654474439679, 56.49999999999994316 ) ) ;
#31948 = CYLINDRICAL_SURFACE ( 'NONE', #33693, 0.1500000000000015488 ) ;
#31949 = CARTESIAN_POINT ( 'NONE',  ( -46.46711114793018282, -12.76354662275040042, 70.87000000000000455 ) ) ;
#31950 = ORIENTED_EDGE ( 'NONE', *, *, #35320, .F. ) ;
#31951 = EDGE_CURVE ( 'NONE', #22984, #44794, #22257, .T. ) ;
#31952 = CARTESIAN_POINT ( 'NONE',  ( -17.39742543611924575, -7.759256981132187647, 67.32039592192056432 ) ) ;
#31953 = CARTESIAN_POINT ( 'NONE',  ( -24.43112999227502868, -15.58634490091467129, 73.00303748142292193 ) ) ;
#31954 = ORIENTED_EDGE ( 'NONE', *, *, #8265, .T. ) ;
#31955 = EDGE_LOOP ( 'NONE', ( #38742, #41609, #29729, #19133 ) ) ;
#31956 = CARTESIAN_POINT ( 'NONE',  ( -46.48223616206310993, -14.19714313411900619, 70.47802965039554124 ) ) ;
#31957 = CARTESIAN_POINT ( 'NONE',  ( -20.09559670342926552, -21.27944071986311414, 72.63152148437504252 ) ) ;
#31958 = EDGE_CURVE ( 'NONE', #24336, #15165, #10031, .T. ) ;
#31959 = CARTESIAN_POINT ( 'NONE',  ( -10.99655682251556144, -18.57624055219563175, 57.99209882808910521 ) ) ;
#31960 = CARTESIAN_POINT ( 'NONE',  ( -18.75534385650551528, -7.417179338643134834, 52.18511593390279302 ) ) ;
#31961 = CARTESIAN_POINT ( 'NONE',  ( -11.74997710522658600, -10.61883180769318535, 70.96892938659537720 ) ) ;
#31962 = CARTESIAN_POINT ( 'NONE',  ( -24.72409385541305582, -14.90920654474410512, 57.89999999999999147 ) ) ;
#31963 = CARTESIAN_POINT ( 'NONE',  ( -12.25434508901797770, -20.17367074759813406, 65.05170324716399932 ) ) ;
#31964 = CARTESIAN_POINT ( 'NONE',  ( -18.94863228570505598, -7.922318267881538922, 70.46248317377518333 ) ) ;
#31965 = VECTOR ( 'NONE', #4150, 1000.000000000000000 ) ;
#31966 = ORIENTED_EDGE ( 'NONE', *, *, #26807, .F. ) ;
#31967 = ORIENTED_EDGE ( 'NONE', *, *, #47856, .T. ) ;
#31968 = EDGE_CURVE ( 'NONE', #42734, #43742, #25235, .T. ) ;
#31969 = CARTESIAN_POINT ( 'NONE',  ( -13.52486571068042487, -17.40907233461224735, 49.52966884056655772 ) ) ;
#31970 = DIRECTION ( 'NONE',  ( 1.000000000000000000, 0.000000000000000000, 0.000000000000000000 ) ) ;
#31971 = MANIFOLD_SOLID_BREP ( 'Stock-MAS-175-1', #36174 ) ;
#31972 = CARTESIAN_POINT ( 'NONE',  ( -23.67460871249246068, -11.65500680865467054, 66.65044377215316729 ) ) ;
#31973 = CARTESIAN_POINT ( 'NONE',  ( -14.78750812280958726, -21.29541618567930072, 61.74673429867123531 ) ) ;
#31974 = CARTESIAN_POINT ( 'NONE',  ( -24.54031182138101741, -12.60405816868659912, 69.87904686005836652 ) ) ;
#31975 =( BOUNDED_CURVE ( )  B_SPLINE_CURVE ( 3, ( #12394, #27415, #34066, #42450 ),
 .UNSPECIFIED., .F., .F. ) 
 B_SPLINE_CURVE_WITH_KNOTS ( ( 4, 4 ),
 ( 0.4074455897393611248, 0.5000000000000000000 ),
 .UNSPECIFIED. ) 
 CURVE ( )  GEOMETRIC_REPRESENTATION_ITEM ( )  RATIONAL_B_SPLINE_CURVE ( ( 0.6983129098260971723, 0.7760317562606624531, 0.8765941196519518863, 0.9999999999999374944 ) ) 
 REPRESENTATION_ITEM ( '' )  );
#31976 = EDGE_CURVE ( 'NONE', #40331, #23337, #33967, .T. ) ;
#31977 = DIRECTION ( 'NONE',  ( -2.231660450020913765E-16, -0.9999954153791275058, -0.003028072113822189229 ) ) ;
#31978 = B_SPLINE_CURVE_WITH_KNOTS ( 'NONE', 3,
 ( #9043, #31435, #39310, #16881, #1387, #27740, #24551, #16402, #43260, #12477 ),
 .UNSPECIFIED., .F., .F.,
 ( 4, 2, 2, 2, 4 ),
 ( 0.1272669073658265759, 0.2522669073439348653, 0.3772669073220431546, 0.5022669073001514439, 0.6272669072782597333 ),
 .UNSPECIFIED. ) ;
#31979 = ORIENTED_EDGE ( 'NONE', *, *, #31984, .T. ) ;
#31980 = DIRECTION ( 'NONE',  ( -1.000000000000000000, 0.000000000000000000, 0.000000000000000000 ) ) ;
#31981 =( NAMED_UNIT ( * ) SI_UNIT ( $, .STERADIAN. ) SOLID_ANGLE_UNIT ( ) );
#31982 = CARTESIAN_POINT ( 'NONE',  ( -11.77169895589660698, -10.59578386207264700, 74.43885051664024388 ) ) ;
#31983 = CARTESIAN_POINT ( 'NONE',  ( -24.11881394502254849, -17.01995806294775448, 73.16863963025599560 ) ) ;
#31984 = EDGE_CURVE ( 'NONE', #17425, #17144, #28593, .T. ) ;
#31985 = VERTEX_POINT ( 'NONE', #30304 ) ;
#31986 = EDGE_CURVE ( 'NONE', #42245, #44810, #15238, .T. ) ;
#31987 = CARTESIAN_POINT ( 'NONE',  ( -21.34511485531846020, -8.950139844736156647, 73.90128722075769474 ) ) ;
#31988 = EDGE_CURVE ( 'NONE', #38501, #40815, #43385, .T. ) ;
#31989 = CARTESIAN_POINT ( 'NONE',  ( -10.58203424369019174, -16.28808381980452324, 71.73284965287206205 ) ) ;
#31990 = ADVANCED_FACE ( 'NONE', ( #10597 ), #22173, .T. ) ;
#31991 = FACE_OUTER_BOUND ( 'NONE', #36037, .T. ) ;
#31992 = CARTESIAN_POINT ( 'NONE',  ( -18.67229701437506506, -7.919758800372044050, 74.02991576449618094 ) ) ;
#31993 = CARTESIAN_POINT ( 'NONE',  ( -15.53265176333180619, -21.60105060138385014, 72.33103357390284316 ) ) ;
#31994 = CARTESIAN_POINT ( 'NONE',  ( -23.51785719624223958, -11.36449344406884343, 70.19210750610864125 ) ) ;
#31995 = ORIENTED_EDGE ( 'NONE', *, *, #31414, .T. ) ;
#31996 = CARTESIAN_POINT ( 'NONE',  ( -10.37599212182869124, -14.63324797960940593, 71.34254748307667171 ) ) ;
#31997 = AXIS2_PLACEMENT_3D ( 'NONE', #27299, #42326, #46512 ) ;
#31998 = CIRCLE ( 'NONE', #32798, 3.982850737850970990 ) ;
#31999 = ORIENTED_EDGE ( 'NONE', *, *, #26397, .F. ) ;
#32000 = PLANE ( 'NONE',  #39025 ) ;
#32001 = EDGE_LOOP ( 'NONE', ( #1335, #35156, #17426, #20005, #26774 ) ) ;
#32002 = CARTESIAN_POINT ( 'NONE',  ( -18.32857756213031664, -22.20418371868804996, 68.93019407337365578 ) ) ;
#32003 = CARTESIAN_POINT ( 'NONE',  ( -15.35534385650552203, -7.417179338643134834, 52.18511593390279302 ) ) ;
#32004 = EDGE_LOOP ( 'NONE', ( #44449, #37044, #4599, #46595, #46508 ) ) ;
#32005 = CARTESIAN_POINT ( 'NONE',  ( -14.11063322135152909, -21.03236308526469855, 72.21135587486895702 ) ) ;
#32006 = VECTOR ( 'NONE', #9806, 1000.000000000000000 ) ;
#32007 = CARTESIAN_POINT ( 'NONE',  ( -10.64864687305616009, -11.71119991730035181, 74.73652894950812708 ) ) ;
#32008 = CARTESIAN_POINT ( 'NONE',  ( -10.88209242003807908, -17.29963164818252608, 64.62739380462950578 ) ) ;
#32009 = ORIENTED_EDGE ( 'NONE', *, *, #36866, .F. ) ;
#32010 = CARTESIAN_POINT ( 'NONE',  ( -16.12274100365893048, -7.931235850141636234, 60.30914399322803376 ) ) ;
#32011 = DIRECTION ( 'NONE',  ( 0.3964226963016397320, 0.9180681052388968144, 0.000000000000000000 ) ) ;
#32012 = CARTESIAN_POINT ( 'NONE',  ( -24.60327268654570432, -12.81871823346896022, 66.40223105660061265 ) ) ;
#32013 = B_SPLINE_CURVE_WITH_KNOTS ( 'NONE', 1,
 ( #42714, #30666 ),
 .UNSPECIFIED., .F., .F.,
 ( 2, 2 ),
 ( 0.000000000000000000, 1.000000000000000000 ),
 .UNSPECIFIED. ) ;
#32014 = DIRECTION ( 'NONE',  ( -0.1240347345892083841, 0.000000000000000000, -0.9922778767136676281 ) ) ;
#32015 = ORIENTED_EDGE ( 'NONE', *, *, #47009, .F. ) ;
#32016 = ORIENTED_EDGE ( 'NONE', *, *, #32517, .T. ) ;
#32017 = CARTESIAN_POINT ( 'NONE',  ( -23.80579133695118443, -18.65331559044849641, 72.87029906539265767 ) ) ;
#32018 = CARTESIAN_POINT ( 'NONE',  ( -24.86242983737997747, -14.39095285025967286, 66.36788159907001727 ) ) ;
#32019 = EDGE_LOOP ( 'NONE', ( #15196, #40845 ) ) ;
#32020 = CARTESIAN_POINT ( 'NONE',  ( -11.46043843694620357, -11.04924462883820802, 57.50903212149482613 ) ) ;
#32021 = DIRECTION ( 'NONE',  ( -3.071710424422018668E-17, 6.404604876783312462E-16, 1.000000000000000000 ) ) ;
#32022 = CARTESIAN_POINT ( 'NONE',  ( -17.43659385759799108, -8.995762431863214559, 51.38120296130585274 ) ) ;
#32023 = DIRECTION ( 'NONE',  ( -0.000000000000000000, -1.000000000000000000, 0.000000000000000000 ) ) ;
#32024 =( BOUNDED_CURVE ( )  B_SPLINE_CURVE ( 3, ( #39829, #5383, #35638, #6095 ),
 .UNSPECIFIED., .F., .F. ) 
 B_SPLINE_CURVE_WITH_KNOTS ( ( 4, 4 ),
 ( 0.000000000000000000, 0.4074455897393618464 ),
 .UNSPECIFIED. ) 
 CURVE ( )  GEOMETRIC_REPRESENTATION_ITEM ( )  RATIONAL_B_SPLINE_CURVE ( ( 1.000000000000000000, 0.4567392136813371861, 0.3561768502900322653, 0.6983129098260852929 ) ) 
 REPRESENTATION_ITEM ( '' )  );
#32025 = CARTESIAN_POINT ( 'NONE',  ( -24.59706333651279664, -12.79617740830267891, 66.48742133194130588 ) ) ;
#32026 = CARTESIAN_POINT ( 'NONE',  ( -15.69736699998981422, -8.025519224215527103, 70.60989840319118116 ) ) ;
#32027 = VERTEX_POINT ( 'NONE', #33216 ) ;
#32028 = ADVANCED_FACE ( 'NONE', ( #4195 ), #45317, .T. ) ;
#32029 = CARTESIAN_POINT ( 'NONE',  ( -20.77150381139373536, -8.660956599501332676, 60.12508712995069260 ) ) ;
#32030 = CARTESIAN_POINT ( 'NONE',  ( -22.85367851456767596, -9.707840327915473466, 73.65973829363548475 ) ) ;
#32031 = CARTESIAN_POINT ( 'NONE',  ( -10.78921115435649369, -11.42050183187454770, 67.75718084852192646 ) ) ;
#32032 =( BOUNDED_CURVE ( )  B_SPLINE_CURVE ( 3, ( #20013, #35976, #17266, #9177 ),
 .UNSPECIFIED., .F., .F. ) 
 B_SPLINE_CURVE_WITH_KNOTS ( ( 4, 4 ),
 ( 0.000000000000000000, 0.4074455897393650106 ),
 .UNSPECIFIED. ) 
 CURVE ( )  GEOMETRIC_REPRESENTATION_ITEM ( )  RATIONAL_B_SPLINE_CURVE ( ( 1.000000000000000000, 0.4567392136813301362, 0.3561768502900296562, 0.6983129098260983936 ) ) 
 REPRESENTATION_ITEM ( '' )  );
#32033 = EDGE_LOOP ( 'NONE', ( #32949, #47176, #32230, #16214 ) ) ;
#32034 = CIRCLE ( 'NONE', #24942, 1.250000000000001110 ) ;
#32035 = ORIENTED_EDGE ( 'NONE', *, *, #48520, .T. ) ;
#32036 = VECTOR ( 'NONE', #46484, 1000.000000000000000 ) ;
#32037 = ORIENTED_EDGE ( 'NONE', *, *, #32122, .T. ) ;
#32038 = B_SPLINE_CURVE_WITH_KNOTS ( 'NONE', 1,
 ( #4422, #45568 ),
 .UNSPECIFIED., .F., .F.,
 ( 2, 2 ),
 ( 0.000000000000000000, 1.000000000000000000 ),
 .UNSPECIFIED. ) ;
#32039 = DIRECTION ( 'NONE',  ( -1.000000000000000000, 0.000000000000000000, 0.000000000000000000 ) ) ;
#32040 = CARTESIAN_POINT ( 'NONE',  ( -22.57823294519915436, -10.07257407465379551, 70.02680971841948576 ) ) ;
#32041 = DIRECTION ( 'NONE',  ( -2.866981220435666553E-17, 1.000000000000000000, 1.190614954331866791E-16 ) ) ;
#32042 = EDGE_LOOP ( 'NONE', ( #11334, #26497, #28740, #41875, #7331 ) ) ;
#32043 = EDGE_CURVE ( 'NONE', #26823, #17855, #22657, .T. ) ;
#32044 = CYLINDRICAL_SURFACE ( 'NONE', #687, 1.999999999999999556 ) ;
#32045 = CARTESIAN_POINT ( 'NONE',  ( -24.72409385541305582, -15.80920654474410725, 65.99999999999998579 ) ) ;
#32046 = EDGE_CURVE ( 'NONE', #40523, #14963, #11085, .T. ) ;
#32047 = EDGE_CURVE ( 'NONE', #16726, #21204, #1152, .T. ) ;
#32049 = ORIENTED_EDGE ( 'NONE', *, *, #9628, .T. ) ;
#32048 = BREP_WITH_VOIDS ( 'NONE', #40135, ( #3125 ) );
#32050 = DIRECTION ( 'NONE',  ( -0.06306825763707681054, 0.9980092158285026605, 2.415158932891090200E-08 ) ) ;
#32051 = CARTESIAN_POINT ( 'NONE',  ( -19.37462041217285957, -21.99941596162432589, 58.56861435762115775 ) ) ;
#32052 = ORIENTED_EDGE ( 'NONE', *, *, #12934, .F. ) ;
#32053 = CARTESIAN_POINT ( 'NONE',  ( -15.74091245749827195, -8.014583633770426374, 67.24893180729357312 ) ) ;
#32054 = ORIENTED_EDGE ( 'NONE', *, *, #27753, .T. ) ;
#32055 = DIRECTION ( 'NONE',  ( -0.7670373483544790094, -0.6416024518573233415, 2.496223344567222537E-08 ) ) ;
#32056 = ORIENTED_EDGE ( 'NONE', *, *, #43115, .T. ) ;
#32057 = CARTESIAN_POINT ( 'NONE',  ( -16.27095827323975996, -7.851109476482911909, 64.08499918177189159 ) ) ;
#32058 = LINE ( 'NONE', #24442, #25982 ) ;
#32059 = FACE_OUTER_BOUND ( 'NONE', #46686, .T. ) ;
#32060 = ORIENTED_EDGE ( 'NONE', *, *, #35644, .F. ) ;
#32061 = CARTESIAN_POINT ( 'NONE',  ( -24.26499789074519597, -17.75976756996305639, 62.65856417960095825 ) ) ;
#32062 = CARTESIAN_POINT ( 'NONE',  ( -45.92409385541306932, -16.70920654474410938, 70.50000000000000000 ) ) ;
#32063 = CARTESIAN_POINT ( 'NONE',  ( -23.65624089557865872, -11.51332380282628343, 66.57214514605458078 ) ) ;
#32064 = VECTOR ( 'NONE', #43751, 1000.000000000000000 ) ;
#32065 = DIRECTION ( 'NONE',  ( -3.071710424422018668E-17, 6.404604876783312462E-16, 1.000000000000000000 ) ) ;
#32066 = CARTESIAN_POINT ( 'NONE',  ( -13.02884944951828494, -13.18282747993466941, 49.52966884056655772 ) ) ;
#32067 = LINE ( 'NONE', #13089, #25073 ) ;
#32068 = ORIENTED_EDGE ( 'NONE', *, *, #47741, .T. ) ;
#32069 = DIRECTION ( 'NONE',  ( 3.071710424422018668E-17, -6.404604876783312462E-16, -1.000000000000000000 ) ) ;
#32070 = AXIS2_PLACEMENT_3D ( 'NONE', #25316, #48194, #10051 ) ;
#32071 = CIRCLE ( 'NONE', #39166, 2.000000000000000000 ) ;
#32072 = LINE ( 'NONE', #31589, #15557 ) ;
#32073 = CARTESIAN_POINT ( 'NONE',  ( -12.07950851572364748, -19.41234162675539920, 58.01862405632531505 ) ) ;
#32074 = CARTESIAN_POINT ( 'NONE',  ( -19.98515930221110892, -21.80534510432024575, 69.09515851530258601 ) ) ;
#32075 = CARTESIAN_POINT ( 'NONE',  ( -12.40380818233537141, -19.68739593843253033, 61.69678633575567517 ) ) ;
#32076 = ADVANCED_FACE ( 'NONE', ( #19197 ), #15043, .T. ) ;
#32077 = ORIENTED_EDGE ( 'NONE', *, *, #41059, .T. ) ;
#32078 = FACE_OUTER_BOUND ( 'NONE', #31779, .T. ) ;
#32079 = CARTESIAN_POINT ( 'NONE',  ( -24.31482301288783532, -13.31912224170856618, 59.66267924674055934 ) ) ;
#32080 = ORIENTED_EDGE ( 'NONE', *, *, #27664, .T. ) ;
#32081 = CARTESIAN_POINT ( 'NONE',  ( -11.25385002771267473, -18.98553936430136702, 68.40345028533118921 ) ) ;
#32082 = CARTESIAN_POINT ( 'NONE',  ( -20.98629261354270170, -17.87291272402722697, 49.52966884056655772 ) ) ;
#32083 = CARTESIAN_POINT ( 'NONE',  ( -23.07906255732286738, -9.958937815627702861, 66.72677557046061736 ) ) ;
#32084 = AXIS2_PLACEMENT_3D ( 'NONE', #29332, #17270, #2734 ) ;
#32085 = CARTESIAN_POINT ( 'NONE',  ( -22.34470984022960138, -19.78791505225649416, 69.17417989488706098 ) ) ;
#32086 = CARTESIAN_POINT ( 'NONE',  ( -16.92616160843403961, -22.24260109534890262, 72.27269065110013457 ) ) ;
#32087 = VERTEX_POINT ( 'NONE', #8365 ) ;
#32088 = VECTOR ( 'NONE', #36178, 1000.000000000000000 ) ;
#32089 = DIRECTION ( 'NONE',  ( -0.000000000000000000, -1.000000000000000000, -0.000000000000000000 ) ) ;
#32090 = CARTESIAN_POINT ( 'NONE',  ( -20.89788161767221197, -20.94431024770144489, 62.39999296070408974 ) ) ;
#32091 = CARTESIAN_POINT ( 'NONE',  ( -23.72463725732412954, -17.86031838844568043, 59.28761838504880899 ) ) ;
#32092 = ORIENTED_EDGE ( 'NONE', *, *, #40165, .F. ) ;
#32093 = DIRECTION ( 'NONE',  ( -9.009793368474262471E-08, 1.813722298394044057E-06, -0.9999999999983512078 ) ) ;
#32094 = CARTESIAN_POINT ( 'NONE',  ( -9.979603215878100286, -14.52052451035377345, 68.04295550616701860 ) ) ;
#32095 = EDGE_CURVE ( 'NONE', #18357, #40783, #23383, .T. ) ;
#32096 = CARTESIAN_POINT ( 'NONE',  ( -13.42842738616806209, -9.059671689720946830, 64.02019725504824521 ) ) ;
#32097 = CARTESIAN_POINT ( 'NONE',  ( -50.42609385541305755, -14.80920654474420139, 66.95294117647057419 ) ) ;
#32098 = CARTESIAN_POINT ( 'NONE',  ( -24.03287018854308954, -12.34366040360348471, 73.24225467054047556 ) ) ;
#32099 = FACE_OUTER_BOUND ( 'NONE', #47268, .T. ) ;
#32100 = VERTEX_POINT ( 'NONE', #8862 ) ;
#32101 = VERTEX_POINT ( 'NONE', #30790 ) ;
#32102 = CARTESIAN_POINT ( 'NONE',  ( -16.50534385541304161, -7.595227055684746986, 51.75156210489594599 ) ) ;
#32103 = CARTESIAN_POINT ( 'NONE',  ( -11.49688049385020960, -18.62690763749001732, 64.76179218520603342 ) ) ;
#32104 = AXIS2_PLACEMENT_3D ( 'NONE', #11467, #33359, #22309 ) ;
#32105 = CARTESIAN_POINT ( 'NONE',  ( -17.74514309872235884, -7.766371812394021745, 60.37500991003656736 ) ) ;
#32106 = AXIS2_PLACEMENT_3D ( 'NONE', #10817, #37141, #3428 ) ;
#32107 = VECTOR ( 'NONE', #9431, 1000.000000000000000 ) ;
#32108 = AXIS2_PLACEMENT_3D ( 'NONE', #5070, #46184, #35335 ) ;
#32109 = DIRECTION ( 'NONE',  ( -0.2196488028684550620, -0.9755790093059855117, 7.835600157697873389E-08 ) ) ;
#32110 = EDGE_CURVE ( 'NONE', #32931, #784, #44095, .T. ) ;
#32111 = CARTESIAN_POINT ( 'NONE',  ( -17.42409385541299471, -14.80920654474435771, 49.52966884056655772 ) ) ;
#32112 = ORIENTED_EDGE ( 'NONE', *, *, #8949, .F. ) ;
#32113 = CARTESIAN_POINT ( 'NONE',  ( -11.33492925930432804, -11.25580429380516456, 60.97325962342065253 ) ) ;
#32114 = CIRCLE ( 'NONE', #21078, 0.2499999999999976408 ) ;
#32115 = CARTESIAN_POINT ( 'NONE',  ( -18.90996479553717791, -7.968725069611966916, 66.90071784165556323 ) ) ;
#32116 = B_SPLINE_CURVE_WITH_KNOTS ( 'NONE', 1,
 ( #30236, #42032 ),
 .UNSPECIFIED., .F., .F.,
 ( 2, 2 ),
 ( 0.000000000000000000, 1.000000000000000000 ),
 .UNSPECIFIED. ) ;
#32117 = ORIENTED_EDGE ( 'NONE', *, *, #45166, .F. ) ;
#32118 = CARTESIAN_POINT ( 'NONE',  ( -16.78411497196904278, -21.83009869597353259, 68.69560651670111895 ) ) ;
#32119 = CARTESIAN_POINT ( 'NONE',  ( -20.86860741727135959, -11.63137574808859753, 52.02966884056656482 ) ) ;
#32120 = ORIENTED_EDGE ( 'NONE', *, *, #27405, .T. ) ;
#32121 = EDGE_CURVE ( 'NONE', #978, #4347, #38883, .T. ) ;
#32122 = EDGE_CURVE ( 'NONE', #33156, #44748, #13738, .T. ) ;
#32123 = CARTESIAN_POINT ( 'NONE',  ( -10.31413044408767554, -17.03453498993188475, 57.94406477676061229 ) ) ;
#32124 = ORIENTED_EDGE ( 'NONE', *, *, #7641, .F. ) ;
#32125 = DIRECTION ( 'NONE',  ( 0.000000000000000000, 1.000000000000000000, 0.000000000000000000 ) ) ;
#32126 = ADVANCED_FACE ( 'NONE', ( #45566 ), #32340, .T. ) ;
#32127 = DIRECTION ( 'NONE',  ( -0.000000000000000000, -1.000000000000000000, -0.000000000000000000 ) ) ;
#32128 = EDGE_CURVE ( 'NONE', #13240, #32374, #33903, .T. ) ;
#32129 = FACE_OUTER_BOUND ( 'NONE', #41620, .T. ) ;
#32130 = LINE ( 'NONE', #43955, #19759 ) ;
#32131 = VERTEX_POINT ( 'NONE', #24113 ) ;
#32132 = CARTESIAN_POINT ( 'NONE',  ( -22.10219206297270489, -9.524287713326932803, 63.33586711951718229 ) ) ;
#32133 = CARTESIAN_POINT ( 'NONE',  ( 18.54465614458695200, 0.6407533398237036382, 50.52649563099625851 ) ) ;
#32134 = LINE ( 'NONE', #27942, #16034 ) ;
#32135 = FACE_OUTER_BOUND ( 'NONE', #16769, .T. ) ;
#32136 = CONTEXT_DEPENDENT_SHAPE_REPRESENTATION ( #25599, #11048 ) ;
#32137 = CARTESIAN_POINT ( 'NONE',  ( -20.05785487306503256, -7.839488668639425839, 73.83441365354759967 ) ) ;
#32138 = CARTESIAN_POINT ( 'NONE',  ( -17.36175868705992897, -7.359389033274929659, 67.06393689457253515 ) ) ;
#32139 = ADVANCED_FACE ( 'NONE', ( #38384 ), #34447, .F. ) ;
#32140 = CARTESIAN_POINT ( 'NONE',  ( -26.92409385541305511, -6.359206544744109735, 63.99999999999998579 ) ) ;
#32141 = FACE_OUTER_BOUND ( 'NONE', #33213, .T. ) ;
#32142 = ORIENTED_EDGE ( 'NONE', *, *, #22371, .T. ) ;
#32143 = DIRECTION ( 'NONE',  ( -4.615129100576721730E-07, 1.699487034244351503E-08, -0.9999999999998933076 ) ) ;
#32144 = VECTOR ( 'NONE', #31303, 1000.000000000000000 ) ;
#32145 = CARTESIAN_POINT ( 'NONE',  ( -14.26613035333006785, -8.061623769020160424, 67.45986280861907858 ) ) ;
#32146 = CARTESIAN_POINT ( 'NONE',  ( -24.29719970949782137, -16.39516428949632854, 62.89328972680635843 ) ) ;
#32147 = ORIENTED_EDGE ( 'NONE', *, *, #14060, .F. ) ;
#32148 = CARTESIAN_POINT ( 'NONE',  ( -23.88415222675040539, -17.63235122089636775, 62.47360984996718969 ) ) ;
#32149 = AXIS2_PLACEMENT_3D ( 'NONE', #29411, #40727, #29907 ) ;
#32150 = AXIS2_PLACEMENT_3D ( 'NONE', #22413, #37404, #3700 ) ;
#32151 = EDGE_LOOP ( 'NONE', ( #18359, #6234 ) ) ;
#32152 = ORIENTED_EDGE ( 'NONE', *, *, #16204, .T. ) ;
#32153 = ORIENTED_EDGE ( 'NONE', *, *, #13355, .T. ) ;
#32154 = CARTESIAN_POINT ( 'NONE',  ( -14.00884526327672397, -20.92003366206770210, 71.94224368477696885 ) ) ;
#32155 = AXIS2_PLACEMENT_3D ( 'NONE', #16842, #17332, #20801 ) ;
#32156 = CARTESIAN_POINT ( 'NONE',  ( -23.72751372599721620, -11.76491108559917720, 59.55523859581371937 ) ) ;
#32157 = DIRECTION ( 'NONE',  ( -0.9118114225829224706, -0.4106092176842892627, -5.589476761700638069E-08 ) ) ;
#32158 = CARTESIAN_POINT ( 'NONE',  ( -12.05483347687720475, -10.31798811457585963, 67.79896870046731294 ) ) ;
#32159 = CARTESIAN_POINT ( 'NONE',  ( -10.72958667791015763, -16.85608332250551200, 57.70377195876292120 ) ) ;
#32160 = ORIENTED_EDGE ( 'NONE', *, *, #33, .F. ) ;
#32161 = VERTEX_POINT ( 'NONE', #15480 ) ;
#32162 = CARTESIAN_POINT ( 'NONE',  ( -18.22409385650551528, -6.426201560718813433, 50.50509628382439331 ) ) ;
#32163 = CARTESIAN_POINT ( 'NONE',  ( -21.02116742812006223, -20.87599269455877860, 61.99982634431184181 ) ) ;
#32164 = CARTESIAN_POINT ( 'NONE',  ( -24.72409385541305582, -14.90920654474415663, 62.02941176470587692 ) ) ;
#32165 =( BOUNDED_SURFACE ( )  B_SPLINE_SURFACE ( 3, 1, ( 
 ( #26990, #46441 ),
 ( #45951, #42258 ),
 ( #38292, #1611 ),
 ( #9015, #16622 ),
 ( #31659, #16376 ),
 ( #27714, #27473 ),
 ( #24036, #42015 ) ),
 .UNSPECIFIED., .T., .F., .F. ) 
 B_SPLINE_SURFACE_WITH_KNOTS ( ( 4, 3, 4 ),
 ( 2, 2 ),
 ( 0.000000000000000000, 0.5000000000000000000, 1.000000000000000000 ),
 ( 0.000000000000000000, 1.000000000000000000 ),
 .UNSPECIFIED. ) 
 GEOMETRIC_REPRESENTATION_ITEM ( )  RATIONAL_B_SPLINE_SURFACE ( (
 ( 1.000000000000000000, 1.000000000000000000),
 ( 0.3333333333333335369, 0.3333333333333330373),
 ( 0.3333333333333335369, 0.3333333333333330373),
 ( 1.000000000000000000, 1.000000000000000000),
 ( 0.3333333333333333703, 0.3333333333333333703),
 ( 0.3333333333333333703, 0.3333333333333333703),
 ( 1.000000000000000000, 1.000000000000000000) ) ) 
 REPRESENTATION_ITEM ( '' )  SURFACE ( )  );
#32166 = EDGE_CURVE ( 'NONE', #3873, #8865, #4672, .T. ) ;
#32167 = CARTESIAN_POINT ( 'NONE',  ( -18.89909385650551599, -8.114302828567740988, 52.18300498402516041 ) ) ;
#32168 = ORIENTED_EDGE ( 'NONE', *, *, #28098, .T. ) ;
#32169 = ADVANCED_FACE ( 'NONE', ( #980 ), #11821, .T. ) ;
#32170 = DIRECTION ( 'NONE',  ( 0.8603395911234834603, 0.5097212845717522534, 0.000000000000000000 ) ) ;
#32171 = AXIS2_PLACEMENT_3D ( 'NONE', #1946, #16945, #43569 ) ;
#32172 = CARTESIAN_POINT ( 'NONE',  ( -24.80746943141735983, -15.80390768895026987, 69.57661537956182940 ) ) ;
#32173 = ORIENTED_EDGE ( 'NONE', *, *, #11450, .F. ) ;
#32174 =( BOUNDED_SURFACE ( )  B_SPLINE_SURFACE ( 3, 1, ( 
 ( #34289, #42185 ),
 ( #8445, #4759 ),
 ( #23479, #16056 ),
 ( #31097, #46119 ),
 ( #5007, #16296 ),
 ( #5240, #24451 ),
 ( #5962, #1536 ) ),
 .UNSPECIFIED., .T., .F., .F. ) 
 B_SPLINE_SURFACE_WITH_KNOTS ( ( 4, 3, 4 ),
 ( 2, 2 ),
 ( 0.000000000000000000, 0.5000000000000000000, 1.000000000000000000 ),
 ( 0.000000000000000000, 1.000000000000000000 ),
 .UNSPECIFIED. ) 
 GEOMETRIC_REPRESENTATION_ITEM ( )  RATIONAL_B_SPLINE_SURFACE ( (
 ( 1.000000000000000000, 1.000000000000000000),
 ( 0.3333333333333335369, 0.3333333333333330373),
 ( 0.3333333333333335369, 0.3333333333333330373),
 ( 1.000000000000000000, 1.000000000000000000),
 ( 0.3333333333333333703, 0.3333333333333333703),
 ( 0.3333333333333333703, 0.3333333333333333703),
 ( 1.000000000000000000, 1.000000000000000000) ) ) 
 REPRESENTATION_ITEM ( '' )  SURFACE ( )  );
#32175 = CARTESIAN_POINT ( 'NONE',  ( -50.42609385541305755, -14.80920654474423159, 69.97058823529410176 ) ) ;
#32176 =( BOUNDED_SURFACE ( )  B_SPLINE_SURFACE ( 3, 1, ( 
 ( #35591, #24541 ),
 ( #37211, #39537 ),
 ( #2350, #5817 ),
 ( #47173, #18014 ),
 ( #48077, #21975 ),
 ( #3259, #14313 ),
 ( #18263, #29364 ) ),
 .UNSPECIFIED., .T., .F., .F. ) 
 B_SPLINE_SURFACE_WITH_KNOTS ( ( 4, 3, 4 ),
 ( 2, 2 ),
 ( 0.000000000000000000, 0.5000000000000000000, 1.000000000000000000 ),
 ( 0.000000000000000000, 1.000000000000000000 ),
 .UNSPECIFIED. ) 
 GEOMETRIC_REPRESENTATION_ITEM ( )  RATIONAL_B_SPLINE_SURFACE ( (
 ( 1.000000000000000000, 1.000000000000000000),
 ( 0.3333333333333335369, 0.3333333333333330373),
 ( 0.3333333333333335369, 0.3333333333333330373),
 ( 1.000000000000000000, 1.000000000000000000),
 ( 0.3333333333333333703, 0.3333333333333333703),
 ( 0.3333333333333333703, 0.3333333333333333703),
 ( 1.000000000000000000, 1.000000000000000000) ) ) 
 REPRESENTATION_ITEM ( '' )  SURFACE ( )  );
#32177 = AXIS2_PLACEMENT_3D ( 'NONE', #24947, #47601, #13833 ) ;
#32178 = VECTOR ( 'NONE', #5315, 1000.000000000000000 ) ;
#32179 = CARTESIAN_POINT ( 'NONE',  ( -11.67943375510494697, -18.89645239624664441, 68.50217487844219022 ) ) ;
#32180 = CARTESIAN_POINT ( 'NONE',  ( -22.53538519471304369, -20.22938801946909138, 65.74775819791243237 ) ) ;
#32181 = ADVANCED_FACE ( 'NONE', ( #12536 ), #27561, .T. ) ;
#32182 = ORIENTED_EDGE ( 'NONE', *, *, #13355, .F. ) ;
#32183 = VECTOR ( 'NONE', #8774, 1000.000000000000114 ) ;
#32184 = ADVANCED_FACE ( 'NONE', ( #28539 ), #5885, .T. ) ;
#32185 = CARTESIAN_POINT ( 'NONE',  ( -22.58023486647882550, -9.989541079992143580, 66.69749311060769514 ) ) ;
#32186 = CARTESIAN_POINT ( 'NONE',  ( -21.01124108229941001, -20.87838065962769463, 65.88453944495783787 ) ) ;
#32187 = EDGE_LOOP ( 'NONE', ( #26608, #30720, #3601, #43136 ) ) ;
#32188 = CARTESIAN_POINT ( 'NONE',  ( -20.68074900106244840, -21.00565013100700895, 58.64475149681948807 ) ) ;
#32189 =( BOUNDED_CURVE ( )  B_SPLINE_CURVE ( 3, ( #10551, #45272, #3905, #29267 ),
 .UNSPECIFIED., .F., .F. ) 
 B_SPLINE_CURVE_WITH_KNOTS ( ( 4, 4 ),
 ( 0.9074455897393650661, 1.000000000000000000 ),
 .UNSPECIFIED. ) 
 CURVE ( )  GEOMETRIC_REPRESENTATION_ITEM ( )  RATIONAL_B_SPLINE_CURVE ( ( 0.6983129098260953960, 0.7760317562607003117, 0.8765941196520018464, 1.000000000000000000 ) ) 
 REPRESENTATION_ITEM ( '' )  );
#32190 = ORIENTED_EDGE ( 'NONE', *, *, #39878, .T. ) ;
#32191 = CARTESIAN_POINT ( 'NONE',  ( -16.16748626245079379, -22.20318634978239203, 54.27966884056655061 ) ) ;
#32192 = CARTESIAN_POINT ( 'NONE',  ( -10.37541943412130863, -14.96049300415475436, 75.08306784598362071 ) ) ;
#32193 = ORIENTED_EDGE ( 'NONE', *, *, #47721, .F. ) ;
#32194 = CARTESIAN_POINT ( 'NONE',  ( -19.19784432118828121, -7.503115221654976352, 54.02312124697527196 ) ) ;
#32195 = CARTESIAN_POINT ( 'NONE',  ( -4.424093855413056886, -8.109206544744111511, 51.75000000000000000 ) ) ;
#32196 = CARTESIAN_POINT ( 'NONE',  ( -24.51063837352987207, -17.11019555850099039, 72.99680753360935626 ) ) ;
#32197 = CARTESIAN_POINT ( 'NONE',  ( -23.23616409499838653, -18.79948708312782557, 65.82389430043846801 ) ) ;
#32198 = VERTEX_POINT ( 'NONE', #24361 ) ;
#32199 = FACE_OUTER_BOUND ( 'NONE', #38967, .T. ) ;
#32200 = ADVANCED_FACE ( 'NONE', ( #13960 ), #43564, .F. ) ;
#32201 = CARTESIAN_POINT ( 'NONE',  ( -23.69044173319201363, -11.56146079933792237, 59.63803016077844177 ) ) ;
#32202 = CARTESIAN_POINT ( 'NONE',  ( -23.79253477450064835, -17.84199475294676063, 62.77360976034447759 ) ) ;
#32203 = ORIENTED_EDGE ( 'NONE', *, *, #47185, .T. ) ;
#32204 = CARTESIAN_POINT ( 'NONE',  ( -23.73493062035036871, -11.65830449210876552, 59.48235750863023696 ) ) ;
#32205 = DIRECTION ( 'NONE',  ( -3.413470714839332458E-33, 1.190614954331866791E-16, -1.000000000000000000 ) ) ;
#32206 = ORIENTED_EDGE ( 'NONE', *, *, #15457, .F. ) ;
#32207 = ORIENTED_EDGE ( 'NONE', *, *, #37483, .F. ) ;
#32208 = CARTESIAN_POINT ( 'NONE',  ( -24.15165104652898620, -11.60707627830156952, 63.13873557927141889 ) ) ;
#32209 = LINE ( 'NONE', #5637, #32006 ) ;
#32211 = CARTESIAN_POINT ( 'NONE',  ( -10.02191625022346955, -15.65273779443635327, 61.15293638507743168 ) ) ;
#32210 = VECTOR ( 'NONE', #32055, 1000.000000000000114 ) ;
#32212 = CARTESIAN_POINT ( 'NONE',  ( -17.18034385650552309, -6.424090610841176385, 49.80797279389977916 ) ) ;
#32213 = CARTESIAN_POINT ( 'NONE',  ( -12.29382548908870909, -9.968360400451484082, 64.12094344831615444 ) ) ;
#32214 = CARTESIAN_POINT ( 'NONE',  ( -11.81178328723415660, -10.62567094834893311, 74.73885052262691886 ) ) ;
#32215 = CARTESIAN_POINT ( 'NONE',  ( -41.41379973776600565, -14.80920654474425291, 71.08235294117645253 ) ) ;
#32216 = CARTESIAN_POINT ( 'NONE',  ( -12.01648201532752935, -10.28590752825076926, 67.64896869922044687 ) ) ;
#32217 = AXIS2_PLACEMENT_3D ( 'NONE', #44553, #28801, #25584 ) ;
#32218 = CARTESIAN_POINT ( 'NONE',  ( -23.04402284766838349, -19.06632961612601918, 59.16938527523783620 ) ) ;
#32219 = EDGE_LOOP ( 'NONE', ( #14695, #35310, #32785, #13133, #44941 ) ) ;
#32220 = ORIENTED_EDGE ( 'NONE', *, *, #26544, .T. ) ;
#32221 = CARTESIAN_POINT ( 'NONE',  ( -24.45381059137804058, -15.38184444469599299, 72.88814935371863157 ) ) ;
#32222 = MANIFOLD_SOLID_BREP ( 'Stock-MAS-175-1', #21271 ) ;
#32223 = CARTESIAN_POINT ( 'NONE',  ( -10.63483715323753565, -17.87674169505483235, 71.75213630217804450 ) ) ;
#32224 = CARTESIAN_POINT ( 'NONE',  ( -15.92486819940615916, -7.971526783001416483, 67.44007330037176473 ) ) ;
#32225 = AXIS2_PLACEMENT_3D ( 'NONE', #26885, #12095, #34740 ) ;
#32226 = CARTESIAN_POINT ( 'NONE',  ( -22.38860277241858654, -19.74596283091575089, 72.87230326346423226 ) ) ;
#32227 = CARTESIAN_POINT ( 'NONE',  ( -20.75714322117456945, -21.47287265741918461, 58.83130466214971221 ) ) ;
#32228 = EDGE_CURVE ( 'NONE', #28368, #40867, #20099, .T. ) ;
#32229 = CARTESIAN_POINT ( 'NONE',  ( -21.28659385650551528, -9.302874398569244363, 51.68646062012417985 ) ) ;
#32230 = ORIENTED_EDGE ( 'NONE', *, *, #33737, .F. ) ;
#32231 = CARTESIAN_POINT ( 'NONE',  ( -21.89264518680100835, -20.26253109894388160, 58.77915004610761684 ) ) ;
#32232 = CARTESIAN_POINT ( 'NONE',  ( -10.23413987642072165, -12.85783452779354086, 67.84558203418174571 ) ) ;
#32233 = AXIS2_PLACEMENT_3D ( 'NONE', #17931, #2686, #44801 ) ;
#32234 =( REPRESENTATION_RELATIONSHIP ('NONE','NONE', #2768, #2486 ) REPRESENTATION_RELATIONSHIP_WITH_TRANSFORMATION ( #41767 )SHAPE_REPRESENTATION_RELATIONSHIP( ) );
#32235 = CARTESIAN_POINT ( 'NONE',  ( -14.72744631621160494, -8.295007313424175521, 60.60524229057013201 ) ) ;
#32236 = CARTESIAN_POINT ( 'NONE',  ( -10.08080428754885105, -16.06609343925254763, 68.23413777636764621 ) ) ;
#32237 = VERTEX_POINT ( 'NONE', #40103 ) ;
#32238 = DIRECTION ( 'NONE',  ( 2.081668171172170091E-15, -0.000000000000000000, -1.000000000000000000 ) ) ;
#32239 = CARTESIAN_POINT ( 'NONE',  ( -13.41301606045583128, -21.08813317394188758, 65.17284274790917209 ) ) ;
#32240 = CARTESIAN_POINT ( 'NONE',  ( -12.81584026802821974, -9.539888144265397329, 74.61922966036955529 ) ) ;
#32241 = EDGE_CURVE ( 'NONE', #3454, #8916, #19388, .T. ) ;
#32242 = VECTOR ( 'NONE', #24909, 1000.000000000000114 ) ;
#32243 = CARTESIAN_POINT ( 'NONE',  ( -10.48020486909296523, -13.57339180249324784, 74.56328874061136958 ) ) ;
#32244 = CARTESIAN_POINT ( 'NONE',  ( -15.63492442327685872, -7.577064122408605051, 70.74956509023566298 ) ) ;
#32245 = EDGE_CURVE ( 'NONE', #997, #17474, #34028, .T. ) ;
#32246 = CARTESIAN_POINT ( 'NONE',  ( -14.86627107493491984, -7.811969877679347363, 56.96504568426624360 ) ) ;
#32247 = DIRECTION ( 'NONE',  ( 0.5562740912439652075, 0.8309988781043535777, 7.851267780903552829E-08 ) ) ;
#32248 = ORIENTED_EDGE ( 'NONE', *, *, #34075, .F. ) ;
#32249 = LINE ( 'NONE', #28550, #44832 ) ;
#32250 = CIRCLE ( 'NONE', #44837, 1.250000000000001110 ) ;
#32251 = EDGE_LOOP ( 'NONE', ( #12291, #39086, #44390, #16065, #17491, #2826 ) ) ;
#32252 = CARTESIAN_POINT ( 'NONE',  ( -21.52725980274252393, -9.076272844571150245, 70.43132538913752683 ) ) ;
#32253 = CARTESIAN_POINT ( 'NONE',  ( -15.07409385759798859, -6.859212275519751323, 50.50378509014259265 ) ) ;
#32254 = EDGE_CURVE ( 'NONE', #38352, #25448, #28199, .T. ) ;
#32255 = ORIENTED_EDGE ( 'NONE', *, *, #26397, .T. ) ;
#32256 = DIRECTION ( 'NONE',  ( 1.568615312922261716E-06, 3.599473019824118231E-09, -0.9999999999987697619 ) ) ;
#32257 = CARTESIAN_POINT ( 'NONE',  ( -13.38659385650551847, -9.302874398569244363, 51.68646062012417985 ) ) ;
#32258 = EDGE_LOOP ( 'NONE', ( #1735, #21608, #38509, #8627, #34951 ) ) ;
#32259 = CARTESIAN_POINT ( 'NONE',  ( -23.70015292207183322, -18.82353835121273988, 69.47867366044893345 ) ) ;
#32260 = AXIS2_PLACEMENT_3D ( 'NONE', #38123, #46019, #18936 ) ;
#32261 = EDGE_CURVE ( 'NONE', #20521, #38839, #47723, .T. ) ;
#32262 = CARTESIAN_POINT ( 'NONE',  ( -14.59650283654637271, -21.27602155829186259, 61.78033139454115030 ) ) ;
#32263 = ORIENTED_EDGE ( 'NONE', *, *, #38261, .T. ) ;
#32264 = DIRECTION ( 'NONE',  ( 0.9477661110324762106, -0.3189661404888857743, 2.738326501554842086E-08 ) ) ;
#32265 = DIRECTION ( 'NONE',  ( -3.549360974554993999E-17, 6.371834667797928663E-18, 1.000000000000000000 ) ) ;
#32266 = CARTESIAN_POINT ( 'NONE',  ( -24.03160971261424805, -17.26750559640275640, 69.71339792588547368 ) ) ;
#32267 = DIRECTION ( 'NONE',  ( 0.8244078399817416081, 0.5659962132175737626, 7.627400655798536990E-08 ) ) ;
#32268 = ORIENTED_EDGE ( 'NONE', *, *, #3898, .T. ) ;
#32269 = ORIENTED_EDGE ( 'NONE', *, *, #40556, .F. ) ;
#32270 = DIRECTION ( 'NONE',  ( 0.000000000000000000, 1.000000000000000000, 0.000000000000000000 ) ) ;
#32271 = CARTESIAN_POINT ( 'NONE',  ( -24.30686519033400828, -16.08525344109053634, 62.60831050571806600 ) ) ;
#32272 = ORIENTED_EDGE ( 'NONE', *, *, #31263, .F. ) ;
#32273 = CARTESIAN_POINT ( 'NONE',  ( -17.63801222301331251, -7.812475947363076045, 60.27163990856254117 ) ) ;
#32274 = CARTESIAN_POINT ( 'NONE',  ( -17.42409385541299471, -14.80920654474435594, 52.02966884056656482 ) ) ;
#32275 = CARTESIAN_POINT ( 'NONE',  ( -19.79909385759798823, -8.105421454601382081, 49.25000573077640098 ) ) ;
#32276 = CARTESIAN_POINT ( 'NONE',  ( -10.42593258563390712, -14.97222729729766044, 74.81281306951763099 ) ) ;
#32277 = EDGE_CURVE ( 'NONE', #1628, #13690, #6118, .T. ) ;
#32278 = LINE ( 'NONE', #5204, #8632 ) ;
#32279 = CARTESIAN_POINT ( 'NONE',  ( -19.42896739221782809, -21.56812523091047851, 62.29503644570711174 ) ) ;
#32280 = EDGE_CURVE ( 'NONE', #12981, #34525, #45216, .T. ) ;
#32281 = ORIENTED_EDGE ( 'NONE', *, *, #42818, .T. ) ;
#32282 = LINE ( 'NONE', #5927, #16264 ) ;
#32283 = CARTESIAN_POINT ( 'NONE',  ( -14.88752825633713606, -21.38711684928872003, 61.63600437443167834 ) ) ;
#32284 = AXIS2_PLACEMENT_3D ( 'NONE', #40886, #2963, #17733 ) ;
#32285 = CARTESIAN_POINT ( 'NONE',  ( -22.84295050904691138, -9.696552564295293664, 73.67499385951728641 ) ) ;
#32286 = PLANE ( 'NONE',  #38700 ) ;
#32287 = EDGE_CURVE ( 'NONE', #73, #7134, #30247, .T. ) ;
#32288 = ORIENTED_EDGE ( 'NONE', *, *, #44137, .T. ) ;
#32289 = B_SPLINE_CURVE_WITH_KNOTS ( 'NONE', 3,
 ( #20007, #16046, #35008, #47075, #46107, #13316, #39681, #46830, #24187, #5952 ),
 .UNSPECIFIED., .F., .F.,
 ( 4, 2, 2, 2, 4 ),
 ( 0.6272669072782346422, 0.7522669073001380102, 0.8772669073220412672, 1.002266907343944524, 1.127266907365847892 ),
 .UNSPECIFIED. ) ;
#32290 = ORIENTED_EDGE ( 'NONE', *, *, #8078, .F. ) ;
#32291 = CARTESIAN_POINT ( 'NONE',  ( -24.47066272824306665, -14.57993217219608795, 62.99824437345093031 ) ) ;
#32292 = CARTESIAN_POINT ( 'NONE',  ( -42.17145494138591033, -14.90920654474420104, 65.02111131221717244 ) ) ;
#32293 = CARTESIAN_POINT ( 'NONE',  ( -10.00731240618708462, -14.10555136595099945, 61.10316694600977172 ) ) ;
#32294 = VECTOR ( 'NONE', #17831, 1000.000000000000227 ) ;
#32295 = ORIENTED_EDGE ( 'NONE', *, *, #23237, .F. ) ;
#32296 = CARTESIAN_POINT ( 'NONE',  ( -16.16815255583688682, -7.465780795815666337, 60.39302609866659566 ) ) ;
#32297 = AXIS2_PLACEMENT_3D ( 'NONE', #7977, #4750, #8696 ) ;
#32298 = VERTEX_POINT ( 'NONE', #48444 ) ;
#32299 = CARTESIAN_POINT ( 'NONE',  ( -13.70540922824953078, -21.34346593505471290, 53.76227901944321275 ) ) ;
#32300 = EDGE_LOOP ( 'NONE', ( #32368, #42484 ) ) ;
#32301 = LINE ( 'NONE', #35726, #1338 ) ;
#32302 = VERTEX_POINT ( 'NONE', #25800 ) ;
#32303 = DIRECTION ( 'NONE',  ( -2.575747231244379256E-06, 1.267954838346457742E-05, 0.9999999999162972886 ) ) ;
#32304 = ORIENTED_EDGE ( 'NONE', *, *, #26264, .T. ) ;
#32305 = CARTESIAN_POINT ( 'NONE',  ( -11.96181431063714484, -19.87549516500596525, 58.11177798925346139 ) ) ;
#32306 = DIRECTION ( 'NONE',  ( 0.4683180279402421875, -0.8835599723313410925, 4.589753183357165266E-08 ) ) ;
#32307 = ADVANCED_FACE ( 'NONE', ( #14936 ), #35183, .T. ) ;
#32308 = DIRECTION ( 'NONE',  ( 1.000000000000000000, 1.669677910507523057E-21, 6.493791346278465266E-22 ) ) ;
#32309 = ORIENTED_EDGE ( 'NONE', *, *, #33095, .T. ) ;
#32310 = DIRECTION ( 'NONE',  ( -3.071710424422018668E-17, 6.404604876783312462E-16, 1.000000000000000000 ) ) ;
#32311 = CARTESIAN_POINT ( 'NONE',  ( -20.16691314815865255, -21.73601827195274794, 72.58974169946205279 ) ) ;
#32312 = DIRECTION ( 'NONE',  ( -0.3478314405900310158, -0.9375570856950865561, 0.000000000000000000 ) ) ;
#32313 = ADVANCED_FACE ( 'NONE', ( #18154 ), #37107, .T. ) ;
#32314 = CIRCLE ( 'NONE', #23642, 5.249999999999998224 ) ;
#32315 =( BOUNDED_CURVE ( )  B_SPLINE_CURVE ( 3, ( #43176, #9451, #39481, #21007 ),
 .UNSPECIFIED., .F., .F. ) 
 B_SPLINE_CURVE_WITH_KNOTS ( ( 4, 4 ),
 ( 0.000000000000000000, 0.4074455897393719495 ),
 .UNSPECIFIED. ) 
 CURVE ( )  GEOMETRIC_REPRESENTATION_ITEM ( )  RATIONAL_B_SPLINE_CURVE ( ( 1.000000000000000000, 0.4567392136813254733, 0.3561768502900278799, 0.6983129098261073864 ) ) 
 REPRESENTATION_ITEM ( '' )  );
#32316 = CARTESIAN_POINT ( 'NONE',  ( -22.51726279860821478, -19.68384809141797120, 72.64400547081167758 ) ) ;
#32317 = CARTESIAN_POINT ( 'NONE',  ( -23.99312268326606201, -11.29471679256767125, 66.60709928216182618 ) ) ;
#32318 = CARTESIAN_POINT ( 'NONE',  ( -45.37196614242555626, -14.20920654474410760, 70.13000000000000966 ) ) ;
#32319 = VERTEX_POINT ( 'NONE', #15188 ) ;
#32320 = VECTOR ( 'NONE', #25266, 1000.000000000000341 ) ;
#32321 = CARTESIAN_POINT ( 'NONE',  ( -17.59211730330735435, -7.811223398082945302, 63.85057029380297422 ) ) ;
#32322 = CARTESIAN_POINT ( 'NONE',  ( -11.88825570308877211, -19.09342130031698304, 71.79571799091935702 ) ) ;
#32323 = DIRECTION ( 'NONE',  ( -3.071710424422018668E-17, 6.404604876783312462E-16, 1.000000000000000000 ) ) ;
#32324 = DIRECTION ( 'NONE',  ( -0.9959323210854037489, 0.09010444948746665350, 2.601165157765155817E-08 ) ) ;
#32325 = CARTESIAN_POINT ( 'NONE',  ( -19.96356197875924110, -21.81308687000214874, 69.04144176266291311 ) ) ;
#32326 = CARTESIAN_POINT ( 'NONE',  ( -24.26647797581570032, -16.29234248507571081, 62.82158650101273167 ) ) ;
#32327 = ORIENTED_EDGE ( 'NONE', *, *, #6136, .F. ) ;
#32328 = ORIENTED_EDGE ( 'NONE', *, *, #15725, .T. ) ;
#32329 = CARTESIAN_POINT ( 'NONE',  ( -21.18398698114219769, -21.24092341087395752, 65.69958654271196963 ) ) ;
#32330 = PLANE ( 'NONE',  #13945 ) ;
#32331 = VERTEX_POINT ( 'NONE', #44525 ) ;
#32332 = CARTESIAN_POINT ( 'NONE',  ( 18.62590614458706995, 3.140741878271803067, 50.53406581128081143 ) ) ;
#32333 = FACE_OUTER_BOUND ( 'NONE', #26308, .T. ) ;
#32334 = CARTESIAN_POINT ( 'NONE',  ( -12.79487214375358839, -8.971058656907512585, 71.03580700614087107 ) ) ;
#32335 = CARTESIAN_POINT ( 'NONE',  ( -23.12302657392458016, -18.95946740514217765, 62.35406880581413702 ) ) ;
#32336 = CARTESIAN_POINT ( 'NONE',  ( -17.00424539706637361, -22.24753552852095950, 72.32576587678371993 ) ) ;
#32337 = VERTEX_POINT ( 'NONE', #33403 ) ;
#32338 = EDGE_CURVE ( 'NONE', #11839, #33399, #14677, .T. ) ;
#32339 = FACE_OUTER_BOUND ( 'NONE', #27711, .T. ) ;
#32340 =( BOUNDED_SURFACE ( )  B_SPLINE_SURFACE ( 3, 1, ( 
 ( #27315, #42827 ),
 ( #5161, #35178 ),
 ( #19934, #1449 ),
 ( #1205, #19440 ),
 ( #38640, #4420 ),
 ( #12294, #19693 ),
 ( #8620, #42101 ) ),
 .UNSPECIFIED., .T., .F., .F. ) 
 B_SPLINE_SURFACE_WITH_KNOTS ( ( 4, 3, 4 ),
 ( 2, 2 ),
 ( 0.000000000000000000, 0.5000000000000000000, 1.000000000000000000 ),
 ( 0.000000000000000000, 1.000000000000000000 ),
 .UNSPECIFIED. ) 
 GEOMETRIC_REPRESENTATION_ITEM ( )  RATIONAL_B_SPLINE_SURFACE ( (
 ( 1.000000000000000000, 1.000000000000000000),
 ( 0.3333333333333335369, 0.3333333333333330373),
 ( 0.3333333333333335369, 0.3333333333333330373),
 ( 1.000000000000000000, 1.000000000000000000),
 ( 0.3333333333333333703, 0.3333333333333333703),
 ( 0.3333333333333333703, 0.3333333333333333703),
 ( 1.000000000000000000, 1.000000000000000000) ) ) 
 REPRESENTATION_ITEM ( '' )  SURFACE ( )  );
#32341 = ADVANCED_FACE ( 'NONE', ( #48696 ), #47968, .T. ) ;
#32342 = CARTESIAN_POINT ( 'NONE',  ( -10.83536388074712598, -17.31742051234312640, 64.92739380450886699 ) ) ;
#32343 = DIRECTION ( 'NONE',  ( -3.413470714839332458E-33, 1.190614954331866791E-16, -1.000000000000000000 ) ) ;
#32344 = ADVANCED_FACE ( 'NONE', ( #11031 ), #14204, .T. ) ;
#32345 = EDGE_CURVE ( 'NONE', #25341, #31554, #41070, .T. ) ;
#32346 = EDGE_CURVE ( 'NONE', #35350, #47755, #31162, .T. ) ;
#32347 = EDGE_LOOP ( 'NONE', ( #12235, #1546, #46001, #19924 ) ) ;
#32348 = CIRCLE ( 'NONE', #11094, 0.7500000000000023315 ) ;
#32349 = CARTESIAN_POINT ( 'NONE',  ( -21.66670709193873634, -21.01608934220539027, 54.02312124697527906 ) ) ;
#32350 = FILL_AREA_STYLE ('',( #43676 ) ) ;
#32351 = CARTESIAN_POINT ( 'NONE',  ( -22.51726247777427758, -19.68384842258191725, 72.94400547081133368 ) ) ;
#32352 = CARTESIAN_POINT ( 'NONE',  ( -21.13865688766858142, -18.88351593698935105, 53.69233794759168177 ) ) ;
#32353 = CARTESIAN_POINT ( 'NONE',  ( -11.58273374504420516, -10.94902345701756730, 57.39830395176002042 ) ) ;
#32354 = EDGE_LOOP ( 'NONE', ( #40065, #36987, #45866, #24375, #3207 ) ) ;
#32355 = ORIENTED_EDGE ( 'NONE', *, *, #42919, .T. ) ;
#32356 = CARTESIAN_POINT ( 'NONE',  ( -16.33659385541304232, -8.995762431863214559, 51.38120296130585274 ) ) ;
#32357 = AXIS2_PLACEMENT_3D ( 'NONE', #41981, #19317, #34085 ) ;
#32358 = CARTESIAN_POINT ( 'NONE',  ( -13.19865322091292370, -9.228302641792829775, 63.98234477754206750 ) ) ;
#32359 = VECTOR ( 'NONE', #37076, 999.9999999999998863 ) ;
#32360 = FACE_OUTER_BOUND ( 'NONE', #18038, .T. ) ;
#32361 = CIRCLE ( 'NONE', #25283, 2.000000000000000444 ) ;
#32362 = CARTESIAN_POINT ( 'NONE',  ( -23.00382044653182945, -10.58231046269237829, 59.60203429539187425 ) ) ;
#32363 = EDGE_CURVE ( 'NONE', #17990, #48035, #7594, .T. ) ;
#32364 = DIRECTION ( 'NONE',  ( -3.071710424422018668E-17, 6.404604876783312462E-16, 1.000000000000000000 ) ) ;
#32365 = VERTEX_POINT ( 'NONE', #21861 ) ;
#32366 = AXIS2_PLACEMENT_3D ( 'NONE', #27859, #24175, #5467 ) ;
#32367 = DIRECTION ( 'NONE',  ( 0.000000000000000000, 0.000000000000000000, -1.000000000000000000 ) ) ;
#32368 = ORIENTED_EDGE ( 'NONE', *, *, #20631, .T. ) ;
#32369 = CARTESIAN_POINT ( 'NONE',  ( -17.99281169931935409, -22.23759039661181802, 61.99723177674093222 ) ) ;
#32370 = CARTESIAN_POINT ( 'NONE',  ( -12.90644216781524811, -9.461594527793637965, 74.33539679058131355 ) ) ;
#32371 = ORIENTED_EDGE ( 'NONE', *, *, #21942, .F. ) ;
#32372 = CARTESIAN_POINT ( 'NONE',  ( -10.64331041279003642, -16.74977650942914309, 58.10249305398041741 ) ) ;
#32373 = CARTESIAN_POINT ( 'NONE',  ( -18.64924655410156973, -21.70115844427598617, 72.39396872550724993 ) ) ;
#32374 = VERTEX_POINT ( 'NONE', #36861 ) ;
#32375 = VECTOR ( 'NONE', #24690, 1000.000000000000000 ) ;
#32376 = EDGE_CURVE ( 'NONE', #46955, #13463, #34644, .T. ) ;
#32377 = CARTESIAN_POINT ( 'NONE',  ( -24.41290230071813383, -15.73718799205770935, 69.82747671076849372 ) ) ;
#32378 = CARTESIAN_POINT ( 'NONE',  ( -24.69822963474414479, -13.19963333263893190, 59.54763306486673713 ) ) ;
#32379 = ORIENTED_EDGE ( 'NONE', *, *, #44027, .T. ) ;
#32380 = CARTESIAN_POINT ( 'NONE',  ( -21.84103824432629892, -20.31425616591354455, 62.37872033649042436 ) ) ;
#32381 = CARTESIAN_POINT ( 'NONE',  ( -19.80301194551662647, -21.44571530912114099, 68.93482476707502826 ) ) ;
#32382 = PRESENTATION_LAYER_ASSIGNMENT (  '', '', ( #21385 ) ) ;
#32383 = DIRECTION ( 'NONE',  ( -3.071710424422018668E-17, 6.404604876783312462E-16, 1.000000000000000000 ) ) ;
#32384 = CARTESIAN_POINT ( 'NONE',  ( -10.76763551407085373, -17.13171859787639661, 61.45743118825841833 ) ) ;
#32385 = VECTOR ( 'NONE', #10692, 1000.000000000000000 ) ;
#32386 = PLANE ( 'NONE',  #22779 ) ;
#32387 = CARTESIAN_POINT ( 'NONE',  ( -23.35262004249965528, -18.62986191134476499, 65.70900547832829375 ) ) ;
#32388 = ORIENTED_EDGE ( 'NONE', *, *, #1273, .T. ) ;
#32389 = CARTESIAN_POINT ( 'NONE',  ( -18.50932193227059486, -21.77517953109191140, 72.58510940649487964 ) ) ;
#32390 = CARTESIAN_POINT ( 'NONE',  ( -50.42609385541305755, -14.90920654474422058, 68.06470588235292496 ) ) ;
#32391 = VERTEX_POINT ( 'NONE', #14434 ) ;
#32392 = LINE ( 'NONE', #32148, #1913 ) ;
#32393 = VERTEX_POINT ( 'NONE', #22350 ) ;
#32394 = EDGE_CURVE ( 'NONE', #10444, #37822, #22897, .T. ) ;
#32395 = ADVANCED_FACE ( 'NONE', ( #18639 ), #6859, .T. ) ;
#32396 = ORIENTED_EDGE ( 'NONE', *, *, #17601, .T. ) ;
#32397 = ORIENTED_EDGE ( 'NONE', *, *, #8543, .T. ) ;
#32398 = CARTESIAN_POINT ( 'NONE',  ( -18.75871633935533112, -7.479601620491856728, 70.49255234965639261 ) ) ;
#32399 = CIRCLE ( 'NONE', #44191, 5.249999999999998224 ) ;
#32400 = CARTESIAN_POINT ( 'NONE',  ( -12.81450638858427737, -9.474958432310776502, 74.46923006088778152 ) ) ;
#32401 = FACE_BOUND ( 'NONE', #21239, .T. ) ;
#32402 = CARTESIAN_POINT ( 'NONE',  ( -22.10534385759799392, -7.595227055684746986, 51.75156210489594599 ) ) ;
#32403 = ORIENTED_EDGE ( 'NONE', *, *, #41450, .F. ) ;
#32404 = ORIENTED_EDGE ( 'NONE', *, *, #19369, .T. ) ;
#32405 = EDGE_CURVE ( 'NONE', #5198, #27631, #21968, .T. ) ;
#32406 = EDGE_CURVE ( 'NONE', #27240, #20428, #26457, .T. ) ;
#32407 = CARTESIAN_POINT ( 'NONE',  ( -17.77409385650551243, -9.792211528768504536, 50.49490371617623197 ) ) ;
#32408 = CARTESIAN_POINT ( 'NONE',  ( -11.47692143115784447, -10.32194432912726612, 74.56168219205009962 ) ) ;
#32409 = CARTESIAN_POINT ( 'NONE',  ( -23.21840254553152860, -18.73701819181863470, 66.12389378410178153 ) ) ;
#32410 = CARTESIAN_POINT ( 'NONE',  ( -17.71784385650551741, -9.790100578890868377, 49.79778022625163203 ) ) ;
#32411 = ORIENTED_EDGE ( 'NONE', *, *, #44462, .F. ) ;
#32412 = EDGE_CURVE ( 'NONE', #37238, #10228, #29246, .T. ) ;
#32413 = CARTESIAN_POINT ( 'NONE',  ( -23.92594474375018621, -12.07410526313069887, 59.78235714318768856 ) ) ;
#32414 = AXIS2_PLACEMENT_3D ( 'NONE', #31617, #35540, #27427 ) ;
#32415 = LINE ( 'NONE', #17846, #38596 ) ;
#32416 = EDGE_LOOP ( 'NONE', ( #16594, #26510, #27070, #1878 ) ) ;
#32417 = DIRECTION ( 'NONE',  ( 0.9687793358424821033, -0.2479245821708679909, 0.000000000000000000 ) ) ;
#32418 = ORIENTED_EDGE ( 'NONE', *, *, #3831, .F. ) ;
#32419 = CARTESIAN_POINT ( 'NONE',  ( -22.40414025807384135, -9.889859561998502357, 73.55449203743623343 ) ) ;
#32420 = DIRECTION ( 'NONE',  ( 1.000000000000000000, 2.866981220435666553E-17, 0.000000000000000000 ) ) ;
#32421 = CARTESIAN_POINT ( 'NONE',  ( -13.71283467540607504, -11.09584481999758054, 52.02966884056656482 ) ) ;
#32422 = ORIENTED_EDGE ( 'NONE', *, *, #21502, .F. ) ;
#32423 = CARTESIAN_POINT ( 'NONE',  ( -21.93588290314558620, -13.54151500546508657, 52.02966884056656482 ) ) ;
#32424 = CARTESIAN_POINT ( 'NONE',  ( -11.25989433568914855, -11.38792842781904469, 64.44882039367774951 ) ) ;
#32425 = CARTESIAN_POINT ( 'NONE',  ( -10.38996398380459318, -17.26349193673827287, 61.30743118028662764 ) ) ;
#32426 = VERTEX_POINT ( 'NONE', #23579 ) ;
#32427 = CARTESIAN_POINT ( 'NONE',  ( -20.76327734442119066, -20.96149803180293247, 58.71763231260016624 ) ) ;
#32428 = CARTESIAN_POINT ( 'NONE',  ( -18.24929096724884658, -21.81104555038653103, 68.82986815895560540 ) ) ;
#32429 = VERTEX_POINT ( 'NONE', #19387 ) ;
#32430 = CARTESIAN_POINT ( 'NONE',  ( -11.10470791607724550, -18.75498134223953883, 61.46206221440264983 ) ) ;
#32431 = CARTESIAN_POINT ( 'NONE',  ( -9.983342151361524586, -14.43473985968501339, 67.99766747612557083 ) ) ;
#32432 = ORIENTED_EDGE ( 'NONE', *, *, #31918, .F. ) ;
#32433 = CARTESIAN_POINT ( 'NONE',  ( -21.06635048418738165, -21.30826373965517817, 62.29966805574095901 ) ) ;
#32434 = CARTESIAN_POINT ( 'NONE',  ( -13.68948761385293800, -20.72981242130265045, 61.74319555004421289 ) ) ;
#32435 = CARTESIAN_POINT ( 'NONE',  ( -24.11881394502254849, -17.01995806294775448, 73.16863963025599560 ) ) ;
#32436 = DIRECTION ( 'NONE',  ( 0.000000000000000000, 0.9999954153791273948, 0.003028072113820366902 ) ) ;
#32437 = ORIENTED_EDGE ( 'NONE', *, *, #43145, .T. ) ;
#32438 = CARTESIAN_POINT ( 'NONE',  ( -21.98930223717667332, -9.502567820616416583, 60.02171225693719947 ) ) ;
#32439 = CARTESIAN_POINT ( 'NONE',  ( -19.05445285856947990, -7.539616405147045342, 67.04038455535467733 ) ) ;
#32440 = DIRECTION ( 'NONE',  ( 0.5351595679979588294, 0.8447509909909772796, 1.584200591473933048E-17 ) ) ;
#32441 = VERTEX_POINT ( 'NONE', #27503 ) ;
#32442 = CARTESIAN_POINT ( 'NONE',  ( -23.91010245674826251, -17.57297063409389537, 62.75888927877479517 ) ) ;
#32443 = CARTESIAN_POINT ( 'NONE',  ( -24.65061889199765233, -12.99785316138012270, 62.87618224063605510 ) ) ;
#32444 = EDGE_CURVE ( 'NONE', #744, #33284, #27668, .T. ) ;
#32445 = ORIENTED_EDGE ( 'NONE', *, *, #21156, .T. ) ;
#32446 = VERTEX_POINT ( 'NONE', #42536 ) ;
#32447 = CARTESIAN_POINT ( 'NONE',  ( -23.59778322581706789, -11.38860327479983603, 63.10785482661193413 ) ) ;
#32448 = CARTESIAN_POINT ( 'NONE',  ( -13.00647906721701297, -9.304695462141918227, 64.06513368409466125 ) ) ;
#32449 = CARTESIAN_POINT ( 'NONE',  ( -11.33842141989115504, -11.24277552151799497, 57.20902919577373069 ) ) ;
#32450 = CARTESIAN_POINT ( 'NONE',  ( -17.34909385650551883, -8.104110260919579645, 48.81699501597546487 ) ) ;
#32451 = CARTESIAN_POINT ( 'NONE',  ( -10.50893933415051507, -13.43540278197274063, 74.96345540680638919 ) ) ;
#32452 = CARTESIAN_POINT ( 'NONE',  ( -19.41474841345058522, -21.52018966427049307, 62.29503644830997189 ) ) ;
#32453 =( BOUNDED_CURVE ( )  B_SPLINE_CURVE ( 3, ( #19592, #39027, #34600, #5305 ),
 .UNSPECIFIED., .F., .F. ) 
 B_SPLINE_CURVE_WITH_KNOTS ( ( 4, 4 ),
 ( 4.712388980384689674, 4.921828490624009511 ),
 .UNSPECIFIED. ) 
 CURVE ( )  GEOMETRIC_REPRESENTATION_ITEM ( )  RATIONAL_B_SPLINE_CURVE ( ( 1.000000000000000000, 0.9963479302455154896, 0.9963479302455154896, 1.000000000000000000 ) ) 
 REPRESENTATION_ITEM ( '' )  );
#32454 = CARTESIAN_POINT ( 'NONE',  ( -21.25771322586351886, -21.19734792347225749, 65.72307405023113347 ) ) ;
#32455 = CARTESIAN_POINT ( 'NONE',  ( -12.19296425323979882, -20.11394705437778896, 65.02821367433101329 ) ) ;
#32456 = CARTESIAN_POINT ( 'NONE',  ( -10.86088752666615065, -11.28245350497684818, 67.80519939327926693 ) ) ;
#32457 = ORIENTED_EDGE ( 'NONE', *, *, #28655, .F. ) ;
#32458 = VERTEX_POINT ( 'NONE', #38322 ) ;
#32459 = EDGE_CURVE ( 'NONE', #40402, #12408, #18800, .T. ) ;
#32460 = DIRECTION ( 'NONE',  ( -2.842893132017732099E-07, 1.090087350972575656E-07, -0.9999999999999535927 ) ) ;
#32461 = EDGE_CURVE ( 'NONE', #18891, #13748, #5104, .T. ) ;
#32462 = DIRECTION ( 'NONE',  ( 0.9687793358424817702, -0.2479245821708688791, 0.000000000000000000 ) ) ;
#32463 = CARTESIAN_POINT ( 'NONE',  ( -21.80947544975385810, -9.353161466788067813, 63.19153755920122251 ) ) ;
#32464 = CARTESIAN_POINT ( 'NONE',  ( -18.97054302448013985, -7.521389842619064403, 67.08567168106696954 ) ) ;
#32465 = CARTESIAN_POINT ( 'NONE',  ( -11.06571665854733766, -11.88142629960236718, 71.31534231900744203 ) ) ;
#32466 = EDGE_CURVE ( 'NONE', #29981, #44852, #5288, .T. ) ;
#32467 = CARTESIAN_POINT ( 'NONE',  ( -19.93659385650551741, -6.915538690918074494, 49.31353937987644542 ) ) ;
#32468 =( BOUNDED_CURVE ( )  B_SPLINE_CURVE ( 2, ( #3496, #10655, #33269, #36970, #17107, #31909, #46926, #36070, #27965 ),
 .UNSPECIFIED., .F., .F. ) 
 B_SPLINE_CURVE_WITH_KNOTS ( ( 3, 2, 2, 2, 3 ),
 ( 0.6666666666666665186, 0.6770833333333332593, 0.6874999999999998890, 0.6979166666666665186, 0.7083333333333332593 ),
 .UNSPECIFIED. ) 
 CURVE ( )  GEOMETRIC_REPRESENTATION_ITEM ( )  RATIONAL_B_SPLINE_CURVE ( ( 1.000000000000000888, 0.9238795325112859613, 1.000000000000000000, 0.9238795325112867385, 1.000000000000000000, 0.9238795325112867385, 1.000000000000000000, 0.9238795325112875156, 0.9999999999999992228 ) ) 
 REPRESENTATION_ITEM ( '' )  );
#32469 = ORIENTED_EDGE ( 'NONE', *, *, #34694, .F. ) ;
#32470 = CARTESIAN_POINT ( 'NONE',  ( -20.04849592361258104, -21.35284569240296548, 72.69006679631316103 ) ) ;
#32471 = DIRECTION ( 'NONE',  ( -3.071710424422018668E-17, 6.404604876783312462E-16, 1.000000000000000000 ) ) ;
#32472 = CARTESIAN_POINT ( 'NONE',  ( -14.60628068055246942, -7.912570010659592867, 60.36350377317607752 ) ) ;
#32473 = CARTESIAN_POINT ( 'NONE',  ( -11.17436915487612303, -18.86448991569423939, 64.86990214591243387 ) ) ;
#32474 = EDGE_LOOP ( 'NONE', ( #31713, #20904 ) ) ;
#32475 =( BOUNDED_SURFACE ( )  B_SPLINE_SURFACE ( 3, 1, ( 
 ( #4440, #7916 ),
 ( #22674, #12311 ),
 ( #22936, #279 ),
 ( #15258, #15011 ),
 ( #27333, #755 ),
 ( #19457, #37675 ),
 ( #15751, #34465 ) ),
 .UNSPECIFIED., .T., .F., .F. ) 
 B_SPLINE_SURFACE_WITH_KNOTS ( ( 4, 3, 4 ),
 ( 2, 2 ),
 ( 0.000000000000000000, 0.5000000000000000000, 1.000000000000000000 ),
 ( 0.000000000000000000, 1.000000000000000000 ),
 .UNSPECIFIED. ) 
 GEOMETRIC_REPRESENTATION_ITEM ( )  RATIONAL_B_SPLINE_SURFACE ( (
 ( 1.000000000000000000, 1.000000000000000000),
 ( 0.3333333333333335369, 0.3333333333333330373),
 ( 0.3333333333333335369, 0.3333333333333330373),
 ( 1.000000000000000000, 1.000000000000000000),
 ( 0.3333333333333333703, 0.3333333333333333703),
 ( 0.3333333333333333703, 0.3333333333333333703),
 ( 1.000000000000000000, 1.000000000000000000) ) ) 
 REPRESENTATION_ITEM ( '' )  SURFACE ( )  );
#32476 = LINE ( 'NONE', #28778, #12546 ) ;
#32477 = CARTESIAN_POINT ( 'NONE',  ( -12.84719963800786502, -9.512789006345032661, 74.31923006385322594 ) ) ;
#32478 = CARTESIAN_POINT ( 'NONE',  ( -15.59637485834756809, -7.586876612986846347, 70.81001046420034584 ) ) ;
#32479 = CARTESIAN_POINT ( 'NONE',  ( -16.03921789102526674, -7.892880921105984271, 60.40848222778001997 ) ) ;
#32480 = ORIENTED_EDGE ( 'NONE', *, *, #2274, .F. ) ;
#32481 = CARTESIAN_POINT ( 'NONE',  ( -22.96484330895583881, -19.08706763331013434, 59.18410642315183878 ) ) ;
#32482 = ORIENTED_EDGE ( 'NONE', *, *, #24414, .F. ) ;
#32483 = CARTESIAN_POINT ( 'NONE',  ( -44.71706047250183502, -12.89566876303302756, 70.50000000000000000 ) ) ;
#32484 = ORIENTED_EDGE ( 'NONE', *, *, #25609, .F. ) ;
#32485 = PLANE ( 'NONE',  #10831 ) ;
#32486 = CARTESIAN_POINT ( 'NONE',  ( -14.73659385650551457, -6.915538690918075382, 49.31353937987644542 ) ) ;
#32487 = ORIENTED_EDGE ( 'NONE', *, *, #13467, .T. ) ;
#32488 = DIRECTION ( 'NONE',  ( 1.000000000000000000, 0.000000000000000000, 0.000000000000000000 ) ) ;
#32489 = EDGE_CURVE ( 'NONE', #36372, #41560, #19805, .T. ) ;
#32490 = DIRECTION ( 'NONE',  ( -2.081668171172170091E-15, 0.000000000000000000, 1.000000000000000000 ) ) ;
#32491 = DIRECTION ( 'NONE',  ( 0.9687793358424821033, -0.2479245821708679909, 0.000000000000000000 ) ) ;
#32492 = VERTEX_POINT ( 'NONE', #38578 ) ;
#32493 = B_SPLINE_CURVE_WITH_KNOTS ( 'NONE', 3,
 ( #25498, #33103, #31749, #33342, #43065, #47256, #29435, #10718, #14618, #17188 ),
 .UNSPECIFIED., .F., .F.,
 ( 4, 2, 2, 2, 4 ),
 ( 0.000000000000000000, 0.2500000000000000000, 0.5000000000000000000, 0.7500000000000000000, 1.000000000000000000 ),
 .UNSPECIFIED. ) ;
#32494 = CARTESIAN_POINT ( 'NONE',  ( -10.47299139157196990, -15.63514485490427575, 61.03789045487297926 ) ) ;
#32495 = CARTESIAN_POINT ( 'NONE',  ( -21.00380318978402627, -21.34292366101719196, 62.22975991904223747 ) ) ;
#32496 = B_SPLINE_CURVE_WITH_KNOTS ( 'NONE', 3,
 ( #46404, #23998, #39001, #5279, #22233, #9941, #44184, #18027, #3274, #6250 ),
 .UNSPECIFIED., .F., .F.,
 ( 4, 2, 2, 2, 4 ),
 ( 0.000000000000000000, 0.2500000000000000000, 0.5000000000000000000, 0.7500000000000000000, 1.000000000000000000 ),
 .UNSPECIFIED. ) ;
#32497 = CARTESIAN_POINT ( 'NONE',  ( -11.96916353976625835, -10.42234295362220919, 67.57184930830715075 ) ) ;
#32498 = CYLINDRICAL_SURFACE ( 'NONE', #12219, 4.686499999999997002 ) ;
#32499 = ORIENTED_EDGE ( 'NONE', *, *, #4638, .T. ) ;
#32500 = ORIENTED_EDGE ( 'NONE', *, *, #6339, .F. ) ;
#32501 = LINE ( 'NONE', #47527, #30658 ) ;
#32502 = CARTESIAN_POINT ( 'NONE',  ( -13.09516132467690674, -9.240204434965294311, 64.11766254823847078 ) ) ;
#32503 = ORIENTED_EDGE ( 'NONE', *, *, #7462, .T. ) ;
#32504 = CARTESIAN_POINT ( 'NONE',  ( -20.75918756122348441, -8.147305293919229641, 63.42626095967343502 ) ) ;
#32505 = CARTESIAN_POINT ( 'NONE',  ( -18.95534385759798823, -8.623186033802570094, 49.24843789510466507 ) ) ;
#32506 = CARTESIAN_POINT ( 'NONE',  ( -23.25657551529890554, -10.17392617991681192, 63.32831932546986309 ) ) ;
#32507 = CARTESIAN_POINT ( 'NONE',  ( 23.52590614458706852, 1.890747609047893185, 50.53028072113869484 ) ) ;
#32508 = CARTESIAN_POINT ( 'NONE',  ( -12.40526403761170648, -9.927684372832816351, 60.78747871995254570 ) ) ;
#32509 = ORIENTED_EDGE ( 'NONE', *, *, #25336, .F. ) ;
#32510 = CARTESIAN_POINT ( 'NONE',  ( -21.94239175829699207, -20.22099772874085488, 59.06442899522711087 ) ) ;
#32511 = CYLINDRICAL_SURFACE ( 'NONE', #40013, 1.999999999999999112 ) ;
#32512 = EDGE_CURVE ( 'NONE', #24436, #1563, #27021, .T. ) ;
#32513 = DIRECTION ( 'NONE',  ( -0.9180681052388980357, 0.3964226963016364014, 0.000000000000000000 ) ) ;
#32514 = CARTESIAN_POINT ( 'NONE',  ( -16.58980513972923276, -22.21251475926257513, 65.38597725124276394 ) ) ;
#32515 = EDGE_CURVE ( 'NONE', #40340, #43582, #28870, .T. ) ;
#32516 = ORIENTED_EDGE ( 'NONE', *, *, #8161, .T. ) ;
#32517 = EDGE_CURVE ( 'NONE', #6262, #20123, #27005, .T. ) ;
#32518 = ORIENTED_EDGE ( 'NONE', *, *, #18522, .F. ) ;
#32519 = CARTESIAN_POINT ( 'NONE',  ( -10.88757861317511200, -12.29993006150962387, 57.51784320375504933 ) ) ;
#32520 = CARTESIAN_POINT ( 'NONE',  ( -12.34368963248081918, -19.70250163048094905, 65.16674848656688823 ) ) ;
#32521 = DIRECTION ( 'NONE',  ( 2.181982678098338148E-16, 0.000000000000000000, -1.000000000000000000 ) ) ;
#32522 = B_SPLINE_CURVE_WITH_KNOTS ( 'NONE', 1,
 ( #33064, #14339 ),
 .UNSPECIFIED., .F., .F.,
 ( 2, 2 ),
 ( 0.000000000000000000, 1.000000000000000000 ),
 .UNSPECIFIED. ) ;
#32523 = EDGE_CURVE ( 'NONE', #17454, #47981, #22975, .T. ) ;
#32524 = ORIENTED_EDGE ( 'NONE', *, *, #32916, .F. ) ;
#32525 = CARTESIAN_POINT ( 'NONE',  ( -23.93648101794248362, -17.51022725521227841, 65.95829288617392194 ) ) ;
#32526 = CARTESIAN_POINT ( 'NONE',  ( -10.92750371411227128, -11.16255126880030701, 64.26386748351472988 ) ) ;
#32527 = CIRCLE ( 'NONE', #48231, 5.249999999999998224 ) ;
#32528 = ORIENTED_EDGE ( 'NONE', *, *, #11093, .T. ) ;
#32529 = LINE ( 'NONE', #47554, #11116 ) ;
#32530 = CARTESIAN_POINT ( 'NONE',  ( -19.69275026785852845, -21.90555837663575645, 65.60452853007984686 ) ) ;
#32531 = CARTESIAN_POINT ( 'NONE',  ( -23.33239146409005471, -10.27081399407338758, 59.74056881163177479 ) ) ;
#32532 = EDGE_LOOP ( 'NONE', ( #41259, #29423 ) ) ;
#32533 = CARTESIAN_POINT ( 'NONE',  ( -14.19282086353638661, -8.542981675383003903, 71.01485553001869278 ) ) ;
#32534 = ORIENTED_EDGE ( 'NONE', *, *, #18984, .T. ) ;
#32535 = CARTESIAN_POINT ( 'NONE',  ( -17.42409385541300892, -14.80920654474439679, 56.49999999999994316 ) ) ;
#32536 = FACE_OUTER_BOUND ( 'NONE', #19560, .T. ) ;
#32537 = CARTESIAN_POINT ( 'NONE',  ( -17.42847466931223011, -7.755496545676928477, 70.79035813383782738 ) ) ;
#32538 = VERTEX_POINT ( 'NONE', #17375 ) ;
#32539 = CARTESIAN_POINT ( 'NONE',  ( -24.14668021940793707, -18.02031455489962042, 59.12661512767745364 ) ) ;
#32540 = PLANE ( 'NONE',  #35960 ) ;
#32541 = EDGE_CURVE ( 'NONE', #9708, #23907, #40236, .T. ) ;
#32542 = CARTESIAN_POINT ( 'NONE',  ( -24.85884029783971982, -14.32113974155904046, 66.29637463883811677 ) ) ;
#32543 = CYLINDRICAL_SURFACE ( 'NONE', #11951, 2.000000000000001776 ) ;
#32544 = CARTESIAN_POINT ( 'NONE',  ( -19.21493033759332647, -8.042099214709203636, 59.97595409364182473 ) ) ;
#32545 = ORIENTED_EDGE ( 'NONE', *, *, #32584, .F. ) ;
#32546 = CARTESIAN_POINT ( 'NONE',  ( -16.92711826723489921, -22.24266155258999333, 72.35881524769365569 ) ) ;
#32547 = FACE_OUTER_BOUND ( 'NONE', #6399, .T. ) ;
#32548 = CARTESIAN_POINT ( 'NONE',  ( -22.98865756656685022, -9.855479763439479512, 70.12683098403445570 ) ) ;
#32549 = B_SPLINE_CURVE_WITH_KNOTS ( 'NONE', 3,
 ( #25688, #2795, #14334, #3033, #43950, #3778, #40243, #33796, #25941, #18535 ),
 .UNSPECIFIED., .F., .F.,
 ( 4, 2, 2, 2, 4 ),
 ( 0.6272669072977127280, 0.7522669073147477681, 0.8772669073317826971, 1.002266907348817737, 1.127266907365852777 ),
 .UNSPECIFIED. ) ;
#32550 = CARTESIAN_POINT ( 'NONE',  ( -24.22177711603362482, -13.13842781680106420, 62.83264177645653348 ) ) ;
#32551 = CARTESIAN_POINT ( 'NONE',  ( -14.31159385650551741, -6.922745924619793101, 51.69366785382590024 ) ) ;
#32552 = ORIENTED_EDGE ( 'NONE', *, *, #14895, .F. ) ;
#32553 = VERTEX_POINT ( 'NONE', #9044 ) ;
#32554 = CARTESIAN_POINT ( 'NONE',  ( 8.575906144586951996, -8.108449526715205025, 50.25000114615553315 ) ) ;
#32555 = ORIENTED_EDGE ( 'NONE', *, *, #32166, .F. ) ;
#32556 = CARTESIAN_POINT ( 'NONE',  ( -9.976686065099853451, -14.58608982656816622, 71.51437949254577120 ) ) ;
#32558 = CARTESIAN_POINT ( 'NONE',  ( -12.67164228717224361, -20.02160031757407310, 64.86674925084864185 ) ) ;
#32557 = CARTESIAN_POINT ( 'NONE',  ( -10.65090206719884591, -13.04127257218233460, 68.03832310965621843 ) ) ;
#32559 = CARTESIAN_POINT ( 'NONE',  ( -22.97409385650551528, -9.792211528768504536, 50.49490371617623197 ) ) ;
#32560 = CARTESIAN_POINT ( 'NONE',  ( -46.29409385541305966, -14.20920654474410760, 71.05212771298751306 ) ) ;
#32561 = FACE_OUTER_BOUND ( 'NONE', #42761, .T. ) ;
#32562 = CARTESIAN_POINT ( 'NONE',  ( -24.90891992605694227, -15.28604896337863472, 54.27966884056655061 ) ) ;
#32563 = FACE_BOUND ( 'NONE', #48233, .T. ) ;
#32564 = ADVANCED_FACE ( 'NONE', ( #13663 ), #46707, .F. ) ;
#32565 = CARTESIAN_POINT ( 'NONE',  ( -11.01266498513346015, -11.85818215851522339, 67.77431642774575948 ) ) ;
#32566 = FACE_OUTER_BOUND ( 'NONE', #20707, .T. ) ;
#32567 = AXIS2_PLACEMENT_3D ( 'NONE', #21550, #37261, #40485 ) ;
#32568 = CARTESIAN_POINT ( 'NONE',  ( -21.18398602608336745, -21.24092397535611809, 65.69958545398036165 ) ) ;
#32569 = VERTEX_POINT ( 'NONE', #32641 ) ;
#32570 = CIRCLE ( 'NONE', #35676, 5.249999999999998224 ) ;
#32571 = PLANE ( 'NONE',  #41601 ) ;
#32572 = PLANE ( 'NONE',  #7794 ) ;
#32573 = DIRECTION ( 'NONE',  ( 2.866981220435666553E-17, -1.000000000000000000, -1.190614954331866791E-16 ) ) ;
#32574 = CARTESIAN_POINT ( 'NONE',  ( -21.12013209665166258, -20.75402305920365720, 69.05450231649803072 ) ) ;
#32575 = CARTESIAN_POINT ( 'NONE',  ( -13.82689732469268407, -20.87277619789260186, 68.47097268802275494 ) ) ;
#32576 = CARTESIAN_POINT ( 'NONE',  ( -20.60788153932096023, -8.518722016582882972, 63.32593600985608617 ) ) ;
#32577 = VERTEX_POINT ( 'NONE', #25021 ) ;
#32578 = EDGE_LOOP ( 'NONE', ( #14229, #27408, #11499, #47286, #46499 ) ) ;
#32579 = CARTESIAN_POINT ( 'NONE',  ( -19.71159385541304232, -8.990409506049200417, 49.61344411288074951 ) ) ;
#32580 = EDGE_CURVE ( 'NONE', #42512, #40794, #47187, .T. ) ;
#32581 = CARTESIAN_POINT ( 'NONE',  ( -13.30711473254145716, -9.147892019113847084, 63.90946529584681457 ) ) ;
#32582 = ADVANCED_FACE ( 'NONE', ( #28711 ), #9279, .T. ) ;
#32583 = CARTESIAN_POINT ( 'NONE',  ( -23.98474789688958353, -17.25007084823549874, 69.71339792561613535 ) ) ;
#32584 = EDGE_CURVE ( 'NONE', #20093, #24954, #27977, .T. ) ;
#32585 = B_SPLINE_CURVE_WITH_KNOTS ( 'NONE', 1,
 ( #34446, #37654 ),
 .UNSPECIFIED., .F., .F.,
 ( 2, 2 ),
 ( 0.000000000000000000, 1.000000000000000000 ),
 .UNSPECIFIED. ) ;
#32586 = CARTESIAN_POINT ( 'NONE',  ( -20.70232273485035890, -8.624288160964143302, 60.14125250309182036 ) ) ;
#32587 = ORIENTED_EDGE ( 'NONE', *, *, #14353, .F. ) ;
#32588 = CARTESIAN_POINT ( 'NONE',  ( -11.34609264327665556, -11.23695660734646573, 60.97885752794695691 ) ) ;
#32589 = FACE_OUTER_BOUND ( 'NONE', #25733, .T. ) ;
#32590 = ORIENTED_EDGE ( 'NONE', *, *, #16333, .F. ) ;
#32591 =( BOUNDED_CURVE ( )  B_SPLINE_CURVE ( 3, ( #5736, #13568, #17016, #9425 ),
 .UNSPECIFIED., .F., .F. ) 
 B_SPLINE_CURVE_WITH_KNOTS ( ( 4, 4 ),
 ( 0.000000000000000000, 0.4074455897393696180 ),
 .UNSPECIFIED. ) 
 CURVE ( )  GEOMETRIC_REPRESENTATION_ITEM ( )  RATIONAL_B_SPLINE_CURVE ( ( 1.000000000000000000, 0.4567392136813241410, 0.3561768502900274358, 0.6983129098261098289 ) ) 
 REPRESENTATION_ITEM ( '' )  );
#32592 = CARTESIAN_POINT ( 'NONE',  ( -17.92211955501489484, -22.24259483734421750, 61.98261762376255746 ) ) ;
#32593 = EDGE_CURVE ( 'NONE', #33012, #4674, #24061, .T. ) ;
#32594 = DIRECTION ( 'NONE',  ( 0.9687793358424821033, -0.2479245821708679909, 0.000000000000000000 ) ) ;
#32595 = ADVANCED_FACE ( 'NONE', ( #1880 ), #39311, .F. ) ;
#32596 = AXIS2_PLACEMENT_3D ( 'NONE', #14660, #48189, #33389 ) ;
#32597 = EDGE_LOOP ( 'NONE', ( #17207, #24999, #43691, #8699, #43172 ) ) ;
#32598 = DIRECTION ( 'NONE',  ( 0.9930145540378111368, -0.1179919296777755949, -4.526730170392852178E-08 ) ) ;
#32599 = ADVANCED_FACE ( 'NONE', ( #28479 ), #5346, .F. ) ;
#32601 = EDGE_CURVE ( 'NONE', #20357, #36713, #36982, .T. ) ;
#32600 = VERTEX_POINT ( 'NONE', #31922 ) ;
#32602 = CARTESIAN_POINT ( 'NONE',  ( -11.96181431063714484, -19.87549516500596525, 58.11177798925346139 ) ) ;
#32603 = AXIS2_PLACEMENT_3D ( 'NONE', #23908, #6875, #36639 ) ;
#32604 = CARTESIAN_POINT ( 'NONE',  ( -24.00901317767524290, -17.32824147414624960, 69.42811846502259243 ) ) ;
#32605 = B_SPLINE_CURVE_WITH_KNOTS ( 'NONE', 3,
 ( #44484, #41763, #48648, #7307, #18595, #14888, #48401, #30203, #45224, #11466 ),
 .UNSPECIFIED., .F., .F.,
 ( 4, 2, 2, 2, 4 ),
 ( 0.6272669072877415930, 0.7522669073072615342, 0.8772669073267813644, 1.002266907346301306, 1.127266907365821247 ),
 .UNSPECIFIED. ) ;
#32606 = DIRECTION ( 'NONE',  ( 0.06357898915123476324, -0.9979768094191905359, 0.000000000000000000 ) ) ;
#32607 = CARTESIAN_POINT ( 'NONE',  ( -21.99213670719075253, -20.17946569659695655, 59.04970794435396897 ) ) ;
#32608 = ORIENTED_EDGE ( 'NONE', *, *, #38597, .T. ) ;
#32609 = DIRECTION ( 'NONE',  ( 0.9687793358424821033, -0.2479245821708679909, 0.000000000000000000 ) ) ;
#32611 =( BOUNDED_CURVE ( )  B_SPLINE_CURVE ( 3, ( #40737, #37514, #11431, #45429 ),
 .UNSPECIFIED., .F., .F. ) 
 B_SPLINE_CURVE_WITH_KNOTS ( ( 4, 4 ),
 ( 0.4074455897393594594, 0.5000000000000000000 ),
 .UNSPECIFIED. ) 
 CURVE ( )  GEOMETRIC_REPRESENTATION_ITEM ( )  RATIONAL_B_SPLINE_CURVE ( ( 0.6983129098260824064, 0.7760317562606884323, 0.8765941196519940748, 0.9999999999999990008 ) ) 
 REPRESENTATION_ITEM ( '' )  );
#32610 = CARTESIAN_POINT ( 'NONE',  ( -24.53826898343381302, -12.59737971884151975, 69.81597065678789704 ) ) ;
#32612 = FACE_OUTER_BOUND ( 'NONE', #21043, .T. ) ;
#32613 = CARTESIAN_POINT ( 'NONE',  ( -11.42962537269896117, -10.38539323336976494, 74.62380298385740218 ) ) ;
#32614 = CARTESIAN_POINT ( 'NONE',  ( -46.92409385541305511, -15.81020654474410847, 61.49999999999999289 ) ) ;
#32615 = FACE_OUTER_BOUND ( 'NONE', #25813, .T. ) ;
#32616 = ORIENTED_EDGE ( 'NONE', *, *, #20909, .T. ) ;
#32617 = CARTESIAN_POINT ( 'NONE',  ( -24.32646187101298807, -17.61277681157253738, 66.04382984432405124 ) ) ;
#32618 = CARTESIAN_POINT ( 'NONE',  ( -20.14428733920338743, -21.74485207141930587, 72.60467522768757931 ) ) ;
#32619 = CARTESIAN_POINT ( 'NONE',  ( -10.00693228073093977, -15.50849547184718880, 57.76066962513968406 ) ) ;
#32620 = ORIENTED_EDGE ( 'NONE', *, *, #9886, .F. ) ;
#32621 = DIRECTION ( 'NONE',  ( -7.484513356303811700E-07, 7.898531944235430371E-07, 0.9999999999994079181 ) ) ;
#32622 = ORIENTED_EDGE ( 'NONE', *, *, #33873, .T. ) ;
#32623 = ADVANCED_FACE ( 'NONE', ( #28228 ), #39551, .T. ) ;
#32624 = ORIENTED_EDGE ( 'NONE', *, *, #38199, .F. ) ;
#32625 = ORIENTED_EDGE ( 'NONE', *, *, #19264, .F. ) ;
#32626 = B_SPLINE_CURVE_WITH_KNOTS ( 'NONE', 1,
 ( #33950, #2155 ),
 .UNSPECIFIED., .F., .F.,
 ( 2, 2 ),
 ( 0.000000000000000000, 1.000000000000000000 ),
 .UNSPECIFIED. ) ;
#32627 = CARTESIAN_POINT ( 'NONE',  ( -10.03125382622086015, -15.73132242054001928, 61.21505925078393773 ) ) ;
#32628 = LINE ( 'NONE', #40991, #20089 ) ;
#32629 = B_SPLINE_CURVE_WITH_KNOTS ( 'NONE', 3,
 ( #29710, #37561, #25768, #33882, #26258, #45000, #38058, #41273, #4345, #15157 ),
 .UNSPECIFIED., .F., .F.,
 ( 4, 2, 2, 2, 4 ),
 ( 0.6272669072877971042, 0.7522669073073185997, 0.8772669073268399842, 1.002266907346361480, 1.127266907365882975 ),
 .UNSPECIFIED. ) ;
#32630 = CARTESIAN_POINT ( 'NONE',  ( -50.42409385541305511, -14.80920654474410547, 65.99999999999998579 ) ) ;
#32631 = ORIENTED_EDGE ( 'NONE', *, *, #4860, .F. ) ;
#32632 = EDGE_LOOP ( 'NONE', ( #9111, #7602, #8393, #6596, #32411 ) ) ;
#32633 = CIRCLE ( 'NONE', #31863, 1.999999999999998446 ) ;
#32634 = CARTESIAN_POINT ( 'NONE',  ( -17.43659385650551741, -6.915538690918075382, 49.31353937987644542 ) ) ;
#32635 = EDGE_CURVE ( 'NONE', #43582, #575, #43475, .T. ) ;
#32636 = AXIS2_PLACEMENT_3D ( 'NONE', #19642, #7847, #22867 ) ;
#32637 = CARTESIAN_POINT ( 'NONE',  ( 10.57590614458695377, 1.890747609047612521, 50.53028072113853142 ) ) ;
#32638 = CARTESIAN_POINT ( 'NONE',  ( -17.21159385650551599, -6.922745924619793101, 51.69366785382590024 ) ) ;
#32639 = B_SPLINE_CURVE_WITH_KNOTS ( 'NONE', 3,
 ( #36717, #33511, #48310, #14542, #25914, #25197, #26165, #45133, #40929, #3497 ),
 .UNSPECIFIED., .F., .F.,
 ( 4, 2, 2, 2, 4 ),
 ( 0.000000000000000000, 0.2500000000000000000, 0.5000000000000000000, 0.7500000000000000000, 1.000000000000000000 ),
 .UNSPECIFIED. ) ;
#32640 = ORIENTED_EDGE ( 'NONE', *, *, #32287, .T. ) ;
#32641 = CARTESIAN_POINT ( 'NONE',  ( -10.50893933415051507, -13.43540278197273885, 74.96345540680638919 ) ) ;
#32642 = DIRECTION ( 'NONE',  ( 0.000000000000000000, 0.000000000000000000, 1.000000000000000000 ) ) ;
#32643 = EDGE_LOOP ( 'NONE', ( #36360, #15175, #40230, #30799, #4416 ) ) ;
#32644 = CARTESIAN_POINT ( 'NONE',  ( -16.39156059917436181, -21.78318494029796781, 62.05568132351888266 ) ) ;
#32645 = EDGE_CURVE ( 'NONE', #6207, #36242, #42240, .T. ) ;
#32646 = ORIENTED_EDGE ( 'NONE', *, *, #15687, .T. ) ;
#32647 = CARTESIAN_POINT ( 'NONE',  ( -22.46950018977775088, -9.956826463545951356, 73.78161090405299660 ) ) ;
#32648 = CARTESIAN_POINT ( 'NONE',  ( -16.20683463515880973, -21.70255690700738782, 58.28585572422844052 ) ) ;
#32649 = EDGE_CURVE ( 'NONE', #27092, #46437, #24630, .T. ) ;
#32650 = EDGE_CURVE ( 'NONE', #43290, #16407, #17427, .T. ) ;
#32651 = CARTESIAN_POINT ( 'NONE',  ( -24.72409385541305582, -14.80920654474411613, 58.90588235294116970 ) ) ;
#32652 = ORIENTED_EDGE ( 'NONE', *, *, #16669, .F. ) ;
#32653 = CARTESIAN_POINT ( 'NONE',  ( -12.76547314785493192, -9.517330534081262172, 74.60450883341005124 ) ) ;
#32654 = CARTESIAN_POINT ( 'NONE',  ( -17.42409385541299471, -14.80920654474435771, 49.52966884056655772 ) ) ;
#32655 = CARTESIAN_POINT ( 'NONE',  ( -10.44104155427339364, -15.80511140325375763, 68.27768108067165542 ) ) ;
#32656 = ORIENTED_EDGE ( 'NONE', *, *, #21722, .T. ) ;
#32657 = CARTESIAN_POINT ( 'NONE',  ( -24.83340397596770543, -15.58795518843777472, 73.12490970255963418 ) ) ;
#32658 = DIRECTION ( 'NONE',  ( -0.5881408891789769999, -0.8087584895849666555, 7.565907428972491290E-08 ) ) ;
#32659 = ORIENTED_EDGE ( 'NONE', *, *, #10058, .T. ) ;
#32660 = AXIS2_PLACEMENT_3D ( 'NONE', #34076, #5031, #11680 ) ;
#32661 = CARTESIAN_POINT ( 'NONE',  ( -13.41658284876181995, -21.09041002232991957, 61.62990919978891924 ) ) ;
#32662 = ADVANCED_FACE ( 'NONE', ( #10489 ), #2835, .F. ) ;
#32663 = CARTESIAN_POINT ( 'NONE',  ( -24.22652117640109992, -16.69121458274543102, 59.26765574801870429 ) ) ;
#32664 = EDGE_LOOP ( 'NONE', ( #19427, #11190, #28856, #20028, #25964 ) ) ;
#32665 = CARTESIAN_POINT ( 'NONE',  ( -13.17178389636663027, -8.691783077619437137, 60.59983596220293833 ) ) ;
#32666 = CARTESIAN_POINT ( 'NONE',  ( -13.16256456194319391, -9.182988408105495992, 60.59517097614691039 ) ) ;
#32667 = DIRECTION ( 'NONE',  ( 1.224646799147353207E-16, 1.000000000000000000, -1.912410701131276611E-32 ) ) ;
#32668 = ORIENTED_EDGE ( 'NONE', *, *, #31414, .F. ) ;
#32669 = CARTESIAN_POINT ( 'NONE',  ( -10.47352315227043640, -13.96536545279488628, 61.10748405753005841 ) ) ;
#32670 = PRODUCT_DEFINITION_CONTEXT ( 'detailed design', #12094, 'design' ) ;
#32671 = CARTESIAN_POINT ( 'NONE',  ( -10.89357934009856521, -11.22367372050276302, 64.19236096111531253 ) ) ;
#32672 = CARTESIAN_POINT ( 'NONE',  ( -21.56595869292629075, -8.616614785013410938, 73.70790421061784059 ) ) ;
#32673 = EDGE_LOOP ( 'NONE', ( #3574, #24276, #31838, #33255, #7221 ) ) ;
#32674 = CARTESIAN_POINT ( 'NONE',  ( -10.18225258457650106, -13.06019941856358102, 71.31554448562532400 ) ) ;
#32675 = CARTESIAN_POINT ( 'NONE',  ( -24.66730423131801331, -13.06573828131289616, 62.94768895321241331 ) ) ;
#32676 = B_SPLINE_CURVE_WITH_KNOTS ( 'NONE', 3,
 ( #1242, #13280, #35460, #12816, #16248, #27600, #24648, #1746, #28336, #43361 ),
 .UNSPECIFIED., .F., .F.,
 ( 4, 2, 2, 2, 4 ),
 ( 0.000000000000000000, 0.2500000000000000000, 0.5000000000000000000, 0.7500000000000000000, 1.000000000000000000 ),
 .UNSPECIFIED. ) ;
#32677 = EDGE_CURVE ( 'NONE', #38392, #9477, #3412, .T. ) ;
#32678 = EDGE_LOOP ( 'NONE', ( #97, #27457, #6941, #29936, #5644, #44660, #13995, #47019 ) ) ;
#32679 = EDGE_LOOP ( 'NONE', ( #4192, #32503, #5249, #2521 ) ) ;
#32680 = CARTESIAN_POINT ( 'NONE',  ( -15.65722414396544870, -8.035737176819681693, 70.60989791501718571 ) ) ;
#32681 = FACE_OUTER_BOUND ( 'NONE', #37570, .T. ) ;
#32682 = DIRECTION ( 'NONE',  ( -3.071710424422018668E-17, 6.404604876783312462E-16, 1.000000000000000000 ) ) ;
#32683 = CARTESIAN_POINT ( 'NONE',  ( -12.62695865377714277, -19.98037072250615154, 71.89833714498439576 ) ) ;
#32684 = LINE ( 'NONE', #36598, #791 ) ;
#32685 = CARTESIAN_POINT ( 'NONE',  ( -12.30133590797630738, -20.21947593564565793, 68.52312695590214275 ) ) ;
#32686 = CARTESIAN_POINT ( 'NONE',  ( -20.50783594841701785, -8.027295835816985914, 66.96599399791791996 ) ) ;
#32687 = ORIENTED_EDGE ( 'NONE', *, *, #19282, .T. ) ;
#32688 = ORIENTED_EDGE ( 'NONE', *, *, #45240, .F. ) ;
#32689 = DIRECTION ( 'NONE',  ( -1.000000000000000000, -2.866981220435666553E-17, -0.000000000000000000 ) ) ;
#32690 = FACE_OUTER_BOUND ( 'NONE', #39222, .T. ) ;
#32691 = CARTESIAN_POINT ( 'NONE',  ( -11.46876066122178095, -18.48806595306161071, 61.57710833523393035 ) ) ;
#32692 = LINE ( 'NONE', #10055, #6363 ) ;
#32693 = CARTESIAN_POINT ( 'NONE',  ( -18.81159385650551741, -6.922745924619793101, 51.69366785382590024 ) ) ;
#32694 = VECTOR ( 'NONE', #14987, 1000.000000000000000 ) ;
#32695 = VERTEX_POINT ( 'NONE', #26227 ) ;
#32696 = CARTESIAN_POINT ( 'NONE',  ( -16.75420032499500422, -21.83093626061109305, 72.25723304517680390 ) ) ;
#32697 = CARTESIAN_POINT ( 'NONE',  ( -10.21985783787665802, -12.91125480557629146, 67.84494027641046898 ) ) ;
#32698 = LINE ( 'NONE', #13726, #44998 ) ;
#32699 = CARTESIAN_POINT ( 'NONE',  ( -10.03860189133040315, -15.79316336790978603, 61.15133701675058120 ) ) ;
#32700 = ORIENTED_EDGE ( 'NONE', *, *, #47944, .F. ) ;
#32701 = CARTESIAN_POINT ( 'NONE',  ( -13.53325528467554406, -21.16256411608339150, 65.17124155742401115 ) ) ;
#32702 = CARTESIAN_POINT ( 'NONE',  ( -16.91855014848012928, -22.24212009645463439, 72.28047803099305213 ) ) ;
#32703 = EDGE_CURVE ( 'NONE', #29981, #26502, #11709, .T. ) ;
#32704 = CARTESIAN_POINT ( 'NONE',  ( -15.49330550865652079, -21.58970246877112587, 72.34575444675695621 ) ) ;
#32705 = LINE ( 'NONE', #17451, #44842 ) ;
#32706 = EDGE_LOOP ( 'NONE', ( #14644, #20702, #12137, #21825, #5416, #22489, #14970, #34290 ) ) ;
#32707 = CYLINDRICAL_SURFACE ( 'NONE', #21240, 2.000000000000003109 ) ;
#32708 = ORIENTED_EDGE ( 'NONE', *, *, #35484, .T. ) ;
#32709 = DIRECTION ( 'NONE',  ( -3.071710424422018668E-17, 6.404604876783312462E-16, 1.000000000000000000 ) ) ;
#32710 = EDGE_CURVE ( 'NONE', #39007, #19712, #15061, .T. ) ;
#32711 = EDGE_CURVE ( 'NONE', #13315, #29603, #37045, .T. ) ;
#32712 = CARTESIAN_POINT ( 'NONE',  ( -10.23791430846135597, -12.84371669600496801, 67.91645119285166743 ) ) ;
#32713 = EDGE_LOOP ( 'NONE', ( #8192, #26967 ) ) ;
#32714 = CARTESIAN_POINT ( 'NONE',  ( -13.67008536917650119, -21.24427532949667707, 68.55650896281578355 ) ) ;
#32715 = EDGE_CURVE ( 'NONE', #7043, #22471, #28588, .T. ) ;
#32716 = EDGE_LOOP ( 'NONE', ( #11877, #40999, #16279, #45915, #23945 ) ) ;
#32717 = CARTESIAN_POINT ( 'NONE',  ( -21.00733138479494855, -11.77013360165371836, 52.02966884056656482 ) ) ;
#32718 = EDGE_CURVE ( 'NONE', #45155, #17452, #42616, .T. ) ;
#32719 =( BOUNDED_SURFACE ( )  B_SPLINE_SURFACE ( 1, 2, ( 
 ( #31675, #45970, #42764, #39299, #5093, #9268, #12230, #4602, #34631, #5585, #16144, #43251, #20102, #27250, #46696, #38566, #8541, #24295, #12466, #23815, #8797, #20598, #12715, #914, #46930, #24052, #23318, #4854, #1872, #30956, #19873, #12943, #13172, #34870, #28219, #9034, #31187, #27969, #1376, #46209, #38311, #35596, #27491, #39047, #38815, #31424, #42994, #5335, #20350, #46461, #35359, #16641, #16872, #6045, #35830, #47656, #14128, #9760, #29424, #39780, #24545, #2113, #47900, #10482, #28939, #13896, #17365, #39541, #43736, #28472, #17112, #9988, #21075, #40275, #9520, #10242, #36315, #36782, #13424, #36543, #36074, #21565, #2828, #25011, #2354, #2602, #40034, #40501, #32162, #5821, #47177, #43496, #43985, #6296, #24779, #47426, #32407, #17600, #13656, #17834, #28699, #21327, #32634, #20833, #25257, #6541, #21788, #32859, #29188, #44230, #6777, #25484, #3071, #18078, #33090, #48139, #14370, #26465, #136, #29670, #41729, #37275, #4307, #15118, #26714, #48372, #7026, #18832, #7771, #3563, #45435, #10960, #44957, #45197, #11689, #18568, #30177, #7522, #3818, #37780, #33576, #44705, #4076, #25978, #10711, #8020, #11437, #22525, #23032, #38017, #41478, #19072, #19314, #34320, #15606, #29921, #25726, #604, #7280, #41234, #22281, #22043, #22786, #37520, #48624, #37037, #3321, #14606, #18324, #33838, #44456, #14858, #40744, #34082, #33332, #372, #15357, #30418, #41000, #11211, #26222 ),
 ( #1318, #42216, #31625, #12173, #27433, #12892, #38510, #45683, #16329, #1572, #30901, #12656, #8737, #11940, #30665, #31372, #26957, #8480, #41977, #38252, #8248, #38997, #23266, #19561, #5525, #5277, #4534, #35055, #46646, #20545, #34570, #27917, #15854, #854, #16580, #45916, #27192, #35545, #20047, #23510, #4791, #42941, #42466, #8975, #1088, #19818, #23764, #38756, #27680, #34816, #1819, #16088, #31127, #9215, #46150, #42713, #12409, #5037, #24238, #46400, #23996, #20292, #35299, #39246, #35777, #9939, #32579, #40221, #2301, #32810, #13119, #39729, #24955, #29129, #2552, #28651, #44180, #10430, #13842, #25203, #25439, #40448, #36725, #17307, #46879, #6723, #28415, #13605, #43439, #28163, #17551, #43683, #24726, #9462, #43192, #20777, #24486, #39974, #14078, #5995, #16818, #28885, #39491, #6248, #36494, #21269, #2058, #47610, #17058, #36265, #21739, #31858, #43928, #10188, #6490, #21512, #9709, #17785, #47123, #2775, #47840, #21020, #5770, #32102, #13367, #36017, #32356, #47375, #33041, #3013, #3756, #18024, #29614, #48085, #10660, #14321, #11384, #29372, #40685, #26653, #26407, #25669, #7470, #19019, #41671, #44404, #4011, #36978, #6965, #37720, #21984, #33276, #7959, #41182, #18271, #3268, #34025, #14796, #30118, #22228, #48316, #29865, #11150, #71, #14549, #22974, #37219, #44643, #15297, #10900, #15060, #40936, #25924, #315, #3503, #45142, #18515, #33520, #7222, #48566, #44899 ) ),
 .UNSPECIFIED., .F., .F., .F. ) 
 B_SPLINE_SURFACE_WITH_KNOTS ( ( 2, 2 ),
 ( 3, 2, 2, 2, 2, 2, 2, 2, 2, 2, 2, 2, 2, 2, 2, 2, 2, 2, 2, 2, 2, 2, 2, 2, 2, 2, 2, 2, 2, 2, 2, 2, 2, 2, 2, 2, 2, 2, 2, 2, 2, 2, 2, 2, 2, 2, 2, 2, 2, 2, 2, 2, 2, 2, 2, 2, 2, 2, 2, 2, 2, 2, 2, 2, 2, 2, 2, 2, 2, 2, 2, 2, 2, 2, 2, 2, 2, 2, 2, 2, 2, 2, 2, 2, 2, 2, 2, 2, 2, 2, 3 ),
 ( 0.000000000000000000, 1.000000000000000000 ),
 ( 0.000000000000000000, 0.01041666666666666609, 0.02083333333333333218, 0.03125000000000000000, 0.04166666666666666435, 0.05208333333333333565, 0.06250000000000000000, 0.07291666666666667129, 0.08333333333333332871, 0.09375000000000000000, 0.1041666666666666713, 0.1145833333333333287, 0.1250000000000000000, 0.1354166666666666574, 0.1458333333333333426, 0.1562500000000000000, 0.1666666666666666574, 0.1770833333333333426, 0.1875000000000000000, 0.1979166666666666574, 0.2083333333333333426, 0.2187500000000000000, 0.2291666666666666574, 0.2395833333333333426, 0.2500000000000000000, 0.2604166666666666852, 0.2708333333333333148, 0.2812500000000000000, 0.2916666666666666852, 0.3020833333333333148, 0.3125000000000000000, 0.3229166666666666852, 0.3333333333333333148, 0.3437500000000000000, 0.3541666666666666852, 0.3645833333333333148, 0.3750000000000000000, 0.3854166666666666852, 0.3958333333333333148, 0.4062500000000000000, 0.4166666666666666852, 0.4270833333333333148, 0.4375000000000000000, 0.4479166666666666852, 0.4583333333333333148, 0.4687500000000000000, 0.4791666666666666852, 0.4895833333333333148, 0.5000000000000000000, 0.5104166666666666297, 0.5208333333333333703, 0.5312500000000000000, 0.5416666666666666297, 0.5520833333333333703, 0.5625000000000000000, 0.5729166666666666297, 0.5833333333333333703, 0.5937500000000000000, 0.6041666666666666297, 0.6145833333333333703, 0.6250000000000000000, 0.6354166666666666297, 0.6458333333333333703, 0.6562500000000000000, 0.6666666666666666297, 0.6770833333333333703, 0.6875000000000000000, 0.6979166666666666297, 0.7083333333333333703, 0.7187500000000000000, 0.7291666666666666297, 0.7395833333333333703, 0.7500000000000000000, 0.7604166666666666297, 0.7708333333333333703, 0.7812500000000000000, 0.7916666666666666297, 0.8020833333333333703, 0.8125000000000000000, 0.8229166666666666297, 0.8333333333333333703, 0.8437500000000000000, 0.8541666666666666297, 0.8645833333333333703, 0.8750000000000000000, 0.8854166666666666297, 0.8958333333333333703, 0.9062500000000000000, 0.9166666666666666297, 0.9259048894201962199, 0.9351639383143981465 ),
 .UNSPECIFIED. ) 
 GEOMETRIC_REPRESENTATION_ITEM ( )  RATIONAL_B_SPLINE_SURFACE ( (
 ( 1.000000000000000000, 0.9238795325112867385, 1.000000000000000000, 0.9238795325112867385, 1.000000000000000000, 0.9238795325112867385, 1.000000000000000000, 0.9238795325112867385, 1.000000000000000000, 0.9238795325112867385, 1.000000000000000000, 0.9238795325112867385, 1.000000000000000000, 0.9238795325112867385, 1.000000000000000000, 0.9238795325112867385, 1.000000000000000000, 0.9238795325112867385, 1.000000000000000000, 0.9238795325112867385, 1.000000000000000000, 0.9238795325112867385, 1.000000000000000000, 0.9238795325112867385, 1.000000000000000000, 0.9238795325112867385, 1.000000000000000000, 0.9238795325112867385, 1.000000000000000000, 0.9238795325112867385, 1.000000000000000000, 0.9238795325112867385, 1.000000000000000000, 0.9238795325112867385, 1.000000000000000000, 0.9238795325112867385, 1.000000000000000000, 0.9238795325112867385, 1.000000000000000000, 0.9238795325112867385, 1.000000000000000000, 0.9238795325112867385, 1.000000000000000000, 0.9238795325112867385, 1.000000000000000000, 0.9238795325112867385, 1.000000000000000000, 0.9238795325112867385, 1.000000000000000000, 0.9238795325112867385, 1.000000000000000000, 0.9238795325112867385, 1.000000000000000000, 0.9238795325112867385, 1.000000000000000000, 0.9238795325112867385, 1.000000000000000000, 0.9238795325112867385, 1.000000000000000000, 0.9238795325112867385, 1.000000000000000000, 0.9238795325112867385, 1.000000000000000000, 0.9238795325112867385, 1.000000000000000000, 0.9238795325112867385, 1.000000000000000000, 0.9238795325112867385, 1.000000000000000000, 0.9238795325112867385, 1.000000000000000000, 0.9238795325112867385, 1.000000000000000000, 0.9238795325112867385, 1.000000000000000000, 0.9238795325112867385, 1.000000000000000000, 0.9238795325112867385, 1.000000000000000000, 0.9238795325112867385, 1.000000000000000000, 0.9238795325112867385, 1.000000000000000000, 0.9238795325112867385, 1.000000000000000000, 0.9238795325112867385, 1.000000000000000000, 0.9238795325112867385, 1.000000000000000000, 0.9238795325112867385, 1.000000000000000000, 0.9238795325112867385, 1.000000000000000000, 0.9238795325112867385, 1.000000000000000000, 0.9238795325112867385, 1.000000000000000000, 0.9238795325112867385, 1.000000000000000000, 0.9238795325112867385, 1.000000000000000000, 0.9238795325112867385, 1.000000000000000000, 0.9238795325112867385, 1.000000000000000000, 0.9238795325112867385, 1.000000000000000000, 0.9238795325112867385, 1.000000000000000000, 0.9238795325112867385, 1.000000000000000000, 0.9238795325112867385, 1.000000000000000000, 0.9238795325112867385, 1.000000000000000000, 0.9238795325112867385, 1.000000000000000000, 0.9238795325112867385, 1.000000000000000000, 0.9238795325112867385, 1.000000000000000000, 0.9238795325112867385, 1.000000000000000000, 0.9238795325112867385, 1.000000000000000000, 0.9238795325112867385, 1.000000000000000000, 0.9238795325112867385, 1.000000000000000000, 0.9238795325112867385, 1.000000000000000000, 0.9238795325112867385, 1.000000000000000000, 0.9238795325112867385, 1.000000000000000000, 0.9238795325112867385, 1.000000000000000000, 0.9238795325112867385, 1.000000000000000000, 0.9238795325112867385, 1.000000000000000000, 0.9238795325112867385, 1.000000000000000000, 0.9238795325112867385, 1.000000000000000000, 0.9238795325112867385, 1.000000000000000000, 0.9238795325112867385, 1.000000000000000000, 0.9238795325112867385, 1.000000000000000000, 0.9238795325112867385, 1.000000000000000000, 0.9238795325112867385, 1.000000000000000000, 0.9238795325112867385, 1.000000000000000000, 0.9238795325112867385, 1.000000000000000000, 0.9238795325112867385, 1.000000000000000000, 0.9238795325112867385, 1.000000000000000000, 0.9238795325112867385, 1.000000000000000000, 0.9238795325112867385, 1.000000000000000000, 0.9238795325112867385, 1.000000000000000000, 0.9238795325112867385, 1.000000000000000000, 0.9238795325112867385, 1.000000000000000000, 0.9238795325112867385, 1.000000000000000000, 0.9238795325112867385, 1.000000000000000000, 0.9324910878627006294, 0.9847253504145836445, 0.9847253504145836445, 0.9847253504145836445),
 ( 1.000000000000000000, 0.9238795325112867385, 1.000000000000000000, 0.9238795325112867385, 1.000000000000000000, 0.9238795325112867385, 1.000000000000000000, 0.9238795325112867385, 1.000000000000000000, 0.9238795325112867385, 1.000000000000000000, 0.9238795325112867385, 1.000000000000000000, 0.9238795325112867385, 1.000000000000000000, 0.9238795325112867385, 1.000000000000000000, 0.9238795325112867385, 1.000000000000000000, 0.9238795325112867385, 1.000000000000000000, 0.9238795325112867385, 1.000000000000000000, 0.9238795325112867385, 1.000000000000000000, 0.9238795325112867385, 1.000000000000000000, 0.9238795325112867385, 1.000000000000000000, 0.9238795325112867385, 1.000000000000000000, 0.9238795325112867385, 1.000000000000000000, 0.9238795325112867385, 1.000000000000000000, 0.9238795325112867385, 1.000000000000000000, 0.9238795325112867385, 1.000000000000000000, 0.9238795325112867385, 1.000000000000000000, 0.9238795325112867385, 1.000000000000000000, 0.9238795325112867385, 1.000000000000000000, 0.9238795325112867385, 1.000000000000000000, 0.9238795325112867385, 1.000000000000000000, 0.9238795325112867385, 1.000000000000000000, 0.9238795325112867385, 1.000000000000000000, 0.9238795325112867385, 1.000000000000000000, 0.9238795325112867385, 1.000000000000000000, 0.9238795325112867385, 1.000000000000000000, 0.9238795325112867385, 1.000000000000000000, 0.9238795325112867385, 1.000000000000000000, 0.9238795325112867385, 1.000000000000000000, 0.9238795325112867385, 1.000000000000000000, 0.9238795325112867385, 1.000000000000000000, 0.9238795325112867385, 1.000000000000000000, 0.9238795325112867385, 1.000000000000000000, 0.9238795325112867385, 1.000000000000000000, 0.9238795325112867385, 1.000000000000000000, 0.9238795325112867385, 1.000000000000000000, 0.9238795325112867385, 1.000000000000000000, 0.9238795325112867385, 1.000000000000000000, 0.9238795325112867385, 1.000000000000000000, 0.9238795325112867385, 1.000000000000000000, 0.9238795325112867385, 1.000000000000000000, 0.9238795325112867385, 1.000000000000000000, 0.9238795325112867385, 1.000000000000000000, 0.9238795325112867385, 1.000000000000000000, 0.9238795325112867385, 1.000000000000000000, 0.9238795325112867385, 1.000000000000000000, 0.9238795325112867385, 1.000000000000000000, 0.9238795325112867385, 1.000000000000000000, 0.9238795325112867385, 1.000000000000000000, 0.9238795325112867385, 1.000000000000000000, 0.9238795325112867385, 1.000000000000000000, 0.9238795325112867385, 1.000000000000000000, 0.9238795325112867385, 1.000000000000000000, 0.9238795325112867385, 1.000000000000000000, 0.9238795325112867385, 1.000000000000000000, 0.9238795325112867385, 1.000000000000000000, 0.9238795325112867385, 1.000000000000000000, 0.9238795325112867385, 1.000000000000000000, 0.9238795325112867385, 1.000000000000000000, 0.9238795325112867385, 1.000000000000000000, 0.9238795325112867385, 1.000000000000000000, 0.9238795325112867385, 1.000000000000000000, 0.9238795325112867385, 1.000000000000000000, 0.9238795325112867385, 1.000000000000000000, 0.9238795325112867385, 1.000000000000000000, 0.9238795325112867385, 1.000000000000000000, 0.9238795325112867385, 1.000000000000000000, 0.9238795325112867385, 1.000000000000000000, 0.9238795325112867385, 1.000000000000000000, 0.9238795325112867385, 1.000000000000000000, 0.9238795325112867385, 1.000000000000000000, 0.9238795325112867385, 1.000000000000000000, 0.9238795325112867385, 1.000000000000000000, 0.9238795325112867385, 1.000000000000000000, 0.9238795325112867385, 1.000000000000000000, 0.9238795325112867385, 1.000000000000000000, 0.9238795325112867385, 1.000000000000000000, 0.9238795325112867385, 1.000000000000000000, 0.9238795325112867385, 1.000000000000000000, 0.9238795325112867385, 1.000000000000000000, 0.9238795325112867385, 1.000000000000000000, 0.9238795325112867385, 1.000000000000000000, 0.9238795325112867385, 1.000000000000000000, 0.9238795325112867385, 1.000000000000000000, 0.9238795325112867385, 1.000000000000000000, 0.9324910878627006294, 0.9847253504145836445, 0.9847253504145836445, 0.9847253504145836445) ) ) 
 REPRESENTATION_ITEM ( '' )  SURFACE ( )  );
#32720 = CARTESIAN_POINT ( 'NONE',  ( -7.924093855413070209, -6.359206544744109735, 52.99999999999997868 ) ) ;
#32721 = CARTESIAN_POINT ( 'NONE',  ( -23.52949419687348964, -11.28347464189849703, 70.17738639980606763 ) ) ;
#32722 = ORIENTED_EDGE ( 'NONE', *, *, #22426, .T. ) ;
#32723 = CARTESIAN_POINT ( 'NONE',  ( -13.46043688762014412, -21.11748779262230258, 65.14775429738139678 ) ) ;
#32724 = AXIS2_PLACEMENT_3D ( 'NONE', #35385, #6324, #21106 ) ;
#32725 = CARTESIAN_POINT ( 'NONE',  ( -17.53499440593470737, -7.752105970505813737, 70.63468544436783247 ) ) ;
#32726 = VECTOR ( 'NONE', #8612, 1000.000000000000000 ) ;
#32727 = CARTESIAN_POINT ( 'NONE',  ( -11.36243649338991091, -11.30818272981683137, 60.96420372599168758 ) ) ;
#32728 = CARTESIAN_POINT ( 'NONE',  ( -23.23616516995063819, -18.79948553760870666, 65.97389430042666447 ) ) ;
#32729 = EDGE_CURVE ( 'NONE', #27273, #6531, #44967, .T. ) ;
#32730 = VERTEX_POINT ( 'NONE', #15127 ) ;
#32731 = ORIENTED_EDGE ( 'NONE', *, *, #40384, .T. ) ;
#32732 = FACE_OUTER_BOUND ( 'NONE', #20765, .T. ) ;
#32733 = CARTESIAN_POINT ( 'NONE',  ( -24.31477923169101629, -16.30090137217950641, 59.40860294853779777 ) ) ;
#32734 = VERTEX_POINT ( 'NONE', #11218 ) ;
#32735 = CARTESIAN_POINT ( 'NONE',  ( -23.81337036566721466, -17.78917542641211469, 59.30378412513616126 ) ) ;
#32736 = CARTESIAN_POINT ( 'NONE',  ( -20.08034385759798823, -9.360768649639302552, 51.01397948905922419 ) ) ;
#32737 = CARTESIAN_POINT ( 'NONE',  ( -23.65513889391139557, -11.50482878637529716, 62.83729622335476961 ) ) ;
#32738 = CARTESIAN_POINT ( 'NONE',  ( -16.86517901922215756, -21.78691905967089326, 68.98095278456760582 ) ) ;
#32739 = CARTESIAN_POINT ( 'NONE',  ( -15.36003256934816719, -8.059790721335600594, 70.76556701434653007 ) ) ;
#32740 =( BOUNDED_CURVE ( )  B_SPLINE_CURVE ( 3, ( #28198, #16369, #1352, #20079 ),
 .UNSPECIFIED., .F., .F. ) 
 B_SPLINE_CURVE_WITH_KNOTS ( ( 4, 4 ),
 ( 0.000000000000000000, 0.4074455897393645665 ),
 .UNSPECIFIED. ) 
 CURVE ( )  GEOMETRIC_REPRESENTATION_ITEM ( )  RATIONAL_B_SPLINE_CURVE ( ( 1.000000000000000000, 0.4567392136813283599, 0.3561768502900289901, 0.6983129098261017242 ) ) 
 REPRESENTATION_ITEM ( '' )  );
#32741 = DIRECTION ( 'NONE',  ( 0.9687793358424821033, -0.2479245821708677133, 0.000000000000000000 ) ) ;
#32742 = ORIENTED_EDGE ( 'NONE', *, *, #7295, .T. ) ;
#32743 = CARTESIAN_POINT ( 'NONE',  ( -10.55572857713978685, -13.45776460179270373, 74.69320064931967806 ) ) ;
#32744 = CARTESIAN_POINT ( 'NONE',  ( -10.80649751745619724, -11.38720838924848522, 67.71840977816552254 ) ) ;
#32745 = VERTEX_POINT ( 'NONE', #18574 ) ;
#32746 =( BOUNDED_CURVE ( )  B_SPLINE_CURVE ( 3, ( #41009, #29930, #33589, #37048 ),
 .UNSPECIFIED., .F., .F. ) 
 B_SPLINE_CURVE_WITH_KNOTS ( ( 4, 4 ),
 ( 0.9074455897393652881, 1.000000000000000000 ),
 .UNSPECIFIED. ) 
 CURVE ( )  GEOMETRIC_REPRESENTATION_ITEM ( )  RATIONAL_B_SPLINE_CURVE ( ( 0.6983129098260870693, 0.7760317562606930952, 0.8765941196519974055, 1.000000000000000000 ) ) 
 REPRESENTATION_ITEM ( '' )  );
#32747 = B_SPLINE_CURVE_WITH_KNOTS ( 'NONE', 3,
 ( #18896, #48684, #14928, #33909, #15177, #30240, #45259, #11502, #39301, #13173 ),
 .UNSPECIFIED., .F., .F.,
 ( 4, 2, 2, 2, 4 ),
 ( 0.1272669073658319605, 0.2522669073463114642, 0.3772669073267909123, 0.5022669073072704160, 0.6272669072877499197 ),
 .UNSPECIFIED. ) ;
#32748 = VERTEX_POINT ( 'NONE', #29679 ) ;
#32749 = CARTESIAN_POINT ( 'NONE',  ( -10.83536385990051798, -17.31742045656482176, 64.77739380450887552 ) ) ;
#32750 = CARTESIAN_POINT ( 'NONE',  ( -10.00591001363343580, -14.11961505468812206, 61.05674763264026694 ) ) ;
#32751 = CARTESIAN_POINT ( 'NONE',  ( -22.41759978862804914, -13.18828134753566417, 50.77966884056655772 ) ) ;
#32752 = EDGE_CURVE ( 'NONE', #19668, #33183, #29195, .T. ) ;
#32753 = VERTEX_POINT ( 'NONE', #10966 ) ;
#32754 = CARTESIAN_POINT ( 'NONE',  ( -24.23612025527544134, -13.19763772753531406, 59.58941156045592180 ) ) ;
#32755 = AXIS2_PLACEMENT_3D ( 'NONE', #41363, #44839, #26852 ) ;
#32756 = CARTESIAN_POINT ( 'NONE',  ( -23.81448002858924795, -17.66644687436950178, 59.23051795168259304 ) ) ;
#32757 = ADVANCED_FACE ( 'NONE', ( #25493 ), #25991, .T. ) ;
#32758 = ORIENTED_EDGE ( 'NONE', *, *, #47124, .T. ) ;
#32759 = LINE ( 'NONE', #30067, #8668 ) ;
#32760 = VECTOR ( 'NONE', #47437, 1000.000000000000000 ) ;
#32761 = CARTESIAN_POINT ( 'NONE',  ( -17.91839958824308709, -21.79173199888728263, 61.87535923606637311 ) ) ;
#32762 = VERTEX_POINT ( 'NONE', #29432 ) ;
#32763 = CARTESIAN_POINT ( 'NONE',  ( -15.03744282974918178, -5.447548802137111679, 54.49999999999995026 ) ) ;
#32764 = ORIENTED_EDGE ( 'NONE', *, *, #33889, .F. ) ;
#32765 = CARTESIAN_POINT ( 'NONE',  ( -17.00410561000564513, -7.771727611841390271, 74.26018273220859101 ) ) ;
#32766 = CARTESIAN_POINT ( 'NONE',  ( -22.65953014494242979, -19.53520302830625965, 72.52911954723420251 ) ) ;
#32767 = CARTESIAN_POINT ( 'NONE',  ( -23.67763357919828948, -11.55377495691942791, 66.42774300827811373 ) ) ;
#32768 = ORIENTED_EDGE ( 'NONE', *, *, #45192, .F. ) ;
#32769 = CARTESIAN_POINT ( 'NONE',  ( -22.53429319464570924, -9.952421322533329118, 73.48161091678163359 ) ) ;
#32770 = CARTESIAN_POINT ( 'NONE',  ( -10.48201079127635715, -16.05857626038448061, 64.71591366516646815 ) ) ;
#32771 = EDGE_CURVE ( 'NONE', #42667, #31657, #3389, .T. ) ;
#32772 = CARTESIAN_POINT ( 'NONE',  ( -22.94909385650551314, -8.104110260919577868, 48.81699501597546487 ) ) ;
#32773 = ADVANCED_FACE ( 'NONE', ( #18838 ), #38936, .T. ) ;
#32774 = CARTESIAN_POINT ( 'NONE',  ( -10.05737394094114912, -15.92036584257266263, 64.61433266094377359 ) ) ;
#32775 = PLANE ( 'NONE',  #29231 ) ;
#32776 = CARTESIAN_POINT ( 'NONE',  ( -12.38697808428427827, -19.74705103147751117, 57.92682335111648939 ) ) ;
#32777 = ORIENTED_EDGE ( 'NONE', *, *, #28274, .F. ) ;
#32778 = CARTESIAN_POINT ( 'NONE',  ( -24.87089661258515960, -14.58528678170222470, 62.87329882295441763 ) ) ;
#32779 = DIRECTION ( 'NONE',  ( 0.9466432954593471116, 0.3222832157619555660, 8.771047036255756069E-09 ) ) ;
#32780 = CARTESIAN_POINT ( 'NONE',  ( -22.69651743546460665, -20.07290662366753864, 69.31271507414059840 ) ) ;
#32781 = CARTESIAN_POINT ( 'NONE',  ( -13.29979614553676370, -21.01354653661592664, 61.77292273241334186 ) ) ;
#32782 = EDGE_CURVE ( 'NONE', #5852, #486, #39266, .T. ) ;
#32783 = CARTESIAN_POINT ( 'NONE',  ( -18.58465539680892320, -7.906023667314016734, 70.44355971113242276 ) ) ;
#32784 = ORIENTED_EDGE ( 'NONE', *, *, #14006, .F. ) ;
#32785 = ORIENTED_EDGE ( 'NONE', *, *, #92, .T. ) ;
#32786 = CARTESIAN_POINT ( 'NONE',  ( -22.75923595801102550, -10.27751167601812909, 66.54182257657851096 ) ) ;
#32787 = CARTESIAN_POINT ( 'NONE',  ( -45.55409385541305767, -14.20920654474410760, 70.08498674719956512 ) ) ;
#32788 = EDGE_LOOP ( 'NONE', ( #40316, #16734, #44199, #31681 ) ) ;
#32790 = CARTESIAN_POINT ( 'NONE',  ( -14.11063322135152909, -21.03236308526469855, 72.21135587486895702 ) ) ;
#32789 = LINE ( 'NONE', #6942, #25864 ) ;
#32791 = DIRECTION ( 'NONE',  ( 0.1240347345892083841, 0.000000000000000000, 0.9922778767136676281 ) ) ;
#32792 = DIRECTION ( 'NONE',  ( -0.6562885720885138774, 0.7545099801500438907, 1.193821363054685294E-08 ) ) ;
#32793 = CARTESIAN_POINT ( 'NONE',  ( -12.13424045023392139, -19.48172391048287011, 61.54111352175390692 ) ) ;
#32794 = ADVANCED_FACE ( 'NONE', ( #30911 ), #8029, .T. ) ;
#32795 = DIRECTION ( 'NONE',  ( 0.8960627639203804229, -0.4439273849576848563, 1.473420430759783058E-16 ) ) ;
#32796 = FACE_BOUND ( 'NONE', #6082, .T. ) ;
#32797 = DIRECTION ( 'NONE',  ( 0.9710973231077276724, -0.2386838684389877008, 7.431671637556431570E-08 ) ) ;
#32798 = AXIS2_PLACEMENT_3D ( 'NONE', #9695, #23984, #36007 ) ;
#32799 = DIRECTION ( 'NONE',  ( 0.8244078399817416081, 0.5659962132175737626, 7.627400655798536990E-08 ) ) ;
#32800 = VERTEX_POINT ( 'NONE', #46157 ) ;
#32801 = CARTESIAN_POINT ( 'NONE',  ( -7.424093855413048892, -27.10920654474410796, 77.00000000000000000 ) ) ;
#32802 = CARTESIAN_POINT ( 'NONE',  ( -11.60006209888454443, -10.16330164164447325, 71.08397698276321819 ) ) ;
#32803 = CIRCLE ( 'NONE', #24176, 2.000000000000000888 ) ;
#32804 = DIRECTION ( 'NONE',  ( -0.8447509909909771686, 0.5351595679979589404, 0.000000000000000000 ) ) ;
#32805 = CARTESIAN_POINT ( 'NONE',  ( -20.80646516979311755, -21.44732190390276472, 58.78441795439189121 ) ) ;
#32806 = CARTESIAN_POINT ( 'NONE',  ( -14.46752719259218622, -19.14754880513559954, 50.77966884056656482 ) ) ;
#32807 = CARTESIAN_POINT ( 'NONE',  ( -11.50273385864769438, -11.07591097799543256, 57.50903212538073461 ) ) ;
#32808 = VERTEX_POINT ( 'NONE', #11447 ) ;
#32809 = ORIENTED_EDGE ( 'NONE', *, *, #22694, .F. ) ;
#32810 = CARTESIAN_POINT ( 'NONE',  ( -19.54284385541304303, -7.587656875400192291, 49.25157356644813689 ) ) ;
#32811 = VERTEX_POINT ( 'NONE', #34821 ) ;
#32812 = DIRECTION ( 'NONE',  ( -0.000000000000000000, -1.000000000000000000, -0.000000000000000000 ) ) ;
#32813 = CARTESIAN_POINT ( 'NONE',  ( -18.98390459359973548, -7.933620001262258192, 66.91543923465638954 ) ) ;
#32814 = EDGE_CURVE ( 'NONE', #26255, #12784, #19294, .T. ) ;
#32815 = CARTESIAN_POINT ( 'NONE',  ( -20.19284385759799605, -8.630756214087126565, 51.74842643355248129 ) ) ;
#32816 = CARTESIAN_POINT ( 'NONE',  ( -9.973358241295501969, -14.79494948476079941, 74.98434255746357735 ) ) ;
#32817 = VERTEX_POINT ( 'NONE', #12419 ) ;
#32818 = CARTESIAN_POINT ( 'NONE',  ( -11.03230881600246427, -10.98182333549695322, 60.79390388117851529 ) ) ;
#32819 = DIRECTION ( 'NONE',  ( 3.071710424422018668E-17, -6.404604876783312462E-16, -1.000000000000000000 ) ) ;
#32820 = ORIENTED_EDGE ( 'NONE', *, *, #48332, .T. ) ;
#32821 = CARTESIAN_POINT ( 'NONE',  ( -24.41887989065141795, -14.52796127067242971, 66.46676134466591179 ) ) ;
#32822 = CARTESIAN_POINT ( 'NONE',  ( -20.38659385541303237, -7.222650657624089199, 49.61879703869475833 ) ) ;
#32823 = VERTEX_POINT ( 'NONE', #27199 ) ;
#32824 = CARTESIAN_POINT ( 'NONE',  ( -17.79108452803360763, -21.84994637594637368, 58.69081321602850920 ) ) ;
#32825 = CARTESIAN_POINT ( 'NONE',  ( -21.42336286209559759, -21.09487474236010485, 69.23945462178221533 ) ) ;
#32826 = LINE ( 'NONE', #29886, #16334 ) ;
#32827 = ORIENTED_EDGE ( 'NONE', *, *, #40704, .T. ) ;
#32828 = FACE_OUTER_BOUND ( 'NONE', #27174, .T. ) ;
#32829 = ADVANCED_FACE ( 'NONE', ( #38025 ), #14363, .F. ) ;
#32830 = CARTESIAN_POINT ( 'NONE',  ( -22.67409364490373491, -14.81069326838761135, 50.77966884056655772 ) ) ;
#32831 = VECTOR ( 'NONE', #32127, 1000.000000000000000 ) ;
#32832 = CARTESIAN_POINT ( 'NONE',  ( -15.27411149333911133, -8.091140114039422571, 74.07985455727100543 ) ) ;
#32833 = EDGE_LOOP ( 'NONE', ( #34034, #19178, #11115, #26775, #37487 ) ) ;
#32834 = CARTESIAN_POINT ( 'NONE',  ( -50.42609385541305755, -14.90920654474421170, 67.05882352941175384 ) ) ;
#32835 = CARTESIAN_POINT ( 'NONE',  ( -20.04849592361258104, -21.35284569240296548, 72.69006679631317525 ) ) ;
#32836 = CARTESIAN_POINT ( 'NONE',  ( -15.55648817577099585, -8.010769314271311003, 74.09457776258329886 ) ) ;
#32837 = ADVANCED_FACE ( 'NONE', ( #26962 ), #267, .T. ) ;
#32838 = CARTESIAN_POINT ( 'NONE',  ( -11.81042834955647258, -10.54382735031610174, 74.45357240259568243 ) ) ;
#32839 = CARTESIAN_POINT ( 'NONE',  ( -20.64396943983181743, -21.02470340508176250, 58.94475165022391394 ) ) ;
#32840 = CARTESIAN_POINT ( 'NONE',  ( -16.60428136649079534, -9.623610389719635450, 50.77966884056655772 ) ) ;
#32841 = ORIENTED_EDGE ( 'NONE', *, *, #40454, .F. ) ;
#32842 = CARTESIAN_POINT ( 'NONE',  ( -36.42409385541304800, -6.859212275519750435, 50.50378509014258555 ) ) ;
#32843 = ADVANCED_FACE ( 'NONE', ( #34091 ), #3699, .T. ) ;
#32844 = CARTESIAN_POINT ( 'NONE',  ( -18.49053343615340239, -7.435173160506244550, 73.95409006490955051 ) ) ;
#32845 = ORIENTED_EDGE ( 'NONE', *, *, #29318, .T. ) ;
#32846 = CARTESIAN_POINT ( 'NONE',  ( -10.04710569707986778, -15.85056516143637140, 64.63054717507066016 ) ) ;
#32847 = ORIENTED_EDGE ( 'NONE', *, *, #8453, .T. ) ;
#32848 = ORIENTED_EDGE ( 'NONE', *, *, #34088, .T. ) ;
#32849 = ORIENTED_EDGE ( 'NONE', *, *, #72, .F. ) ;
#32850 = CARTESIAN_POINT ( 'NONE',  ( -15.46629645379085893, -8.032742063557217094, 70.81809580567336582 ) ) ;
#32851 = CARTESIAN_POINT ( 'NONE',  ( -11.03230825063491594, -10.98182429003440674, 60.79390496990795612 ) ) ;
#32852 = DIRECTION ( 'NONE',  ( 0.7437128929774847741, -0.6684991644116392573, 1.736198598216997869E-08 ) ) ;
#32853 = EDGE_CURVE ( 'NONE', #13885, #16707, #42403, .T. ) ;
#32854 = CARTESIAN_POINT ( 'NONE',  ( -21.88034385759798539, -9.360768649639309658, 51.01397948905920998 ) ) ;
#32855 = AXIS2_PLACEMENT_3D ( 'NONE', #36561, #39802, #2375 ) ;
#32856 = EDGE_CURVE ( 'NONE', #32161, #34852, #28568, .T. ) ;
#32857 = ORIENTED_EDGE ( 'NONE', *, *, #35044, .T. ) ;
#32858 = ORIENTED_EDGE ( 'NONE', *, *, #1361, .T. ) ;
#32859 = CARTESIAN_POINT ( 'NONE',  ( -17.15534385650551741, -7.417179338643134834, 52.18511593390279302 ) ) ;
#32860 = EDGE_CURVE ( 'NONE', #33937, #47544, #8146, .T. ) ;
#32861 = CYLINDRICAL_SURFACE ( 'NONE', #19001, 5.249999999999998224 ) ;
#32862 = CIRCLE ( 'NONE', #7736, 4.686499999999997890 ) ;
#32863 = CARTESIAN_POINT ( 'NONE',  ( -10.81484411697162962, -17.11524594140972155, 61.15743118925659161 ) ) ;
#32864 =( BOUNDED_CURVE ( )  B_SPLINE_CURVE ( 3, ( #684, #47445, #21349, #6565 ),
 .UNSPECIFIED., .F., .F. ) 
 B_SPLINE_CURVE_WITH_KNOTS ( ( 4, 4 ),
 ( 0.4074455897393661763, 0.5000000000000000000 ),
 .UNSPECIFIED. ) 
 CURVE ( )  GEOMETRIC_REPRESENTATION_ITEM ( )  RATIONAL_B_SPLINE_CURVE ( ( 0.6983129098260940637, 0.7760317562607209618, 0.8765941196520292689, 1.000000000000034639 ) ) 
 REPRESENTATION_ITEM ( '' )  );
#32865 = CARTESIAN_POINT ( 'NONE',  ( -19.68659385650551386, -9.302874398569244363, 51.68646062012417985 ) ) ;
#32866 = ORIENTED_EDGE ( 'NONE', *, *, #3038, .T. ) ;
#32867 = B_SPLINE_CURVE_WITH_KNOTS ( 'NONE', 3,
 ( #16184, #12509, #5134, #20142, #27531, #24331, #28008, #31467, #24087, #5627 ),
 .UNSPECIFIED., .F., .F.,
 ( 4, 2, 2, 2, 4 ),
 ( 0.1272669073658321548, 0.2522669073484877789, 0.3772669073311433197, 0.5022669073137989715, 0.6272669072964545123 ),
 .UNSPECIFIED. ) ;
#32868 = DIRECTION ( 'NONE',  ( 0.1847813031241906101, -0.9827796650397888634, 7.910442904995644076E-08 ) ) ;
#32869 = CARTESIAN_POINT ( 'NONE',  ( -22.14090652532222236, -20.04928072148792495, 62.51967078134249078 ) ) ;
#32870 = ORIENTED_EDGE ( 'NONE', *, *, #18050, .T. ) ;
#32871 = FACE_OUTER_BOUND ( 'NONE', #11152, .T. ) ;
#32872 =( BOUNDED_CURVE ( )  B_SPLINE_CURVE ( 3, ( #35339, #5312, #9012, #39032 ),
 .UNSPECIFIED., .F., .F. ) 
 B_SPLINE_CURVE_WITH_KNOTS ( ( 4, 4 ),
 ( 0.000000000000000000, 0.4074455897393750581 ),
 .UNSPECIFIED. ) 
 CURVE ( )  GEOMETRIC_REPRESENTATION_ITEM ( )  RATIONAL_B_SPLINE_CURVE ( ( 1.000000000000000000, 0.4567392136813260839, 0.3561768502900281574, 0.6983129098261062762 ) ) 
 REPRESENTATION_ITEM ( '' )  );
#32873 = ORIENTED_EDGE ( 'NONE', *, *, #9276, .F. ) ;
#32874 = CARTESIAN_POINT ( 'NONE',  ( -14.42683419600288985, -8.428067575814653267, 67.55975083869262221 ) ) ;
#32875 = CARTESIAN_POINT ( 'NONE',  ( -19.47326802145739322, -21.50389079897565736, 65.69316087734659959 ) ) ;
#32876 = CARTESIAN_POINT ( 'NONE',  ( -16.98991503782990975, -22.24662993548692214, 72.35038528954983406 ) ) ;
#32877 = EDGE_LOOP ( 'NONE', ( #37604, #32056, #29304 ) ) ;
#32878 = AXIS2_PLACEMENT_3D ( 'NONE', #25695, #17807, #7742 ) ;
#32879 = CYLINDRICAL_SURFACE ( 'NONE', #20297, 0.1500000000000015210 ) ;
#32880 = CARTESIAN_POINT ( 'NONE',  ( -16.73034385541296132, -6.857644439847485174, 49.98602051094192689 ) ) ;
#32881 = CARTESIAN_POINT ( 'NONE',  ( -10.46944733747312917, -15.96661384539355133, 67.99239968927004441 ) ) ;
#32882 = ORIENTED_EDGE ( 'NONE', *, *, #2708, .F. ) ;
#32883 = CARTESIAN_POINT ( 'NONE',  ( -24.82475127085388422, -15.66597259679895693, 73.11808347143848152 ) ) ;
#32884 = DIRECTION ( 'NONE',  ( -3.071710424422018668E-17, 6.404604876783312462E-16, 1.000000000000000000 ) ) ;
#32885 = VECTOR ( 'NONE', #29962, 1000.000000000000114 ) ;
#32886 = VECTOR ( 'NONE', #4572, 1000.000000000000114 ) ;
#32887 = ORIENTED_EDGE ( 'NONE', *, *, #20219, .T. ) ;
#32888 = CARTESIAN_POINT ( 'NONE',  ( -13.60236376389480384, -20.73382277062339085, 61.80174179654961364 ) ) ;
#32890 = ADVANCED_FACE ( 'NONE', ( #39253 ), #21276, .F. ) ;
#32889 = ORIENTED_EDGE ( 'NONE', *, *, #32729, .F. ) ;
#32891 = CARTESIAN_POINT ( 'NONE',  ( -22.18998830427770841, -20.00468049915955859, 65.71893796558269685 ) ) ;
#32892 = CARTESIAN_POINT ( 'NONE',  ( -13.10056816152199843, -9.240526811222729009, 67.67942760033977834 ) ) ;
#32893 = EDGE_CURVE ( 'NONE', #18335, #47432, #35306, .T. ) ;
#32894 = CARTESIAN_POINT ( 'NONE',  ( -23.22266324395799231, -18.81915189215696671, 65.82389459980581137 ) ) ;
#32895 = VERTEX_POINT ( 'NONE', #5776 ) ;
#32896 = CARTESIAN_POINT ( 'NONE',  ( -10.46253582967156426, -14.07554997744959024, 61.21821325757298382 ) ) ;
#32897 = VECTOR ( 'NONE', #7052, 1000.000000000000114 ) ;
#32898 = CARTESIAN_POINT ( 'NONE',  ( -14.84764829735760827, -8.246537290690364230, 60.33468334944129197 ) ) ;
#32899 = CARTESIAN_POINT ( 'NONE',  ( -24.34138250757122535, -16.17068267630804357, 62.89328676667766160 ) ) ;
#32900 = EDGE_LOOP ( 'NONE', ( #12736, #33940, #34475, #31514 ) ) ;
#32901 = FACE_OUTER_BOUND ( 'NONE', #32716, .T. ) ;
#32902 = CARTESIAN_POINT ( 'NONE',  ( -24.76666462671617097, -16.07013689822947455, 66.17050792933571302 ) ) ;
#32903 = ORIENTED_EDGE ( 'NONE', *, *, #35484, .F. ) ;
#32904 = ORIENTED_EDGE ( 'NONE', *, *, #21237, .F. ) ;
#32905 = CARTESIAN_POINT ( 'NONE',  ( -15.41198273355754900, -21.57429164360176799, 65.26163917071316689 ) ) ;
#32906 = CARTESIAN_POINT ( 'NONE',  ( -13.24203256135214346, -20.97556893053616989, 58.15994682967826179 ) ) ;
#32907 = CARTESIAN_POINT ( 'NONE',  ( -19.86520892150080897, -18.82374422416847537, 49.52966884056656482 ) ) ;
#32908 = CARTESIAN_POINT ( 'NONE',  ( -23.92719381113450083, -11.17417296164256157, 70.00715453762190066 ) ) ;
#32909 = CARTESIAN_POINT ( 'NONE',  ( -23.48344415125163565, -18.41350569598871090, 73.04896097104848707 ) ) ;
#32910 = DIRECTION ( 'NONE',  ( 0.9687793358424821033, -0.2479245821708677133, 0.000000000000000000 ) ) ;
#32911 = CARTESIAN_POINT ( 'NONE',  ( -22.78151580134219500, -19.98625284378301004, 72.75905219260647527 ) ) ;
#32912 = EDGE_CURVE ( 'NONE', #27105, #32937, #47133, .T. ) ;
#32913 = EDGE_LOOP ( 'NONE', ( #3691, #18076, #44362, #16618, #42849 ) ) ;
#32914 = VERTEX_POINT ( 'NONE', #39498 ) ;
#32915 = CARTESIAN_POINT ( 'NONE',  ( -50.42609385541305755, -14.80920654474425291, 71.08235294117645253 ) ) ;
#32916 = EDGE_CURVE ( 'NONE', #11434, #17028, #27687, .T. ) ;
#32917 = EDGE_CURVE ( 'NONE', #45841, #29545, #36025, .T. ) ;
#32918 = EDGE_CURVE ( 'NONE', #26269, #27788, #46884, .T. ) ;
#32919 = CARTESIAN_POINT ( 'NONE',  ( -19.95257394585953747, -8.281687416969214510, 74.02096610897844187 ) ) ;
#32920 = CARTESIAN_POINT ( 'NONE',  ( -14.81535805098777736, -7.777528402031244958, 77.49999999999994316 ) ) ;
#32921 = CARTESIAN_POINT ( 'NONE',  ( -19.03296962921835345, -7.534949906353642923, 67.00797648986954869 ) ) ;
#32922 = CARTESIAN_POINT ( 'NONE',  ( -18.58265938564740338, -7.449833053036199360, 73.94040763329604715 ) ) ;
#32923 = ORIENTED_EDGE ( 'NONE', *, *, #15090, .F. ) ;
#32924 = CARTESIAN_POINT ( 'NONE',  ( -20.55534385650551599, -7.417179338643134834, 52.18511593390279302 ) ) ;
#32925 = AXIS2_PLACEMENT_3D ( 'NONE', #14787, #10888, #29604 ) ;
#32926 = VECTOR ( 'NONE', #823, 1000.000000000000000 ) ;
#32927 = ORIENTED_EDGE ( 'NONE', *, *, #39826, .T. ) ;
#32928 = CARTESIAN_POINT ( 'NONE',  ( -14.60479746972646886, -7.913168098764732150, 60.50491608655884335 ) ) ;
#32929 = CARTESIAN_POINT ( 'NONE',  ( -10.03016471889695183, -15.72215649304404117, 61.08143109537672188 ) ) ;
#32930 = AXIS2_PLACEMENT_3D ( 'NONE', #30328, #37683, #45339 ) ;
#32931 = VERTEX_POINT ( 'NONE', #43200 ) ;
#32932 = CARTESIAN_POINT ( 'NONE',  ( -17.85555652284939043, -7.772123375420258107, 60.09532845646905486 ) ) ;
#32933 = ADVANCED_FACE ( 'NONE', ( #5534 ), #9471, .T. ) ;
#32934 = CARTESIAN_POINT ( 'NONE',  ( 18.62590614458706995, 1.890747609047893185, 50.53028072113869484 ) ) ;
#32935 = ORIENTED_EDGE ( 'NONE', *, *, #13, .T. ) ;
#32936 = CARTESIAN_POINT ( 'NONE',  ( -13.86189509728330904, -11.74550036546145826, 52.02966884056656482 ) ) ;
#32937 = VERTEX_POINT ( 'NONE', #24961 ) ;
#32938 = CARTESIAN_POINT ( 'NONE',  ( -23.86582823559828626, -17.67428107336104404, 62.47920748027621585 ) ) ;
#32939 = CARTESIAN_POINT ( 'NONE',  ( -12.25438268106910833, -10.01050553627876383, 57.29755567529926452 ) ) ;
#32940 = ORIENTED_EDGE ( 'NONE', *, *, #40091, .T. ) ;
#32941 = DIRECTION ( 'NONE',  ( 0.2479245821708712938, 0.9687793358424811041, 0.000000000000000000 ) ) ;
#32942 = CARTESIAN_POINT ( 'NONE',  ( -17.42409385541299471, -14.80920654474435594, 52.02966884056656482 ) ) ;
#32943 = EDGE_CURVE ( 'NONE', #773, #39013, #19916, .T. ) ;
#32944 = EDGE_LOOP ( 'NONE', ( #29422, #14423, #26862, #44495, #31642 ) ) ;
#32945 = CARTESIAN_POINT ( 'NONE',  ( -12.45873566688477929, -9.804017486950373339, 57.10407583662104258 ) ) ;
#32946 =( BOUNDED_SURFACE ( )  B_SPLINE_SURFACE ( 3, 1, ( 
 ( #41106, #42084 ),
 ( #3934, #45069 ),
 ( #34685, #15959 ),
 ( #7636, #27059 ),
 ( #4404, #18681 ),
 ( #8352, #8122 ),
 ( #248, #11316 ) ),
 .UNSPECIFIED., .T., .F., .F. ) 
 B_SPLINE_SURFACE_WITH_KNOTS ( ( 4, 3, 4 ),
 ( 2, 2 ),
 ( 0.000000000000000000, 0.5000000000000000000, 1.000000000000000000 ),
 ( 0.000000000000000000, 1.000000000000000000 ),
 .UNSPECIFIED. ) 
 GEOMETRIC_REPRESENTATION_ITEM ( )  RATIONAL_B_SPLINE_SURFACE ( (
 ( 1.000000000000000000, 1.000000000000000000),
 ( 0.3333333333333335369, 0.3333333333333330373),
 ( 0.3333333333333335369, 0.3333333333333330373),
 ( 1.000000000000000000, 1.000000000000000000),
 ( 0.3333333333333333703, 0.3333333333333333703),
 ( 0.3333333333333333703, 0.3333333333333333703),
 ( 1.000000000000000000, 1.000000000000000000) ) ) 
 REPRESENTATION_ITEM ( '' )  SURFACE ( )  );
#32947 = DIRECTION ( 'NONE',  ( 1.224646799147353207E-16, 1.000000000000000000, -1.912410701131276611E-32 ) ) ;
#32948 = LINE ( 'NONE', #14232, #10904 ) ;
#32949 = ORIENTED_EDGE ( 'NONE', *, *, #24665, .T. ) ;
#32950 = CARTESIAN_POINT ( 'NONE',  ( -19.91241090325594243, -21.83142246198826797, 69.12820776009694157 ) ) ;
#32951 = AXIS2_PLACEMENT_3D ( 'NONE', #41335, #8113, #22891 ) ;
#32952 = AXIS2_PLACEMENT_3D ( 'NONE', #47025, #24391, #42628 ) ;
#32953 = CARTESIAN_POINT ( 'NONE',  ( -11.33353553667378044, -11.35870856699622955, 60.75173739346320190 ) ) ;
#32954 = DIRECTION ( 'NONE',  ( 0.6043825497304157190, -0.7966942535134532433, 5.656674838975381179E-08 ) ) ;
#32955 = ORIENTED_EDGE ( 'NONE', *, *, #9747, .F. ) ;
#32956 = EDGE_LOOP ( 'NONE', ( #20744, #39219, #11473, #9365 ) ) ;
#32957 = CARTESIAN_POINT ( 'NONE',  ( -6.792537093481112898, -14.13189257747792738, 54.60745305979834541 ) ) ;
#32958 = CARTESIAN_POINT ( 'NONE',  ( -11.90533692723668224, -10.50281135863178150, 71.26893075534566435 ) ) ;
#32959 = LINE ( 'NONE', #24876, #546 ) ;
#32960 = AXIS2_PLACEMENT_3D ( 'NONE', #7441, #18490, #18741 ) ;
#32961 = CARTESIAN_POINT ( 'NONE',  ( -13.55534385759799143, -8.623186033802571870, 49.24843789510467218 ) ) ;
#32962 = DIRECTION ( 'NONE',  ( -3.071710424422018668E-17, 6.404604876783312462E-16, 1.000000000000000000 ) ) ;
#32963 = FACE_OUTER_BOUND ( 'NONE', #30308, .T. ) ;
#32964 = CARTESIAN_POINT ( 'NONE',  ( -17.42409385541299471, -14.80920654474434883, 62.02966884056656482 ) ) ;
#32965 = CARTESIAN_POINT ( 'NONE',  ( -16.49760773099677991, -22.20149646633050367, 65.40377166897843608 ) ) ;
#32966 = VERTEX_POINT ( 'NONE', #31865 ) ;
#32967 = CYLINDRICAL_SURFACE ( 'NONE', #14690, 0.1500000000000066835 ) ;
#32968 = EDGE_CURVE ( 'NONE', #40286, #2125, #7353, .T. ) ;
#32969 = EDGE_CURVE ( 'NONE', #11779, #17527, #31691, .T. ) ;
#32970 = CARTESIAN_POINT ( 'NONE',  ( -45.67409385541305511, -14.80920654474410547, 61.49999999999999289 ) ) ;
#32971 = CARTESIAN_POINT ( 'NONE',  ( -16.50454536406711981, -22.20232556258728351, 65.34068991928313608 ) ) ;
#32972 = VERTEX_POINT ( 'NONE', #40229 ) ;
#32973 = ADVANCED_FACE ( 'NONE', ( #18030 ), #10324, .T. ) ;
#32974 = EDGE_CURVE ( 'NONE', #36634, #36681, #38790, .T. ) ;
#32975 = ORIENTED_EDGE ( 'NONE', *, *, #30078, .T. ) ;
#32976 = DIRECTION ( 'NONE',  ( 0.9687793358424821033, -0.2479245821708679909, 0.000000000000000000 ) ) ;
#32977 = CARTESIAN_POINT ( 'NONE',  ( -19.83053741356648558, -21.43962678742999728, 65.67306095859845527 ) ) ;
#32978 = EDGE_CURVE ( 'NONE', #39540, #7278, #8761, .T. ) ;
#32979 = VECTOR ( 'NONE', #42724, 1000.000000000000000 ) ;
#32980 = CARTESIAN_POINT ( 'NONE',  ( -23.30384418855528139, -19.38433790851559735, 58.99136497286766456 ) ) ;
#32981 = DIRECTION ( 'NONE',  ( -0.7841839494287597967, 0.6205284308219183309, 3.872224938349061382E-17 ) ) ;
#32982 = VERTEX_POINT ( 'NONE', #22236 ) ;
#32983 = CARTESIAN_POINT ( 'NONE',  ( -10.43949455435184603, -13.84896052950683476, 57.46297163929641982 ) ) ;
#32984 = EDGE_CURVE ( 'NONE', #26571, #9308, #21520, .T. ) ;
#32985 = ORIENTED_EDGE ( 'NONE', *, *, #25774, .T. ) ;
#32986 = CARTESIAN_POINT ( 'NONE',  ( -21.93816111929147539, -20.22843456855405364, 62.64927864921646261 ) ) ;
#32987 = AXIS2_PLACEMENT_3D ( 'NONE', #44303, #32247, #39622 ) ;
#32988 = CARTESIAN_POINT ( 'NONE',  ( -24.46435014771442695, -14.30944682264569856, 62.86863794226144364 ) ) ;
#32989 =( BOUNDED_CURVE ( )  B_SPLINE_CURVE ( 3, ( #40502, #33334, #36546, #25980 ),
 .UNSPECIFIED., .F., .F. ) 
 B_SPLINE_CURVE_WITH_KNOTS ( ( 4, 4 ),
 ( 0.5000000000000000000, 0.9074455897393675086 ),
 .UNSPECIFIED. ) 
 CURVE ( )  GEOMETRIC_REPRESENTATION_ITEM ( )  RATIONAL_B_SPLINE_CURVE ( ( 1.000000000000003775, 0.4567392136813254178, 0.3561768502900251598, 0.6983129098261069423 ) ) 
 REPRESENTATION_ITEM ( '' )  );
#32990 = CARTESIAN_POINT ( 'NONE',  ( -23.29918407416772297, -19.39037376486758646, 58.99915347576865088 ) ) ;
#32991 = ORIENTED_EDGE ( 'NONE', *, *, #5805, .F. ) ;
#32992 = CARTESIAN_POINT ( 'NONE',  ( -24.14084261439634460, -12.83653908289654488, 70.05626466142305731 ) ) ;
#32993 = ORIENTED_EDGE ( 'NONE', *, *, #47773, .F. ) ;
#32994 = CARTESIAN_POINT ( 'NONE',  ( -17.42409385541299471, -14.80920654474435771, 49.52966884056655772 ) ) ;
#32995 = CARTESIAN_POINT ( 'NONE',  ( -24.38874385864151506, -14.10660391674899827, 69.76161322672021470 ) ) ;
#32996 = VERTEX_POINT ( 'NONE', #32586 ) ;
#32997 = PLANE ( 'NONE',  #39600 ) ;
#32998 = CARTESIAN_POINT ( 'NONE',  ( -36.42409385541304800, -6.859212275519750435, 50.50378509014258555 ) ) ;
#32999 = CARTESIAN_POINT ( 'NONE',  ( -24.28579947082789303, -13.18942387424446316, 62.84736316175410309 ) ) ;
#33000 = CARTESIAN_POINT ( 'NONE',  ( -14.38541658028441184, -8.447521680442473979, 67.55415319938168750 ) ) ;
#33001 = DIRECTION ( 'NONE',  ( 0.000000000000000000, 0.000000000000000000, 1.000000000000000000 ) ) ;
#33002 = DIRECTION ( 'NONE',  ( 2.866981220435666553E-17, -1.000000000000000000, -1.190614954331866791E-16 ) ) ;
#33003 = DIRECTION ( 'NONE',  ( 2.866981220435666553E-17, -1.000000000000000000, -1.190614954331866791E-16 ) ) ;
#33004 = VERTEX_POINT ( 'NONE', #25447 ) ;
#33006 = CARTESIAN_POINT ( 'NONE',  ( -11.93522140360746242, -14.45952210441258678, 54.07175714974879099 ) ) ;
#33005 =( BOUNDED_SURFACE ( )  B_SPLINE_SURFACE ( 3, 1, ( 
 ( #38673, #5193 ),
 ( #45836, #43094 ),
 ( #35212, #31532 ),
 ( #46567, #24148 ),
 ( #12807, #35455 ),
 ( #8398, #16242 ),
 ( #34969, #38418 ) ),
 .UNSPECIFIED., .T., .F., .F. ) 
 B_SPLINE_SURFACE_WITH_KNOTS ( ( 4, 3, 4 ),
 ( 2, 2 ),
 ( 0.000000000000000000, 0.5000000000000000000, 1.000000000000000000 ),
 ( 0.000000000000000000, 1.000000000000000000 ),
 .UNSPECIFIED. ) 
 GEOMETRIC_REPRESENTATION_ITEM ( )  RATIONAL_B_SPLINE_SURFACE ( (
 ( 1.000000000000000000, 1.000000000000000000),
 ( 0.3333333333333335369, 0.3333333333333330373),
 ( 0.3333333333333335369, 0.3333333333333330373),
 ( 1.000000000000000000, 1.000000000000000000),
 ( 0.3333333333333333703, 0.3333333333333333703),
 ( 0.3333333333333333703, 0.3333333333333333703),
 ( 1.000000000000000000, 1.000000000000000000) ) ) 
 REPRESENTATION_ITEM ( '' )  SURFACE ( )  );
#33007 = CYLINDRICAL_SURFACE ( 'NONE', #2223, 0.1500000000000000777 ) ;
#33008 = CARTESIAN_POINT ( 'NONE',  ( -22.69667682133237463, -20.07274909735609825, 69.33451383057273176 ) ) ;
#33009 = CARTESIAN_POINT ( 'NONE',  ( -19.54271803596333257, -21.95161028251255786, 62.14503642488964630 ) ) ;
#33010 = PLANE ( 'NONE',  #11718 ) ;
#33011 = CARTESIAN_POINT ( 'NONE',  ( -24.27720235214249200, -16.23785455720555859, 62.60945374813341147 ) ) ;
#33012 = VERTEX_POINT ( 'NONE', #44412 ) ;
#33013 = ORIENTED_EDGE ( 'NONE', *, *, #16484, .F. ) ;
#33014 = CIRCLE ( 'NONE', #11822, 1.999999999999998890 ) ;
#33015 = CARTESIAN_POINT ( 'NONE',  ( -11.16720021946830244, -11.56054808309503734, 67.91864607954204303 ) ) ;
#33016 = CARTESIAN_POINT ( 'NONE',  ( -45.55409385541305767, -12.76354662275040219, 69.95698270748289360 ) ) ;
#33017 = ORIENTED_EDGE ( 'NONE', *, *, #43997, .T. ) ;
#33019 = CARTESIAN_POINT ( 'NONE',  ( -13.27409385650551599, -9.792211528768504536, 50.49490371617623197 ) ) ;
#33018 = CARTESIAN_POINT ( 'NONE',  ( -23.75243126011088890, -11.69520888738364306, 66.83703234806088744 ) ) ;
#33020 = CARTESIAN_POINT ( 'NONE',  ( -11.34825610409693475, -18.28566130560761849, 57.80714629623370371 ) ) ;
#33021 = AXIS2_PLACEMENT_3D ( 'NONE', #40404, #24680, #24912 ) ;
#33022 = FACE_OUTER_BOUND ( 'NONE', #26553, .T. ) ;
#33023 = CARTESIAN_POINT ( 'NONE',  ( -21.73633048181673999, -9.221757950931626979, 59.87738363463013513 ) ) ;
#33024 = EDGE_CURVE ( 'NONE', #46985, #9191, #11158, .T. ) ;
#33025 = CARTESIAN_POINT ( 'NONE',  ( -22.18998830427770841, -20.00468049915955859, 65.71893796558269685 ) ) ;
#33026 = CARTESIAN_POINT ( 'NONE',  ( -16.88181972730358638, -20.29590995520119989, 53.69233794759168887 ) ) ;
#33027 = CYLINDRICAL_SURFACE ( 'NONE', #16127, 0.1499999999999994116 ) ;
#33028 =( BOUNDED_SURFACE ( )  B_SPLINE_SURFACE ( 3, 1, ( 
 ( #8202, #38459 ),
 ( #34522, #41684 ),
 ( #23219, #27382 ),
 ( #22986, #31081 ),
 ( #20236, #11891 ),
 ( #37973, #34272 ),
 ( #35004, #26666 ) ),
 .UNSPECIFIED., .T., .F., .F. ) 
 B_SPLINE_SURFACE_WITH_KNOTS ( ( 4, 3, 4 ),
 ( 2, 2 ),
 ( 0.000000000000000000, 0.5000000000000000000, 1.000000000000000000 ),
 ( 0.000000000000000000, 1.000000000000000000 ),
 .UNSPECIFIED. ) 
 GEOMETRIC_REPRESENTATION_ITEM ( )  RATIONAL_B_SPLINE_SURFACE ( (
 ( 1.000000000000000000, 1.000000000000000000),
 ( 0.3333333333333335369, 0.3333333333333330373),
 ( 0.3333333333333335369, 0.3333333333333330373),
 ( 1.000000000000000000, 1.000000000000000000),
 ( 0.3333333333333333703, 0.3333333333333333703),
 ( 0.3333333333333333703, 0.3333333333333333703),
 ( 1.000000000000000000, 1.000000000000000000) ) ) 
 REPRESENTATION_ITEM ( '' )  SURFACE ( )  );
#33029 = CARTESIAN_POINT ( 'NONE',  ( -16.42041309862903375, -21.79104485276047853, 58.49405286284293481 ) ) ;
#33030 = EDGE_CURVE ( 'NONE', #46821, #12740, #2783, .T. ) ;
#33031 = ORIENTED_EDGE ( 'NONE', *, *, #43826, .F. ) ;
#33032 = CARTESIAN_POINT ( 'NONE',  ( -19.23707162763026801, -10.47461692831664060, 49.52966884056655772 ) ) ;
#33033 = CARTESIAN_POINT ( 'NONE',  ( -11.59474043620840966, -10.17003886705225568, 71.16231417095823986 ) ) ;
#33034 = CARTESIAN_POINT ( 'NONE',  ( -14.69705846215979328, -19.60099676430529314, 53.69233794759168177 ) ) ;
#33035 = CARTESIAN_POINT ( 'NONE',  ( -17.89121901661899727, -21.84743352196291255, 65.64532279319318775 ) ) ;
#33036 = DIRECTION ( 'NONE',  ( -3.071710424422018668E-17, 6.404604876783312462E-16, 1.000000000000000000 ) ) ;
#33037 = DIRECTION ( 'NONE',  ( -0.3478314405900309048, -0.9375570856950864451, 0.000000000000000000 ) ) ;
#33038 = CARTESIAN_POINT ( 'NONE',  ( -22.16371339239454130, -9.585275839764586081, 59.81351278129218230 ) ) ;
#33039 = ORIENTED_EDGE ( 'NONE', *, *, #12735, .F. ) ;
#33040 = ORIENTED_EDGE ( 'NONE', *, *, #7783, .F. ) ;
#33041 = CARTESIAN_POINT ( 'NONE',  ( -16.22409385541304516, -9.359200813967568422, 50.49621490985803263 ) ) ;
#33042 = EDGE_CURVE ( 'NONE', #38839, #25922, #9711, .T. ) ;
#33043 = EDGE_LOOP ( 'NONE', ( #9356, #3660 ) ) ;
#33044 = CARTESIAN_POINT ( 'NONE',  ( -42.43291738482482600, -14.80920654474415699, 62.92941176470587550 ) ) ;
#33045 = EDGE_CURVE ( 'NONE', #33991, #24829, #29620, .T. ) ;
#33046 = CARTESIAN_POINT ( 'NONE',  ( -20.02395964528090033, -18.70843468947692045, 49.52966884056656482 ) ) ;
#33047 = ADVANCED_FACE ( 'NONE', ( #43938 ), #25134, .T. ) ;
#33048 = CARTESIAN_POINT ( 'NONE',  ( -17.42409385541299471, -14.80920654474435771, 49.52966884056655772 ) ) ;
#33049 = CARTESIAN_POINT ( 'NONE',  ( -9.975093131592752016, -14.93635113986534257, 74.98274190467411415 ) ) ;
#33050 = ORIENTED_EDGE ( 'NONE', *, *, #13742, .T. ) ;
#33051 = CARTESIAN_POINT ( 'NONE',  ( -23.13450524283604182, -10.02421013782724657, 66.70328774705285468 ) ) ;
#33052 = CARTESIAN_POINT ( 'NONE',  ( -11.64902330566212463, -10.02396254413167576, 53.49999999999994316 ) ) ;
#33053 = ORIENTED_EDGE ( 'NONE', *, *, #36737, .F. ) ;
#33054 = FACE_OUTER_BOUND ( 'NONE', #6257, .T. ) ;
#33055 = AXIS2_PLACEMENT_3D ( 'NONE', #18333, #22797, #30185 ) ;
#33056 = CARTESIAN_POINT ( 'NONE',  ( -12.36794914932409561, -19.72224030764921565, 61.39678633597973345 ) ) ;
#33057 = ORIENTED_EDGE ( 'NONE', *, *, #16262, .F. ) ;
#33058 = CARTESIAN_POINT ( 'NONE',  ( -10.88286923018596575, -17.43962093083235843, 68.11193994895104709 ) ) ;
#33059 = CARTESIAN_POINT ( 'NONE',  ( -17.42409385541305511, -14.80920654474410725, 52.21286476528345588 ) ) ;
#33060 = CARTESIAN_POINT ( 'NONE',  ( -23.34092642400682038, -10.28208056094584677, 59.78698708435513254 ) ) ;
#33061 = ORIENTED_EDGE ( 'NONE', *, *, #22500, .T. ) ;
#33062 = LINE ( 'NONE', #14571, #36382 ) ;
#33063 = CARTESIAN_POINT ( 'NONE',  ( -24.36966136476852540, -17.50601128794927774, 69.59995046513768102 ) ) ;
#33064 = CARTESIAN_POINT ( 'NONE',  ( -19.17604249790256077, -21.63836284480991878, 58.53979515915469278 ) ) ;
#33065 = CARTESIAN_POINT ( 'NONE',  ( -11.03557423443333008, -17.80950410671109196, 68.25289248663547426 ) ) ;
#33066 = ORIENTED_EDGE ( 'NONE', *, *, #34201, .F. ) ;
#33067 = LINE ( 'NONE', #18055, #6968 ) ;
#33068 = DIRECTION ( 'NONE',  ( -5.888300610989836252E-06, -9.662809626516592716E-06, 0.9999999999359789893 ) ) ;
#33069 = CYLINDRICAL_SURFACE ( 'NONE', #27048, 0.1500000000000002165 ) ;
#33070 = AXIS2_PLACEMENT_3D ( 'NONE', #9417, #9173, #5483 ) ;
#33071 = CARTESIAN_POINT ( 'NONE',  ( -23.30963478160716562, -18.69084381296369557, 69.30844128244088154 ) ) ;
#33072 = DIRECTION ( 'NONE',  ( 2.083496782661112619E-06, -1.347747140477569176E-07, -0.9999999999978204102 ) ) ;
#33073 = ORIENTED_EDGE ( 'NONE', *, *, #23059, .T. ) ;
#33074 = CARTESIAN_POINT ( 'NONE',  ( -10.37497031247464463, -14.69804315800203298, 71.62782692816419683 ) ) ;
#33075 = CARTESIAN_POINT ( 'NONE',  ( -24.18470913683765389, -12.80901137141652768, 69.78715111652664405 ) ) ;
#33076 = CARTESIAN_POINT ( 'NONE',  ( -18.63018860987378389, -7.457396320151260305, 73.95569119842126327 ) ) ;
#33077 = EDGE_CURVE ( 'NONE', #35817, #20111, #27143, .T. ) ;
#33078 = ORIENTED_EDGE ( 'NONE', *, *, #11707, .T. ) ;
#33079 = CARTESIAN_POINT ( 'NONE',  ( -10.05191582289251961, -15.88326310211563275, 64.70782794937979077 ) ) ;
#33080 = VERTEX_POINT ( 'NONE', #45380 ) ;
#33081 = ORIENTED_EDGE ( 'NONE', *, *, #46363, .T. ) ;
#33082 = ORIENTED_EDGE ( 'NONE', *, *, #47622, .T. ) ;
#33083 = AXIS2_PLACEMENT_3D ( 'NONE', #40841, #7126, #37125 ) ;
#33084 = CARTESIAN_POINT ( 'NONE',  ( -18.84335783304844369, -7.495515834006305056, 70.49351169566308783 ) ) ;
#33085 = CYLINDRICAL_SURFACE ( 'NONE', #9449, 0.1500000000000041578 ) ;
#33086 = CYLINDRICAL_SURFACE ( 'NONE', #29931, 0.1500000000000050460 ) ;
#33087 = CIRCLE ( 'NONE', #39417, 0.5000000000000004441 ) ;
#33088 = ORIENTED_EDGE ( 'NONE', *, *, #28826, .T. ) ;
#33089 = ORIENTED_EDGE ( 'NONE', *, *, #35401, .F. ) ;
#33090 = CARTESIAN_POINT ( 'NONE',  ( -16.76159385650551314, -9.295667164867525756, 49.30633214617472504 ) ) ;
#33091 = EDGE_CURVE ( 'NONE', #27869, #31116, #23217, .T. ) ;
#33092 = DIRECTION ( 'NONE',  ( 0.000000000000000000, 1.000000000000000000, -0.000000000000000000 ) ) ;
#33093 = AXIS2_PLACEMENT_3D ( 'NONE', #34704, #12295, #27075 ) ;
#33094 = CARTESIAN_POINT ( 'NONE',  ( -23.44980453451080393, -18.46889374286061525, 73.06368236440982855 ) ) ;
#33095 = EDGE_CURVE ( 'NONE', #15953, #14238, #30370, .T. ) ;
#33096 = B_SPLINE_CURVE_WITH_KNOTS ( 'NONE', 3,
 ( #37878, #8339, #33674, #38114, #42068, #48718, #26313, #19170, #18926, #3657 ),
 .UNSPECIFIED., .F., .F.,
 ( 4, 2, 2, 2, 4 ),
 ( 0.1272669073658372341, 0.2522669073463233991, 0.3772669073268095641, 0.5022669073072957291, 0.6272669072877818941 ),
 .UNSPECIFIED. ) ;
#33097 = CARTESIAN_POINT ( 'NONE',  ( -18.78659385650551528, -9.302874398569244363, 51.68646062012417985 ) ) ;
#33098 = ORIENTED_EDGE ( 'NONE', *, *, #32601, .T. ) ;
#33099 = EDGE_CURVE ( 'NONE', #12632, #38388, #37176, .T. ) ;
#33100 = CARTESIAN_POINT ( 'NONE',  ( -10.33531725737393181, -17.10115422170377641, 57.87255955594724810 ) ) ;
#33101 = AXIS2_PLACEMENT_3D ( 'NONE', #5840, #28491, #24796 ) ;
#33102 = CARTESIAN_POINT ( 'NONE',  ( -18.77776586261893144, -7.941280436638581186, 66.97359733704600160 ) ) ;
#33103 = CARTESIAN_POINT ( 'NONE',  ( -24.40527839663079845, -14.29480931175867120, 69.65275285367388847 ) ) ;
#33104 = ADVANCED_FACE ( 'NONE', ( #11632 ), #23856, .T. ) ;
#33105 = VERTEX_POINT ( 'NONE', #33785 ) ;
#33106 = CARTESIAN_POINT ( 'NONE',  ( -11.22967102384216886, -11.54873604311523039, 67.91864634137124312 ) ) ;
#33107 = EDGE_CURVE ( 'NONE', #46816, #35760, #11097, .T. ) ;
#33108 = ORIENTED_EDGE ( 'NONE', *, *, #38974, .F. ) ;
#33109 = COLOUR_RGB ( '', 0.72549020, 0.75294118, 0.79215686) ;
#33110 = B_SPLINE_CURVE_WITH_KNOTS ( 'NONE', 3,
 ( #20050, #38757, #8739, #35056 ),
 .UNSPECIFIED., .F., .F.,
 ( 4, 4 ),
 ( 0.000000000000000000, 0.2909959651135547443 ),
 .UNSPECIFIED. ) ;
#33111 = DIRECTION ( 'NONE',  ( -3.071710424422018668E-17, 6.404604876783312462E-16, 1.000000000000000000 ) ) ;
#33112 = CARTESIAN_POINT ( 'NONE',  ( -10.13258936719380898, -16.33817337277914561, 71.63245765104117879 ) ) ;
#33113 = CARTESIAN_POINT ( 'NONE',  ( -6.424093855413055110, -6.359206544744109735, 47.99999999999998579 ) ) ;
#33114 = CARTESIAN_POINT ( 'NONE',  ( -17.23659385541294142, -8.995762431863342456, 51.38120296130598064 ) ) ;
#33115 = B_SPLINE_CURVE_WITH_KNOTS ( 'NONE', 3,
 ( #39790, #44718, #34095, #14872, #26475, #15366, #11701, #384, #18844, #7293 ),
 .UNSPECIFIED., .F., .F.,
 ( 4, 2, 2, 2, 4 ),
 ( 0.000000000000000000, 0.2500000000000000000, 0.5000000000000000000, 0.7500000000000000000, 1.000000000000000000 ),
 .UNSPECIFIED. ) ;
#33116 = VECTOR ( 'NONE', #2338, 1000.000000000000000 ) ;
#33117 = ORIENTED_EDGE ( 'NONE', *, *, #37482, .T. ) ;
#33118 = CARTESIAN_POINT ( 'NONE',  ( -10.33431758219403207, -12.52035302217920254, 60.98348881056122650 ) ) ;
#33119 = CARTESIAN_POINT ( 'NONE',  ( -22.81416393091693706, -19.95214112651346383, 72.84389334246579040 ) ) ;
#33120 = B_SPLINE_CURVE_WITH_KNOTS ( 'NONE', 3,
 ( #15584, #1555, #42199, #23492 ),
 .UNSPECIFIED., .F., .F.,
 ( 4, 4 ),
 ( 0.001310108020964424790, 0.002761379516307284256 ),
 .UNSPECIFIED. ) ;
#33121 = CARTESIAN_POINT ( 'NONE',  ( -14.79922817013080483, -7.836842635312091687, 57.03495431467663224 ) ) ;
#33122 = DIRECTION ( 'NONE',  ( 0.9774082387306984865, -0.2113602016968848807, 7.903122840289808494E-08 ) ) ;
#33123 = ORIENTED_EDGE ( 'NONE', *, *, #186, .F. ) ;
#33124 = DIRECTION ( 'NONE',  ( 5.854827030937197869E-31, 1.020425574103664912E-16, 1.000000000000000000 ) ) ;
#33125 = CARTESIAN_POINT ( 'NONE',  ( -14.60689764421331738, -8.346551857622415582, 63.78978840692987262 ) ) ;
#33126 = CARTESIAN_POINT ( 'NONE',  ( -12.64016520574754843, -19.91947694667972968, 64.93963025601375705 ) ) ;
#33127 = ORIENTED_EDGE ( 'NONE', *, *, #26864, .T. ) ;
#33128 = FACE_BOUND ( 'NONE', #9759, .T. ) ;
#33129 = EDGE_LOOP ( 'NONE', ( #34036, #10625 ) ) ;
#33130 = CARTESIAN_POINT ( 'NONE',  ( 10.57590614458695377, 1.644457370994424572, 49.30478444670939808 ) ) ;
#33131 = LINE ( 'NONE', #48169, #30261 ) ;
#33132 = CARTESIAN_POINT ( 'NONE',  ( -21.18398602608336745, -21.24092397535611809, 65.69958545398036165 ) ) ;
#33133 = ORIENTED_EDGE ( 'NONE', *, *, #9149, .T. ) ;
#33134 = LINE ( 'NONE', #10518, #39408 ) ;
#33135 = ORIENTED_EDGE ( 'NONE', *, *, #4493, .T. ) ;
#33136 =( BOUNDED_CURVE ( )  B_SPLINE_CURVE ( 2, ( #3880, #8073, #33900, #33388, #15408, #4130, #428, #41540, #18886 ),
 .UNSPECIFIED., .F., .F. ) 
 B_SPLINE_CURVE_WITH_KNOTS ( ( 3, 2, 2, 2, 3 ),
 ( 0.03540611873294381706, 0.03638973639061496290, 0.03737335404828610874, 0.03835697170595725458, 0.03934058936362840042 ),
 .UNSPECIFIED. ) 
 CURVE ( )  GEOMETRIC_REPRESENTATION_ITEM ( )  RATIONAL_B_SPLINE_CURVE ( ( 0.9999999999999245048, 0.9238795325113622336, 1.000000000000000000, 0.9238795325112867385, 1.000000000000000000, 0.9238795325112867385, 1.000000000000000000, 0.9238795325113857704, 0.9999999999999009681 ) ) 
 REPRESENTATION_ITEM ( '' )  );
#33137 = ADVANCED_FACE ( 'NONE', ( #19506 ), #36738, .T. ) ;
#33138 = CARTESIAN_POINT ( 'NONE',  ( -23.32532355526320345, -18.57446955825106016, 69.59371930732142175 ) ) ;
#33139 = B_SPLINE_CURVE_WITH_KNOTS ( 'NONE', 1,
 ( #9004, #46904 ),
 .UNSPECIFIED., .F., .F.,
 ( 2, 2 ),
 ( 0.000000000000000000, 1.000000000000000000 ),
 .UNSPECIFIED. ) ;
#33140 = VERTEX_POINT ( 'NONE', #41253 ) ;
#33141 = CARTESIAN_POINT ( 'NONE',  ( -23.83043763270304183, -11.86620476845630101, 59.48235732590898550 ) ) ;
#33142 = CARTESIAN_POINT ( 'NONE',  ( -24.63355139826557760, -12.92841318297298692, 62.94608782021682458 ) ) ;
#33143 = B_SPLINE_CURVE_WITH_KNOTS ( 'NONE', 3,
 ( #32648, #47196, #21342, #44004, #16888, #31928, #40289, #36090, #2128, #13187 ),
 .UNSPECIFIED., .F., .F.,
 ( 4, 2, 2, 2, 4 ),
 ( 0.000000000000000000, 0.2500000000000000000, 0.5000000000000000000, 0.7500000000000000000, 1.000000000000000000 ),
 .UNSPECIFIED. ) ;
#33145 = ORIENTED_EDGE ( 'NONE', *, *, #41187, .F. ) ;
#33144 = AXIS2_PLACEMENT_3D ( 'NONE', #22195, #26134, #36459 ) ;
#33146 = VERTEX_POINT ( 'NONE', #18850 ) ;
#33147 = DIRECTION ( 'NONE',  ( 1.000000000000000000, 2.866981220435666553E-17, 0.000000000000000000 ) ) ;
#33148 = DIRECTION ( 'NONE',  ( -8.766499794606700203E-07, -3.805972782304116817E-07, 0.9999999999995433653 ) ) ;
#33149 = CARTESIAN_POINT ( 'NONE',  ( -10.60168018607446960, -13.23530295033109638, 74.86744747271762890 ) ) ;
#33150 =( BOUNDED_CURVE ( )  B_SPLINE_CURVE ( 3, ( #43659, #17031, #24211, #32079 ),
 .UNSPECIFIED., .F., .F. ) 
 B_SPLINE_CURVE_WITH_KNOTS ( ( 4, 4 ),
 ( 0.5000000000000000000, 0.9074455897393600701 ),
 .UNSPECIFIED. ) 
 CURVE ( )  GEOMETRIC_REPRESENTATION_ITEM ( )  RATIONAL_B_SPLINE_CURVE ( ( 1.000000000000019762, 0.4567392136813480108, 0.3561768502900223288, 0.6983129098260643097 ) ) 
 REPRESENTATION_ITEM ( '' )  );
#33151 = CARTESIAN_POINT ( 'NONE',  ( -21.24554616535955631, -21.20453920045676810, 65.76949338751086316 ) ) ;
#33152 = PLANE ( 'NONE',  #32596 ) ;
#33153 = EDGE_CURVE ( 'NONE', #35243, #30729, #38125, .T. ) ;
#33154 = CARTESIAN_POINT ( 'NONE',  ( -20.44433886619616914, -7.998055119120133227, 66.89448804686142580 ) ) ;
#33155 = VERTEX_POINT ( 'NONE', #26001 ) ;
#33156 = VERTEX_POINT ( 'NONE', #10727 ) ;
#33157 = AXIS2_PLACEMENT_3D ( 'NONE', #39610, #21148, #44058 ) ;
#33158 = DIRECTION ( 'NONE',  ( 2.866981220435666553E-17, -1.000000000000000000, -1.190614954331866791E-16 ) ) ;
#33159 = CARTESIAN_POINT ( 'NONE',  ( -21.06635048418738165, -21.30826373965517817, 62.29966805574095901 ) ) ;
#33160 = CARTESIAN_POINT ( 'NONE',  ( -18.95673185541715711, -7.518389839197517688, 67.03925230700772886 ) ) ;
#33161 = FACE_OUTER_BOUND ( 'NONE', #7201, .T. ) ;
#33162 = VERTEX_POINT ( 'NONE', #3340 ) ;
#33163 = CARTESIAN_POINT ( 'NONE',  ( -19.82409385650551670, -6.426201560718813433, 50.50509628382439331 ) ) ;
#33164 =( BOUNDED_SURFACE ( )  B_SPLINE_SURFACE ( 3, 1, ( 
 ( #23851, #20637 ),
 ( #35632, #1908 ),
 ( #13212, #44266 ),
 ( #14408, #36583 ),
 ( #37080, #7071 ),
 ( #40312, #3115 ),
 ( #6581, #48416 ) ),
 .UNSPECIFIED., .T., .F., .F. ) 
 B_SPLINE_SURFACE_WITH_KNOTS ( ( 4, 3, 4 ),
 ( 2, 2 ),
 ( 0.000000000000000000, 0.5000000000000000000, 1.000000000000000000 ),
 ( 0.000000000000000000, 1.000000000000000000 ),
 .UNSPECIFIED. ) 
 GEOMETRIC_REPRESENTATION_ITEM ( )  RATIONAL_B_SPLINE_SURFACE ( (
 ( 1.000000000000000000, 1.000000000000000000),
 ( 0.3333333333333335369, 0.3333333333333330373),
 ( 0.3333333333333335369, 0.3333333333333330373),
 ( 1.000000000000000000, 1.000000000000000000),
 ( 0.3333333333333333703, 0.3333333333333333703),
 ( 0.3333333333333333703, 0.3333333333333333703),
 ( 1.000000000000000000, 1.000000000000000000) ) ) 
 REPRESENTATION_ITEM ( '' )  SURFACE ( )  );
#33165 = VERTEX_POINT ( 'NONE', #25745 ) ;
#33166 = EDGE_CURVE ( 'NONE', #4941, #29515, #43991, .T. ) ;
#33167 = DIRECTION ( 'NONE',  ( 0.7029450532227031756, 0.7112441579020042370, -7.405715380709557223E-09 ) ) ;
#33168 = CARTESIAN_POINT ( 'NONE',  ( -12.95698253826988022, -9.064354784168759949, 49.69365525927820215 ) ) ;
#33169 = EDGE_CURVE ( 'NONE', #25610, #42180, #37539, .T. ) ;
#33170 = CARTESIAN_POINT ( 'NONE',  ( -10.76542914127749739, -16.97361976459616173, 61.34670158936435769 ) ) ;
#33171 = CARTESIAN_POINT ( 'NONE',  ( -10.49189908542464700, -16.09426454567519116, 68.26295692486267797 ) ) ;
#33172 = EDGE_CURVE ( 'NONE', #21219, #38940, #3402, .T. ) ;
#33173 = ORIENTED_EDGE ( 'NONE', *, *, #38286, .T. ) ;
#33174 = DIRECTION ( 'NONE',  ( -0.7489133456531320565, -0.6626679415081376812, 6.686399169904807862E-09 ) ) ;
#33175 = CARTESIAN_POINT ( 'NONE',  ( -36.42409385541304800, -9.359200813967566646, 50.49621490985803263 ) ) ;
#33176 = ORIENTED_EDGE ( 'NONE', *, *, #45854, .F. ) ;
#33177 = DIRECTION ( 'NONE',  ( -3.071710424422018668E-17, 6.404604876783312462E-16, 1.000000000000000000 ) ) ;
#33178 = EDGE_CURVE ( 'NONE', #35366, #33155, #6998, .T. ) ;
#33179 = CARTESIAN_POINT ( 'NONE',  ( -20.19231670334047735, -8.325423520194950910, 70.40100341277891971 ) ) ;
#33180 = EDGE_LOOP ( 'NONE', ( #36897, #46093, #40159, #9839 ) ) ;
#33181 = CARTESIAN_POINT ( 'NONE',  ( -20.91839533430741227, -20.87517621519315369, 65.86837424650867945 ) ) ;
#33182 = EDGE_CURVE ( 'NONE', #28748, #10266, #35770, .T. ) ;
#33183 = VERTEX_POINT ( 'NONE', #25275 ) ;
#33184 = CARTESIAN_POINT ( 'NONE',  ( -11.81042834955647258, -10.54382735031610174, 74.45357240259568243 ) ) ;
#33185 = CARTESIAN_POINT ( 'NONE',  ( -17.63008012001554192, -7.362005203207129256, 63.74395322827410126 ) ) ;
#33186 = EDGE_LOOP ( 'NONE', ( #23797, #20946, #14674, #386, #28860 ) ) ;
#33187 = EDGE_CURVE ( 'NONE', #10912, #15909, #30182, .T. ) ;
#33188 = EDGE_CURVE ( 'NONE', #8644, #45412, #4651, .T. ) ;
#33189 = CARTESIAN_POINT ( 'NONE',  ( -18.46282016565315587, -21.73182091564523688, 72.28510983673571388 ) ) ;
#33190 = CARTESIAN_POINT ( 'NONE',  ( -10.38078067960954698, -14.50222210708341919, 68.15800126083216526 ) ) ;
#33191 = ORIENTED_EDGE ( 'NONE', *, *, #5733, .T. ) ;
#33192 = CARTESIAN_POINT ( 'NONE',  ( -41.16232914953070576, -14.80920654474427600, 73.09411764705880898 ) ) ;
#33193 = CARTESIAN_POINT ( 'NONE',  ( -19.42045769886998841, -21.57377358197381412, 65.87974951360257592 ) ) ;
#33194 = DIRECTION ( 'NONE',  ( -0.9501515917649785425, -0.3117883138709295898, 1.594035198720926202E-08 ) ) ;
#33195 = ORIENTED_EDGE ( 'NONE', *, *, #34504, .F. ) ;
#33196 = CARTESIAN_POINT ( 'NONE',  ( -12.00582977146459562, -10.37713343423881796, 67.78431519901778302 ) ) ;
#33197 = CARTESIAN_POINT ( 'NONE',  ( -45.38107656289594871, -12.76354662275040219, 70.87000000000000455 ) ) ;
#33198 = ORIENTED_EDGE ( 'NONE', *, *, #15111, .F. ) ;
#33199 = ORIENTED_EDGE ( 'NONE', *, *, #25916, .T. ) ;
#33200 = CARTESIAN_POINT ( 'NONE',  ( -12.78872866433637867, -9.492418930890588413, 70.84925165228416688 ) ) ;
#33201 = DIRECTION ( 'NONE',  ( -1.027096117176089930E-05, -2.598167872330529078E-06, -0.9999999999438783371 ) ) ;
#33202 = CARTESIAN_POINT ( 'NONE',  ( -16.98659385759799179, -7.222650657624104298, 49.61879703869476543 ) ) ;
#33203 = CARTESIAN_POINT ( 'NONE',  ( -23.16908677366360436, -10.06487111558154801, 63.18530634343710517 ) ) ;
#33204 = CARTESIAN_POINT ( 'NONE',  ( -16.82992792493983458, -21.78406743069276885, 68.99560622300008106 ) ) ;
#33205 = CARTESIAN_POINT ( 'NONE',  ( -12.36731040760125744, -9.968228163758537264, 60.57534674602654690 ) ) ;
#33206 = CYLINDRICAL_SURFACE ( 'NONE', #30037, 0.1499999999999964972 ) ;
#33207 = VERTEX_POINT ( 'NONE', #12431 ) ;
#33208 = CARTESIAN_POINT ( 'NONE',  ( -21.99213670719075253, -20.17946569659695299, 59.04970794435396897 ) ) ;
#33209 = EDGE_CURVE ( 'NONE', #32817, #17131, #45703, .T. ) ;
#33210 = CARTESIAN_POINT ( 'NONE',  ( -14.30855566557790226, -8.484641631233271752, 70.74429704309763167 ) ) ;
#33211 = LINE ( 'NONE', #48246, #9097 ) ;
#33212 = CYLINDRICAL_SURFACE ( 'NONE', #18218, 0.1500000000000006883 ) ;
#33213 = EDGE_LOOP ( 'NONE', ( #37631, #35381, #832, #46037, #12112 ) ) ;
#33214 = VERTEX_POINT ( 'NONE', #11961 ) ;
#33215 = CARTESIAN_POINT ( 'NONE',  ( -16.94458633259734270, -7.374567983260779336, 74.14513688882354359 ) ) ;
#33216 = CARTESIAN_POINT ( 'NONE',  ( -13.88293547364789227, -20.90532801101632643, 68.75625136993008368 ) ) ;
#33217 = CARTESIAN_POINT ( 'NONE',  ( -10.70532053225239544, -12.67267096592666498, 61.08381491717225487 ) ) ;
#33218 = FACE_OUTER_BOUND ( 'NONE', #12272, .T. ) ;
#33219 = ORIENTED_EDGE ( 'NONE', *, *, #3273, .F. ) ;
#33220 = B_SPLINE_CURVE_WITH_KNOTS ( 'NONE', 1,
 ( #43546, #47703 ),
 .UNSPECIFIED., .F., .F.,
 ( 2, 2 ),
 ( 0.000000000000000000, 1.000000000000000000 ),
 .UNSPECIFIED. ) ;
#33221 = CARTESIAN_POINT ( 'NONE',  ( -12.86353962931362283, -9.432586330540292607, 74.33395128836551180 ) ) ;
#33222 = VERTEX_POINT ( 'NONE', #38268 ) ;
#33223 = CARTESIAN_POINT ( 'NONE',  ( -13.63868562514487870, -21.22603565268462233, 68.59591802951210582 ) ) ;
#33224 =( BOUNDED_SURFACE ( )  B_SPLINE_SURFACE ( 3, 1, ( 
 ( #6574, #47209 ),
 ( #47933, #36349 ),
 ( #10512, #25518 ),
 ( #35625, #1902 ),
 ( #16905, #48654 ),
 ( #33364, #10741 ),
 ( #34115, #406 ) ),
 .UNSPECIFIED., .T., .F., .F. ) 
 B_SPLINE_SURFACE_WITH_KNOTS ( ( 4, 3, 4 ),
 ( 2, 2 ),
 ( 0.000000000000000000, 0.5000000000000000000, 1.000000000000000000 ),
 ( 0.000000000000000000, 1.000000000000000000 ),
 .UNSPECIFIED. ) 
 GEOMETRIC_REPRESENTATION_ITEM ( )  RATIONAL_B_SPLINE_SURFACE ( (
 ( 1.000000000000000000, 1.000000000000000000),
 ( 0.3333333333333335369, 0.3333333333333330373),
 ( 0.3333333333333335369, 0.3333333333333330373),
 ( 1.000000000000000000, 1.000000000000000000),
 ( 0.3333333333333333703, 0.3333333333333333703),
 ( 0.3333333333333333703, 0.3333333333333333703),
 ( 1.000000000000000000, 1.000000000000000000) ) ) 
 REPRESENTATION_ITEM ( '' )  SURFACE ( )  );
#33225 = CARTESIAN_POINT ( 'NONE',  ( -24.46479344177693349, -14.44719919422189491, 66.18292729247950490 ) ) ;
#33226 = LINE ( 'NONE', #30315, #17049 ) ;
#33227 = ORIENTED_EDGE ( 'NONE', *, *, #11038, .F. ) ;
#33228 = DIRECTION ( 'NONE',  ( 0.9811758422909350186, 0.1931164583992469597, 7.863147543881891826E-08 ) ) ;
#33229 = VERTEX_POINT ( 'NONE', #8268 ) ;
#33230 = CARTESIAN_POINT ( 'NONE',  ( -22.56207008003183745, -19.63703213565221262, 72.92928497383269359 ) ) ;
#33231 = CARTESIAN_POINT ( 'NONE',  ( -19.42896739221782809, -21.56812523091047851, 62.29503644570711174 ) ) ;
#33232 = ORIENTED_EDGE ( 'NONE', *, *, #45296, .T. ) ;
#33233 = CARTESIAN_POINT ( 'NONE',  ( -21.42336380182764088, -21.09487415076890215, 69.23945570945444672 ) ) ;
#33234 = EDGE_CURVE ( 'NONE', #15728, #2461, #16102, .T. ) ;
#33235 = ADVANCED_FACE ( 'NONE', ( #4559 ), #19331, .F. ) ;
#33236 = CARTESIAN_POINT ( 'NONE',  ( -10.27345486655506868, -12.71824029969684844, 64.45331411623358520 ) ) ;
#33237 = AXIS2_PLACEMENT_3D ( 'NONE', #44464, #3828, #29929 ) ;
#33238 = CARTESIAN_POINT ( 'NONE',  ( -20.64284385650552522, -8.811426318492348031, 52.18089403414751359 ) ) ;
#33239 = DIRECTION ( 'NONE',  ( -3.071710424422018668E-17, 6.404604876783312462E-16, 1.000000000000000000 ) ) ;
#33240 = CARTESIAN_POINT ( 'NONE',  ( -23.85820194903862657, -17.69173191509663923, 62.48833042115953873 ) ) ;
#33241 = CARTESIAN_POINT ( 'NONE',  ( -14.00534385759799427, -7.595227055684746986, 51.75156210489594599 ) ) ;
#33242 = CARTESIAN_POINT ( 'NONE',  ( -13.65684165595416921, -8.849801312179289781, 56.98439896120441261 ) ) ;
#33243 = ORIENTED_EDGE ( 'NONE', *, *, #28832, .F. ) ;
#33244 = CARTESIAN_POINT ( 'NONE',  ( -24.87272206221888737, -14.66350473979836444, 62.82022316917439042 ) ) ;
#33245 = CYLINDRICAL_SURFACE ( 'NONE', #39194, 0.1499999999999995226 ) ;
#33246 = CARTESIAN_POINT ( 'NONE',  ( -14.49299406798265011, -7.959851448313194133, 63.92945445847834662 ) ) ;
#33247 = ADVANCED_FACE ( 'NONE', ( #42485 ), #19093, .T. ) ;
#33248 = EDGE_CURVE ( 'NONE', #27479, #8282, #4054, .T. ) ;
#33249 = DIRECTION ( 'NONE',  ( 1.000000000000000000, 0.000000000000000000, 0.000000000000000000 ) ) ;
#33250 = FACE_OUTER_BOUND ( 'NONE', #15811, .T. ) ;
#33251 = CARTESIAN_POINT ( 'NONE',  ( -22.79434678427405814, -9.645412829818440059, 73.65878004203302964 ) ) ;
#33252 = VERTEX_POINT ( 'NONE', #45932 ) ;
#33253 = ORIENTED_EDGE ( 'NONE', *, *, #3409, .T. ) ;
#33254 = CARTESIAN_POINT ( 'NONE',  ( -11.10470733248389230, -18.75498039752055490, 61.46206112672981448 ) ) ;
#33255 = ORIENTED_EDGE ( 'NONE', *, *, #23876, .T. ) ;
#33257 = CARTESIAN_POINT ( 'NONE',  ( -11.71829917361626627, -18.86652339032711012, 71.75856246530707949 ) ) ;
#33256 = CARTESIAN_POINT ( 'NONE',  ( -15.34355019510111617, -7.655489747179978544, 74.20172882442081175 ) ) ;
#33258 = CYLINDRICAL_SURFACE ( 'NONE', #34172, 0.4000000000000006883 ) ;
#33259 = CARTESIAN_POINT ( 'NONE',  ( -12.50376689573318956, -9.829596806175777246, 57.37318925805055159 ) ) ;
#33260 = CARTESIAN_POINT ( 'NONE',  ( -22.27695970603427966, -9.156476278077038344, 59.97817131676683999 ) ) ;
#33261 = FACE_BOUND ( 'NONE', #17019, .T. ) ;
#33262 = DIRECTION ( 'NONE',  ( -0.5652317888644005084, -0.8249321334856241084, 7.911723905267715079E-08 ) ) ;
#33263 = CARTESIAN_POINT ( 'NONE',  ( -11.42803680512448850, -19.23074358453217414, 71.78711645111522444 ) ) ;
#33264 = CARTESIAN_POINT ( 'NONE',  ( -16.74954601956997635, -21.77674034875754927, 68.69560679921868029 ) ) ;
#33265 = EDGE_CURVE ( 'NONE', #18111, #14728, #43696, .T. ) ;
#33266 = ORIENTED_EDGE ( 'NONE', *, *, #40247, .T. ) ;
#33267 = DIRECTION ( 'NONE',  ( -3.071710424422018668E-17, 6.404604876783312462E-16, 1.000000000000000000 ) ) ;
#33268 = CARTESIAN_POINT ( 'NONE',  ( -10.21764062494887781, -12.91954801228597915, 67.92327636273336111 ) ) ;
#33269 = CARTESIAN_POINT ( 'NONE',  ( -15.41159385759799072, -8.990409506049202193, 49.61344411288074951 ) ) ;
#33270 = CARTESIAN_POINT ( 'NONE',  ( -20.69909385759799036, -8.105421454601382081, 49.25000573077640098 ) ) ;
#33271 = DIRECTION ( 'NONE',  ( 0.000000000000000000, 0.000000000000000000, 1.000000000000000000 ) ) ;
#33272 = CARTESIAN_POINT ( 'NONE',  ( -13.71154894328531704, -21.26836094557570433, 68.49979187789318757 ) ) ;
#33273 = CARTESIAN_POINT ( 'NONE',  ( -16.46055638328560278, -21.74386646685260160, 65.29734724012402580 ) ) ;
#33274 = ORIENTED_EDGE ( 'NONE', *, *, #47084, .F. ) ;
#33275 = EDGE_LOOP ( 'NONE', ( #41842, #20415 ) ) ;
#33276 = CARTESIAN_POINT ( 'NONE',  ( -14.93034385541304232, -6.857644439848013640, 49.98602051094139398 ) ) ;
#33277 = EDGE_LOOP ( 'NONE', ( #37118, #46676, #47168, #9656, #25968 ) ) ;
#33278 = CARTESIAN_POINT ( 'NONE',  ( -15.86159385759799001, -7.228003583438117552, 51.38655588711986155 ) ) ;
#33279 = AXIS2_PLACEMENT_3D ( 'NONE', #3715, #26868, #34468 ) ;
#33280 = CARTESIAN_POINT ( 'NONE',  ( -24.03543181337825629, -17.10925231076594599, 69.52225900064301811 ) ) ;
#33281 =( BOUNDED_CURVE ( )  B_SPLINE_CURVE ( 3, ( #6252, #3507, #25675, #3021 ),
 .UNSPECIFIED., .F., .F. ) 
 B_SPLINE_CURVE_WITH_KNOTS ( ( 4, 4 ),
 ( 0.4074455897393663983, 0.5000000000000000000 ),
 .UNSPECIFIED. ) 
 CURVE ( )  GEOMETRIC_REPRESENTATION_ITEM ( )  RATIONAL_B_SPLINE_CURVE ( ( 0.6983129098260830725, 0.7760317562606791064, 0.8765941196519817513, 0.9999999999999834577 ) ) 
 REPRESENTATION_ITEM ( '' )  );
#33282 = CARTESIAN_POINT ( 'NONE',  ( -15.97409385759799072, -6.859212275519751323, 50.50378509014259265 ) ) ;
#33283 = DIRECTION ( 'NONE',  ( -3.071710424422018668E-17, 6.404604876783312462E-16, 1.000000000000000000 ) ) ;
#33284 = VERTEX_POINT ( 'NONE', #27451 ) ;
#33285 = CARTESIAN_POINT ( 'NONE',  ( -13.42824119710918573, -20.62712141855529779, 65.13062048310476371 ) ) ;
#33286 = CARTESIAN_POINT ( 'NONE',  ( -21.00380416015782004, -21.34292312329482399, 62.22976100777699315 ) ) ;
#33287 = ORIENTED_EDGE ( 'NONE', *, *, #8323, .T. ) ;
#33288 = CARTESIAN_POINT ( 'NONE',  ( -45.55409385541305767, -14.20920654474410760, 69.94787228701220272 ) ) ;
#33289 =( BOUNDED_CURVE ( )  B_SPLINE_CURVE ( 3, ( #39877, #6151, #10086, #25110 ),
 .UNSPECIFIED., .F., .F. ) 
 B_SPLINE_CURVE_WITH_KNOTS ( ( 4, 4 ),
 ( 1.570796326794896558, 1.780235837034217283 ),
 .UNSPECIFIED. ) 
 CURVE ( )  GEOMETRIC_REPRESENTATION_ITEM ( )  RATIONAL_B_SPLINE_CURVE ( ( 1.000000000000000000, 0.9963479302455154896, 0.9963479302455154896, 1.000000000000000000 ) ) 
 REPRESENTATION_ITEM ( '' )  );
#33290 = LINE ( 'NONE', #24969, #27495 ) ;
#33291 = ORIENTED_EDGE ( 'NONE', *, *, #29122, .F. ) ;
#33292 = DIRECTION ( 'NONE',  ( -5.731567514496413899E-31, -1.020425574103664789E-16, -1.000000000000000000 ) ) ;
#33293 = LINE ( 'NONE', #94, #41698 ) ;
#33294 = FACE_OUTER_BOUND ( 'NONE', #21786, .T. ) ;
#33295 = ORIENTED_EDGE ( 'NONE', *, *, #27570, .T. ) ;
#33296 = CARTESIAN_POINT ( 'NONE',  ( -11.91859816416373441, -19.82845034313010402, 58.03408211766759450 ) ) ;
#33297 = EDGE_CURVE ( 'NONE', #29013, #5623, #41753, .T. ) ;
#33298 = DIRECTION ( 'NONE',  ( -1.684279434840741878E-06, 5.535644405454969375E-06, -0.9999999999832599462 ) ) ;
#33299 = LINE ( 'NONE', #14575, #39204 ) ;
#33300 = CARTESIAN_POINT ( 'NONE',  ( -17.28496127917699710, -14.43418371046636217, 47.99999999999994316 ) ) ;
#33301 = ORIENTED_EDGE ( 'NONE', *, *, #16075, .F. ) ;
#33302 = CYLINDRICAL_SURFACE ( 'NONE', #43133, 5.249999999999998224 ) ;
#33303 = DIRECTION ( 'NONE',  ( 0.1539336739619741601, 0.9880811829098681276, 6.607022902453645889E-08 ) ) ;
#33304 = CARTESIAN_POINT ( 'NONE',  ( -18.05334954050576357, -21.78092763974751733, 62.10209302353499794 ) ) ;
#33305 = EDGE_CURVE ( 'NONE', #9562, #40815, #38774, .T. ) ;
#33306 = EDGE_CURVE ( 'NONE', #19273, #34260, #34588, .T. ) ;
#33307 = CARTESIAN_POINT ( 'NONE',  ( -21.90534385650552096, -8.801233750844183135, 48.81488406609782515 ) ) ;
#33308 = CIRCLE ( 'NONE', #18388, 1.999999999999999556 ) ;
#33310 = EDGE_CURVE ( 'NONE', #22122, #39770, #19835, .T. ) ;
#33309 = ORIENTED_EDGE ( 'NONE', *, *, #20237, .T. ) ;
#33311 = CARTESIAN_POINT ( 'NONE',  ( -16.16063142123006813, -7.467037929575190525, 60.38523757159160965 ) ) ;
#33312 = LINE ( 'NONE', #37017, #10047 ) ;
#33313 = ORIENTED_EDGE ( 'NONE', *, *, #12884, .T. ) ;
#33314 = CARTESIAN_POINT ( 'NONE',  ( -18.37542852932119430, -7.874153375602881866, 74.03167481725151333 ) ) ;
#33315 = EDGE_CURVE ( 'NONE', #19358, #11201, #15330, .T. ) ;
#33316 = CARTESIAN_POINT ( 'NONE',  ( -15.46798524158586119, -8.087945009721268619, 74.37985622463165214 ) ) ;
#33317 = DIRECTION ( 'NONE',  ( -0.9796876409582463419, 0.2005296141562636081, 7.890952370353029293E-08 ) ) ;
#33318 = ORIENTED_EDGE ( 'NONE', *, *, #20298, .F. ) ;
#33319 = CARTESIAN_POINT ( 'NONE',  ( -10.04821600842096174, -15.85811274820897410, 64.62276192103250594 ) ) ;
#33320 = CARTESIAN_POINT ( 'NONE',  ( -10.68182900717074091, -12.92559417569690439, 68.02215820193474372 ) ) ;
#33321 = ORIENTED_EDGE ( 'NONE', *, *, #45847, .T. ) ;
#33322 = ORIENTED_EDGE ( 'NONE', *, *, #5015, .T. ) ;
#33323 = ADVANCED_FACE ( 'NONE', ( #15136 ), #4326, .F. ) ;
#33324 = VERTEX_POINT ( 'NONE', #30438 ) ;
#33325 = CARTESIAN_POINT ( 'NONE',  ( -15.43659385650551741, -6.915538690918075382, 49.31353937987644542 ) ) ;
#33326 = CARTESIAN_POINT ( 'NONE',  ( -20.43185948505062299, -8.432683554863363184, 66.79576150497511833 ) ) ;
#33327 = CARTESIAN_POINT ( 'NONE',  ( -18.57335281209669731, -21.76520412651811043, 72.57038810541313012 ) ) ;
#33328 = CARTESIAN_POINT ( 'NONE',  ( -24.84853950285492630, -14.19203740149359483, 69.84549430759402355 ) ) ;
#33329 = CARTESIAN_POINT ( 'NONE',  ( -13.30028440927262068, -8.603736347584243660, 60.62605674953037749 ) ) ;
#33330 = ORIENTED_EDGE ( 'NONE', *, *, #47603, .F. ) ;
#33331 = VERTEX_POINT ( 'NONE', #30194 ) ;
#33332 = CARTESIAN_POINT ( 'NONE',  ( -13.38659385650551847, -9.302874398569244363, 51.68646062012417985 ) ) ;
#33333 = B_SPLINE_CURVE_WITH_KNOTS ( 'NONE', 3,
 ( #37837, #41054, #11749, #41541, #44764, #22334, #37094, #3881, #33636, #7826 ),
 .UNSPECIFIED., .F., .F.,
 ( 4, 2, 2, 2, 4 ),
 ( 0.000000000000000000, 0.2500000000000000000, 0.5000000000000000000, 0.7500000000000000000, 1.000000000000000000 ),
 .UNSPECIFIED. ) ;
#33334 = CARTESIAN_POINT ( 'NONE',  ( -10.75506213788527887, -17.10647899198255217, 64.71919382801875997 ) ) ;
#33335 = CARTESIAN_POINT ( 'NONE',  ( -10.81484442788029376, -17.11524687497682251, 61.45743118925498294 ) ) ;
#33336 = CARTESIAN_POINT ( 'NONE',  ( -16.42409385650551812, -6.426201560718813433, 50.50509628382439331 ) ) ;
#33337 = VECTOR ( 'NONE', #40378, 1000.000000000000000 ) ;
#33338 =( BOUNDED_SURFACE ( )  B_SPLINE_SURFACE ( 3, 1, ( 
 ( #25504, #16711 ),
 ( #17192, #24123 ),
 ( #32243, #42841 ),
 ( #28306, #20675 ),
 ( #36804, #31752 ),
 ( #24616, #44474 ),
 ( #46772, #40761 ) ),
 .UNSPECIFIED., .T., .F., .F. ) 
 B_SPLINE_SURFACE_WITH_KNOTS ( ( 4, 3, 4 ),
 ( 2, 2 ),
 ( 0.000000000000000000, 0.5000000000000000000, 1.000000000000000000 ),
 ( 0.000000000000000000, 1.000000000000000000 ),
 .UNSPECIFIED. ) 
 GEOMETRIC_REPRESENTATION_ITEM ( )  RATIONAL_B_SPLINE_SURFACE ( (
 ( 1.000000000000000000, 1.000000000000000000),
 ( 0.3333333333333335369, 0.3333333333333330373),
 ( 0.3333333333333335369, 0.3333333333333330373),
 ( 1.000000000000000000, 1.000000000000000000),
 ( 0.3333333333333333703, 0.3333333333333333703),
 ( 0.3333333333333333703, 0.3333333333333333703),
 ( 1.000000000000000000, 1.000000000000000000) ) ) 
 REPRESENTATION_ITEM ( '' )  SURFACE ( )  );
#33339 = VERTEX_POINT ( 'NONE', #30921 ) ;
#33340 = DIRECTION ( 'NONE',  ( 0.9375570856950865561, -0.3478314405900308492, 0.000000000000000000 ) ) ;
#33341 = CARTESIAN_POINT ( 'NONE',  ( -12.26752988409003287, -16.72227946798956211, 54.49999999999995026 ) ) ;
#33342 = CARTESIAN_POINT ( 'NONE',  ( -24.41275632663629125, -14.38907708926503126, 69.72445513987456422 ) ) ;
#33343 = EDGE_CURVE ( 'NONE', #32538, #35964, #38649, .T. ) ;
#33344 = ORIENTED_EDGE ( 'NONE', *, *, #31692, .F. ) ;
#33345 = FACE_BOUND ( 'NONE', #35594, .T. ) ;
#33346 = ORIENTED_EDGE ( 'NONE', *, *, #1151, .F. ) ;
#33347 = CARTESIAN_POINT ( 'NONE',  ( -13.44410990971816666, -8.986443949771105721, 64.32435409333248799 ) ) ;
#33348 = CARTESIAN_POINT ( 'NONE',  ( -19.56314425575162730, -21.47449014599886752, 65.46486235662891318 ) ) ;
#33349 =( NAMED_UNIT ( * ) PLANE_ANGLE_UNIT ( ) SI_UNIT ( $, .RADIAN. ) );
#33350 = CARTESIAN_POINT ( 'NONE',  ( -11.39127492490111315, -11.16067319722467843, 60.69357916181100876 ) ) ;
#33351 = EDGE_CURVE ( 'NONE', #7024, #32569, #11913, .T. ) ;
#33352 = VERTEX_POINT ( 'NONE', #24976 ) ;
#33353 = CARTESIAN_POINT ( 'NONE',  ( -22.72409385759798894, -9.359200813967568422, 50.49621490985803263 ) ) ;
#33354 = CARTESIAN_POINT ( 'NONE',  ( -45.55409385541305767, -12.70920654474410760, 69.20000000000001705 ) ) ;
#33355 = CARTESIAN_POINT ( 'NONE',  ( -19.36100759928269355, -7.615224647604666330, 60.12126342487893282 ) ) ;
#33356 = DIRECTION ( 'NONE',  ( 1.927470528863119542E-16, 0.000000000000000000, -1.000000000000000000 ) ) ;
#33357 = VERTEX_POINT ( 'NONE', #8994 ) ;
#33358 = DIRECTION ( 'NONE',  ( 3.071710424422018668E-17, -6.404604876783312462E-16, -1.000000000000000000 ) ) ;
#33359 = DIRECTION ( 'NONE',  ( 0.8949343913984054710, -0.4461977533475101065, -3.119193279067933041E-16 ) ) ;
#33360 = CARTESIAN_POINT ( 'NONE',  ( -18.90456104531098092, -7.507023198961870314, 70.55723427638547207 ) ) ;
#33361 = VERTEX_POINT ( 'NONE', #39016 ) ;
#33362 = FACE_BOUND ( 'NONE', #564, .T. ) ;
#33363 = ORIENTED_EDGE ( 'NONE', *, *, #39179, .F. ) ;
#33364 = CARTESIAN_POINT ( 'NONE',  ( -10.64331041279003642, -16.74977650942914309, 58.10249305398041741 ) ) ;
#33365 = CARTESIAN_POINT ( 'NONE',  ( -13.57571756020798581, -20.65642803140422856, 61.51646323935151628 ) ) ;
#33366 = CARTESIAN_POINT ( 'NONE',  ( -14.90981263331598328, -21.39562362703504306, 61.93600440604522817 ) ) ;
#33367 = ADVANCED_FACE ( 'NONE', ( #47393 ), #45572, .T. ) ;
#33368 = CARTESIAN_POINT ( 'NONE',  ( -41.42703503188364778, -14.80920654474424225, 70.97647058823527288 ) ) ;
#33369 = ORIENTED_EDGE ( 'NONE', *, *, #10601, .F. ) ;
#33370 = CARTESIAN_POINT ( 'NONE',  ( -10.45275823860530906, -14.15883715200053317, 64.49876946959942359 ) ) ;
#33371 = EDGE_CURVE ( 'NONE', #44591, #33361, #17327, .T. ) ;
#33372 = ORIENTED_EDGE ( 'NONE', *, *, #19487, .F. ) ;
#33373 = DIRECTION ( 'NONE',  ( -0.6990986543038602008, -0.7150252244155670400, 1.750055599226864974E-16 ) ) ;
#33374 = CARTESIAN_POINT ( 'NONE',  ( -23.37526786102125342, -18.49490670617680266, 69.52045215527557787 ) ) ;
#33375 = ORIENTED_EDGE ( 'NONE', *, *, #33182, .F. ) ;
#33376 = CARTESIAN_POINT ( 'NONE',  ( -10.53028993777715883, -16.28642212234895226, 71.73278239416407587 ) ) ;
#33377 = AXIS2_PLACEMENT_3D ( 'NONE', #41792, #27246, #19615 ) ;
#33378 = EDGE_CURVE ( 'NONE', #32027, #22984, #1834, .T. ) ;
#33379 = CARTESIAN_POINT ( 'NONE',  ( -14.96332094776524357, -21.84106950312725459, 65.25596681347286676 ) ) ;
#33380 = CIRCLE ( 'NONE', #1171, 2.500000000000000444 ) ;
#33381 = ORIENTED_EDGE ( 'NONE', *, *, #150, .T. ) ;
#33382 = VERTEX_POINT ( 'NONE', #43702 ) ;
#33383 = LINE ( 'NONE', #25779, #46940 ) ;
#33384 = CARTESIAN_POINT ( 'NONE',  ( -22.34470984022960138, -19.78791505225649416, 69.17417989488706098 ) ) ;
#33385 = CARTESIAN_POINT ( 'NONE',  ( -10.12326218194131044, -13.32541594658350448, 74.86312942357149325 ) ) ;
#33387 = EDGE_CURVE ( 'NONE', #3383, #43409, #43211, .T. ) ;
#33386 = CARTESIAN_POINT ( 'NONE',  ( -10.03304496037382698, -13.87377773147474613, 57.64813805078288311 ) ) ;
#33388 = CARTESIAN_POINT ( 'NONE',  ( -19.20534385541296629, -7.595227055684692807, 51.75156210489608810 ) ) ;
#33389 = DIRECTION ( 'NONE',  ( 2.515468002857175786E-08, 7.569577117229404680E-10, -0.9999999999999997780 ) ) ;
#33390 = CARTESIAN_POINT ( 'NONE',  ( -13.04909385759799001, -8.112991634885936776, 51.74999426922421719 ) ) ;
#33391 = ORIENTED_EDGE ( 'NONE', *, *, #23691, .F. ) ;
#33392 = EDGE_LOOP ( 'NONE', ( #38368, #17363, #20734, #48450, #5381, #46885, #19453, #46791, #19619, #33219 ) ) ;
#33393 = B_SPLINE_CURVE_WITH_KNOTS ( 'NONE', 1,
 ( #3908, #19154 ),
 .UNSPECIFIED., .F., .F.,
 ( 2, 2 ),
 ( 0.000000000000000000, 1.000000000000000000 ),
 .UNSPECIFIED. ) ;
#33394 = CARTESIAN_POINT ( 'NONE',  ( -12.09316379863263613, -10.27246524284629636, 64.10202428021784726 ) ) ;
#33395 = DIRECTION ( 'NONE',  ( 1.148482745121145911E-06, -2.957121390393632846E-08, -0.9999999999993400834 ) ) ;
#33396 = CARTESIAN_POINT ( 'NONE',  ( -21.07246205680086959, -21.30487707300596512, 62.23658632844267657 ) ) ;
#33397 = DIRECTION ( 'NONE',  ( 0.9687793358424821033, -0.2479245821708677133, 0.000000000000000000 ) ) ;
#33398 = DIRECTION ( 'NONE',  ( -3.071710424422018668E-17, 6.404604876783312462E-16, 1.000000000000000000 ) ) ;
#33399 = VERTEX_POINT ( 'NONE', #35071 ) ;
#33400 = CARTESIAN_POINT ( 'NONE',  ( -17.57409385650551314, -9.792211528768504536, 50.49490371617623197 ) ) ;
#33401 = ORIENTED_EDGE ( 'NONE', *, *, #39173, .F. ) ;
#33402 = CARTESIAN_POINT ( 'NONE',  ( -24.33858701346967734, -15.90815918667622775, 69.76137442214673001 ) ) ;
#33403 = CARTESIAN_POINT ( 'NONE',  ( -24.08517543038346531, -12.49907855475201579, 73.52753481283211556 ) ) ;
#33404 = DIRECTION ( 'NONE',  ( -0.9974380310868017352, -0.07153582418399355436, 3.008056591778321396E-08 ) ) ;
#33405 = EDGE_CURVE ( 'NONE', #48003, #28824, #21548, .T. ) ;
#33406 = VERTEX_POINT ( 'NONE', #6263 ) ;
#33407 = B_SPLINE_CURVE_WITH_KNOTS ( 'NONE', 3,
 ( #17866, #9789, #32665, #2386, #6078, #13924, #47685, #10019, #14164, #25289 ),
 .UNSPECIFIED., .F., .F.,
 ( 4, 2, 2, 2, 4 ),
 ( 0.6272669072877528063, 0.7522669073072690837, 0.8772669073267853612, 1.002266907346301750, 1.127266907365817916 ),
 .UNSPECIFIED. ) ;
#33408 = VECTOR ( 'NONE', #6477, 1000.000000000000114 ) ;
#33409 = CARTESIAN_POINT ( 'NONE',  ( -10.49189908542464522, -16.09426454567519116, 68.26295692486267797 ) ) ;
#33410 = ORIENTED_EDGE ( 'NONE', *, *, #31504, .T. ) ;
#33411 = DIRECTION ( 'NONE',  ( 0.9640890753730593232, -0.2655790932026004803, 6.310348465037888425E-08 ) ) ;
#33412 =( BOUNDED_CURVE ( )  B_SPLINE_CURVE ( 3, ( #43424, #47822, #14058, #39711 ),
 .UNSPECIFIED., .F., .F. ) 
 B_SPLINE_CURVE_WITH_KNOTS ( ( 4, 4 ),
 ( 0.4074455897393701731, 0.5000000000000000000 ),
 .UNSPECIFIED. ) 
 CURVE ( )  GEOMETRIC_REPRESENTATION_ITEM ( )  RATIONAL_B_SPLINE_CURVE ( ( 0.6983129098261028345, 0.7760317562607076392, 0.8765941196520069534, 1.000000000000001554 ) ) 
 REPRESENTATION_ITEM ( '' )  );
#33413 = CYLINDRICAL_SURFACE ( 'NONE', #45632, 2.000000000000001776 ) ;
#33414 = EDGE_LOOP ( 'NONE', ( #46475, #12153, #14173, #5557, #37945 ) ) ;
#33415 = CARTESIAN_POINT ( 'NONE',  ( -15.68502974777997316, -7.977065180327442384, 70.90989839958919561 ) ) ;
#33416 = ORIENTED_EDGE ( 'NONE', *, *, #18522, .T. ) ;
#33417 = DIRECTION ( 'NONE',  ( 0.9687793358424819923, -0.2479245821708680464, 0.000000000000000000 ) ) ;
#33418 = PRODUCT ( 'Governing Air Vane Flywheel Fan', 'Governing Air Vane Flywheel Fan', '', ( #16367 ) ) ;
#33419 = CARTESIAN_POINT ( 'NONE',  ( -12.25221656496721856, -10.01269428147863749, 57.08935561312273421 ) ) ;
#33420 = ORIENTED_EDGE ( 'NONE', *, *, #16956, .F. ) ;
#33421 = CARTESIAN_POINT ( 'NONE',  ( -22.26148258426732340, -19.94273495432607035, 62.44259083056840609 ) ) ;
#33422 = CARTESIAN_POINT ( 'NONE',  ( -18.58312024667335294, -22.16850747602615357, 72.38487304212588924 ) ) ;
#33423 = EDGE_CURVE ( 'NONE', #6404, #20491, #42124, .T. ) ;
#33424 = EDGE_LOOP ( 'NONE', ( #25243, #13059 ) ) ;
#33425 = LINE ( 'NONE', #22377, #11890 ) ;
#33426 = CARTESIAN_POINT ( 'NONE',  ( -17.42558057905623414, -9.559206755253621068, 49.52966884056655772 ) ) ;
#33427 =( BOUNDED_CURVE ( )  B_SPLINE_CURVE ( 3, ( #7539, #4328, #23286, #41255 ),
 .UNSPECIFIED., .F., .F. ) 
 B_SPLINE_CURVE_WITH_KNOTS ( ( 4, 4 ),
 ( 0.5000000000000000000, 0.9074455897393596260 ),
 .UNSPECIFIED. ) 
 CURVE ( )  GEOMETRIC_REPRESENTATION_ITEM ( )  RATIONAL_B_SPLINE_CURVE ( ( 1.000000000000021538, 0.4567392136813413495, 0.3561768502900184985, 0.6983129098260767442 ) ) 
 REPRESENTATION_ITEM ( '' )  );
#33428 = CARTESIAN_POINT ( 'NONE',  ( -23.85760449859744625, -11.05106826658364838, 70.00555402674318373 ) ) ;
#33429 = EDGE_LOOP ( 'NONE', ( #8325, #42609, #43238, #21651, #5803, #36119, #12594, #37161, #32528, #2550, #30980 ) ) ;
#33431 = CARTESIAN_POINT ( 'NONE',  ( -12.26581428767149795, -15.78626943986449405, 50.77966884056655772 ) ) ;
#33430 =( BOUNDED_CURVE ( )  B_SPLINE_CURVE ( 3, ( #6787, #31987, #21800, #7038 ),
 .UNSPECIFIED., .F., .F. ) 
 B_SPLINE_CURVE_WITH_KNOTS ( ( 4, 4 ),
 ( 0.9074455897393665094, 1.000000000000000000 ),
 .UNSPECIFIED. ) 
 CURVE ( )  GEOMETRIC_REPRESENTATION_ITEM ( )  RATIONAL_B_SPLINE_CURVE ( ( 0.6983129098260950629, 0.7760317562606999786, 0.8765941196520016243, 1.000000000000000000 ) ) 
 REPRESENTATION_ITEM ( '' )  );
#33432 = EDGE_CURVE ( 'NONE', #20123, #12513, #43462, .T. ) ;
#33433 = CARTESIAN_POINT ( 'NONE',  ( -12.81450749931373245, -9.474957484202729319, 74.31923006089486705 ) ) ;
#33434 = DIRECTION ( 'NONE',  ( -3.827383491158052452E-06, 8.363078748037870009E-06, 0.9999999999577049437 ) ) ;
#33435 = ORIENTED_EDGE ( 'NONE', *, *, #38447, .T. ) ;
#33436 = ORIENTED_EDGE ( 'NONE', *, *, #16204, .F. ) ;
#33437 = CARTESIAN_POINT ( 'NONE',  ( -22.91296630721855365, -15.15889098507617128, 53.49999999999995026 ) ) ;
#33438 = CARTESIAN_POINT ( 'NONE',  ( -24.37445139888341927, -16.03700657411734198, 59.27899288712937675 ) ) ;
#33439 = DIRECTION ( 'NONE',  ( 0.2075053346947366428, -0.3961584734335814040, 0.8944271909999158554 ) ) ;
#33440 = EDGE_CURVE ( 'NONE', #23343, #21318, #23063, .T. ) ;
#33441 = CARTESIAN_POINT ( 'NONE',  ( -16.64909385759798965, -8.112991634885936776, 51.74999426922421719 ) ) ;
#33442 = DIRECTION ( 'NONE',  ( 0.8858372764600287441, 0.4639960340712823705, 2.848505657311695038E-17 ) ) ;
#33443 = CARTESIAN_POINT ( 'NONE',  ( -12.95890174405234241, -8.844667670358365541, 67.56598159878524257 ) ) ;
#33444 = CARTESIAN_POINT ( 'NONE',  ( -24.08638337272136098, -17.13919944035470522, 66.09924551876292753 ) ) ;
#33445 =( BOUNDED_CURVE ( )  B_SPLINE_CURVE ( 3, ( #19410, #27288, #30759, #46012 ),
 .UNSPECIFIED., .F., .F. ) 
 B_SPLINE_CURVE_WITH_KNOTS ( ( 4, 4 ),
 ( 0.5000000000000000000, 0.9074455897393702841 ),
 .UNSPECIFIED. ) 
 CURVE ( )  GEOMETRIC_REPRESENTATION_ITEM ( )  RATIONAL_B_SPLINE_CURVE ( ( 1.000000000000007772, 0.4567392136813255843, 0.3561768502900223288, 0.6983129098261066092 ) ) 
 REPRESENTATION_ITEM ( '' )  );
#33446 = DIRECTION ( 'NONE',  ( 0.000000000000000000, 0.000000000000000000, -1.000000000000000000 ) ) ;
#33447 = AXIS2_PLACEMENT_3D ( 'NONE', #27186, #11934, #41970 ) ;
#33448 = ORIENTED_EDGE ( 'NONE', *, *, #15545, .T. ) ;
#33449 = CARTESIAN_POINT ( 'NONE',  ( -24.32852063849251323, -13.38246526728995001, 59.37740068604990995 ) ) ;
#33450 = CARTESIAN_POINT ( 'NONE',  ( -14.19282086353638839, -8.542981675383003903, 71.01485553001869278 ) ) ;
#33451 = CARTESIAN_POINT ( 'NONE',  ( -19.99112977906324318, -8.296885409642934306, 74.02096600045412345 ) ) ;
#33452 = CARTESIAN_POINT ( 'NONE',  ( -10.52701369859243208, -13.34860595097322111, 74.67817664682546308 ) ) ;
#33453 = ADVANCED_FACE ( 'NONE', ( #16359 ), #31389, .T. ) ;
#33454 = EDGE_LOOP ( 'NONE', ( #28053, #35775, #8871, #3561 ) ) ;
#33455 = EDGE_CURVE ( 'NONE', #16463, #33382, #1821, .T. ) ;
#33456 = ORIENTED_EDGE ( 'NONE', *, *, #19264, .T. ) ;
#33457 = ADVANCED_FACE ( 'NONE', ( #20569 ), #42960, .T. ) ;
#33458 = DIRECTION ( 'NONE',  ( 0.000000000000000000, 1.000000000000000000, -0.000000000000000000 ) ) ;
#33459 = CARTESIAN_POINT ( 'NONE',  ( -10.64450000169400035, -13.06134498814596334, 71.27998937039448890 ) ) ;
#33460 = CARTESIAN_POINT ( 'NONE',  ( -11.68183240635974407, -10.06254296414596539, 67.67613765047124730 ) ) ;
#33461 = DIRECTION ( 'NONE',  ( 0.9991556020692451412, -0.04108628546905146450, 1.062351070541542511E-16 ) ) ;
#33462 = ORIENTED_EDGE ( 'NONE', *, *, #32405, .F. ) ;
#33463 = CARTESIAN_POINT ( 'NONE',  ( -11.42622084110231029, -18.51434063454204093, 61.27710833181470917 ) ) ;
#33464 = CARTESIAN_POINT ( 'NONE',  ( -22.98984126167822239, -19.13650646057006099, 58.88410662258176842 ) ) ;
#33465 = ORIENTED_EDGE ( 'NONE', *, *, #24071, .T. ) ;
#33466 = CARTESIAN_POINT ( 'NONE',  ( -17.42409385541299471, -14.80920654474435771, 49.52966884056655772 ) ) ;
#33467 = CARTESIAN_POINT ( 'NONE',  ( -17.49776267610204528, -21.86253320314435200, 58.70553367701982239 ) ) ;
#33468 = CARTESIAN_POINT ( 'NONE',  ( -14.01837044221388417, -8.636059239884620098, 74.48482605064899076 ) ) ;
#33469 = ORIENTED_EDGE ( 'NONE', *, *, #40499, .F. ) ;
#33470 = CARTESIAN_POINT ( 'NONE',  ( -21.65477468606848532, -9.232349032746775208, 66.96149992608901869 ) ) ;
#33471 = AXIS2_PLACEMENT_3D ( 'NONE', #47975, #30252, #22866 ) ;
#33472 = EDGE_LOOP ( 'NONE', ( #25268, #30216, #23187, #15542 ) ) ;
#33473 = B_SPLINE_CURVE_WITH_KNOTS ( 'NONE', 1,
 ( #42383, #46070 ),
 .UNSPECIFIED., .F., .F.,
 ( 2, 2 ),
 ( 0.000000000000000000, 1.000000000000000000 ),
 .UNSPECIFIED. ) ;
#33474 = CARTESIAN_POINT ( 'NONE',  ( -10.44610064225645019, -17.41918600737009015, 64.75022468138659804 ) ) ;
#33475 = CARTESIAN_POINT ( 'NONE',  ( -17.19980212172655953, -7.762775302065858085, 70.79035839668003405 ) ) ;
#33476 = ORIENTED_EDGE ( 'NONE', *, *, #18378, .F. ) ;
#33477 = CARTESIAN_POINT ( 'NONE',  ( -16.19792114999740562, -7.866354181730329742, 60.48556343814865954 ) ) ;
#33478 = DIRECTION ( 'NONE',  ( -1.000000000000000000, -2.866981220435666553E-17, 0.000000000000000000 ) ) ;
#33479 = CARTESIAN_POINT ( 'NONE',  ( -21.31784385650551883, -9.790100578890868377, 49.79778022625163203 ) ) ;
#33480 = DIRECTION ( 'NONE',  ( -0.6771828760946864145, 0.7358147540815750398, -3.419290845356464415E-09 ) ) ;
#33481 = CARTESIAN_POINT ( 'NONE',  ( -10.53536195276627829, -13.30851587854854579, 74.69289754060230280 ) ) ;
#33482 = DIRECTION ( 'NONE',  ( -0.9524241471993249997, 0.3047743298226213149, 0.0009228828802126874372 ) ) ;
#33483 = FACE_OUTER_BOUND ( 'NONE', #26928, .T. ) ;
#33484 = EDGE_LOOP ( 'NONE', ( #40136, #1415 ) ) ;
#33485 = CARTESIAN_POINT ( 'NONE',  ( -41.03659385541305937, -14.80920654474410725, 74.09999999999998010 ) ) ;
#33486 = CARTESIAN_POINT ( 'NONE',  ( -45.36800283045199933, -16.43194983366105077, 70.50000000000000000 ) ) ;
#33487 = CARTESIAN_POINT ( 'NONE',  ( -14.42127303407290384, -7.991116021394736535, 63.98253012168138554 ) ) ;
#33488 = DIRECTION ( 'NONE',  ( 0.3478314405900309603, 0.9375570856950864451, -9.567072274253696421E-17 ) ) ;
#33489 = ADVANCED_FACE ( 'NONE', ( #2320 ), #13465, .T. ) ;
#33490 = CARTESIAN_POINT ( 'NONE',  ( -16.13432406759100246, -21.74052631579560568, 58.30057715624173653 ) ) ;
#33491 = CARTESIAN_POINT ( 'NONE',  ( -17.15997071016939302, -7.814068483533316289, 70.79035844394253729 ) ) ;
#33492 = ORIENTED_EDGE ( 'NONE', *, *, #13354, .F. ) ;
#33493 = ORIENTED_EDGE ( 'NONE', *, *, #46151, .T. ) ;
#33494 = B_SPLINE_CURVE_WITH_KNOTS ( 'NONE', 3,
 ( #15933, #46486, #16662, #31449, #5357, #38593, #30977, #27755, #31696, #27272 ),
 .UNSPECIFIED., .F., .F.,
 ( 4, 2, 2, 2, 4 ),
 ( 0.000000000000000000, 0.2500000000000000000, 0.5000000000000000000, 0.7500000000000000000, 1.000000000000000000 ),
 .UNSPECIFIED. ) ;
#33495 = CARTESIAN_POINT ( 'NONE',  ( -11.13733870171179596, -11.61806121328041996, 67.90392505421056057 ) ) ;
#33496 = DIRECTION ( 'NONE',  ( 0.9687793358424819923, -0.2479245821708680464, 0.000000000000000000 ) ) ;
#33497 = EDGE_LOOP ( 'NONE', ( #24461, #29373, #32887, #43165, #10521 ) ) ;
#33499 = CARTESIAN_POINT ( 'NONE',  ( -13.44284385650551705, -8.811426318492348031, 52.18089403414752070 ) ) ;
#33498 = CARTESIAN_POINT ( 'NONE',  ( -10.74628672884880132, -17.07053172313825939, 61.17215199736627795 ) ) ;
#33500 = CARTESIAN_POINT ( 'NONE',  ( -19.80621920301059546, -19.48766556757794532, 50.77966884056656482 ) ) ;
#33501 = CARTESIAN_POINT ( 'NONE',  ( -20.68882847039305872, -8.112503303873584315, 63.43308756725068775 ) ) ;
#33502 = CARTESIAN_POINT ( 'NONE',  ( -21.94242186726961208, -9.397052521110282441, 60.00699132926281010 ) ) ;
#33503 = CARTESIAN_POINT ( 'NONE',  ( -17.42409385541300892, -14.80920654474439679, 47.99999999999994316 ) ) ;
#33504 = CARTESIAN_POINT ( 'NONE',  ( -11.44306888606149819, -19.25104975142471986, 71.88674653068365217 ) ) ;
#33505 = CARTESIAN_POINT ( 'NONE',  ( -11.41497376296057098, -19.21309731666858411, 71.80190493362104576 ) ) ;
#33506 = CARTESIAN_POINT ( 'NONE',  ( -21.99178428503401861, -9.439038574390064440, 60.02171213140443484 ) ) ;
#33507 = ORIENTED_EDGE ( 'NONE', *, *, #24641, .F. ) ;
#33508 = CARTESIAN_POINT ( 'NONE',  ( -24.30048669258562200, -16.36410883687464590, 59.42332431756338451 ) ) ;
#33509 = CARTESIAN_POINT ( 'NONE',  ( -11.50943330868083514, -18.55322154803265988, 61.56245428017365384 ) ) ;
#33510 = CARTESIAN_POINT ( 'NONE',  ( -19.38197731428664028, -19.06713733463150007, 49.52966884056656482 ) ) ;
#33511 = CARTESIAN_POINT ( 'NONE',  ( -24.27425349805069033, -13.36807680166415402, 59.36267976138583435 ) ) ;
#33512 = CARTESIAN_POINT ( 'NONE',  ( -11.77467277675836321, -9.951459619914194477, 64.14259051640634368 ) ) ;
#33513 = FACE_OUTER_BOUND ( 'NONE', #19261, .T. ) ;
#33514 = FACE_OUTER_BOUND ( 'NONE', #21679, .T. ) ;
#33516 = ORIENTED_EDGE ( 'NONE', *, *, #9645, .F. ) ;
#33515 = EDGE_CURVE ( 'NONE', #21061, #10723, #33062, .T. ) ;
#33517 = VECTOR ( 'NONE', #12766, 1000.000000000000000 ) ;
#33518 = ORIENTED_EDGE ( 'NONE', *, *, #36438, .F. ) ;
#33519 = AXIS2_PLACEMENT_3D ( 'NONE', #38383, #42099, #12293 ) ;
#33520 = CARTESIAN_POINT ( 'NONE',  ( -13.47466815348276903, -9.357823189459354651, 50.04126597187313763 ) ) ;
#33521 = ORIENTED_EDGE ( 'NONE', *, *, #12560, .F. ) ;
#33522 = EDGE_CURVE ( 'NONE', #15022, #10119, #48105, .T. ) ;
#33523 = EDGE_CURVE ( 'NONE', #12218, #31226, #2781, .T. ) ;
#33524 = DIRECTION ( 'NONE',  ( 0.6827297667453423591, 0.7306709694519485376, 5.176517822219622992E-09 ) ) ;
#33525 = CARTESIAN_POINT ( 'NONE',  ( -22.47245519635065492, -19.73066437834766873, 72.65872596779033188 ) ) ;
#33526 =( BOUNDED_CURVE ( )  B_SPLINE_CURVE ( 3, ( #40623, #37159, #29808, #44838 ),
 .UNSPECIFIED., .F., .F. ) 
 B_SPLINE_CURVE_WITH_KNOTS ( ( 4, 4 ),
 ( 1.570796326794896558, 1.780235837034216617 ),
 .UNSPECIFIED. ) 
 CURVE ( )  GEOMETRIC_REPRESENTATION_ITEM ( )  RATIONAL_B_SPLINE_CURVE ( ( 1.000000000000000000, 0.9963479302455154896, 0.9963479302455154896, 1.000000000000000000 ) ) 
 REPRESENTATION_ITEM ( '' )  );
#33527 = CARTESIAN_POINT ( 'NONE',  ( -20.08034385759798468, -9.360768649639306105, 51.01397948905921709 ) ) ;
#33528 = CARTESIAN_POINT ( 'NONE',  ( -23.23616624490289695, -18.79948399208958776, 66.12389430041484673 ) ) ;
#33529 = VERTEX_POINT ( 'NONE', #18537 ) ;
#33530 = PLANE ( 'NONE',  #19771 ) ;
#33531 = CARTESIAN_POINT ( 'NONE',  ( -6.424093855413055110, -25.10920654474410441, 45.99999999999998579 ) ) ;
#33532 = ORIENTED_EDGE ( 'NONE', *, *, #36457, .F. ) ;
#33533 = CARTESIAN_POINT ( 'NONE',  ( -23.49605051889219709, -11.22618518380361152, 73.37665428612797314 ) ) ;
#33534 = CARTESIAN_POINT ( 'NONE',  ( -14.69894550035548875, -21.31512775581534669, 61.72780404081314742 ) ) ;
#33535 = ORIENTED_EDGE ( 'NONE', *, *, #39480, .T. ) ;
#33536 = CARTESIAN_POINT ( 'NONE',  ( -17.76832444385116005, -7.367037027254299986, 60.25777669754219801 ) ) ;
#33537 = LINE ( 'NONE', #11401, #5538 ) ;
#33538 = DIRECTION ( 'NONE',  ( -0.000000000000000000, -1.000000000000000000, -0.000000000000000000 ) ) ;
#33539 = ORIENTED_EDGE ( 'NONE', *, *, #25989, .F. ) ;
#33540 = LINE ( 'NONE', #25943, #45870 ) ;
#33541 = ADVANCED_FACE ( 'NONE', ( #32828 ), #25221, .T. ) ;
#33542 = DIRECTION ( 'NONE',  ( 1.000000000000000000, -4.164305804376849172E-17, 1.614929280266638808E-16 ) ) ;
#33543 = B_SPLINE_CURVE_WITH_KNOTS ( 'NONE', 3,
 ( #35347, #42020, #8289, #1615, #6228, #27237, #21253, #46445, #900, #20339 ),
 .UNSPECIFIED., .F., .F.,
 ( 4, 2, 2, 2, 4 ),
 ( 0.1272669073658828920, 0.2522669073463614242, 0.3772669073268399842, 0.5022669073073184887, 0.6272669072877969931 ),
 .UNSPECIFIED. ) ;
#33544 = CARTESIAN_POINT ( 'NONE',  ( -10.75256062612175967, -17.08851307629239358, 61.16302898656469722 ) ) ;
#33545 = CARTESIAN_POINT ( 'NONE',  ( -15.50089181596375276, -21.59567371606877728, 68.57592836473452280 ) ) ;
#33546 = ORIENTED_EDGE ( 'NONE', *, *, #977, .T. ) ;
#33547 = CARTESIAN_POINT ( 'NONE',  ( -11.95727733380162050, -19.27338395605723420, 71.84252737392968413 ) ) ;
#33548 = LINE ( 'NONE', #48593, #11711 ) ;
#33549 = LINE ( 'NONE', #36756, #36440 ) ;
#33550 = AXIS2_PLACEMENT_3D ( 'NONE', #36364, #2645, #10527 ) ;
#33551 = AXIS2_PLACEMENT_3D ( 'NONE', #4024, #804, #7971 ) ;
#33552 = CARTESIAN_POINT ( 'NONE',  ( -17.99499063918263886, -21.78594895119847763, 62.16070588972903010 ) ) ;
#33553 = CARTESIAN_POINT ( 'NONE',  ( -20.16159385650551883, -9.295667164867525756, 49.30633214617472504 ) ) ;
#33554 = EDGE_CURVE ( 'NONE', #42239, #42405, #29633, .T. ) ;
#33555 = VERTEX_POINT ( 'NONE', #10678 ) ;
#33556 = EDGE_CURVE ( 'NONE', #45860, #6783, #33540, .T. ) ;
#33557 = CARTESIAN_POINT ( 'NONE',  ( -24.69852204723760281, -16.41745771733451775, 59.30827817708741634 ) ) ;
#33558 = CARTESIAN_POINT ( 'NONE',  ( -24.69822986944709697, -13.19963441799314197, 59.54763197719577761 ) ) ;
#33559 = ORIENTED_EDGE ( 'NONE', *, *, #12304, .F. ) ;
#33560 = AXIS2_PLACEMENT_3D ( 'NONE', #48098, #14329, #29385 ) ;
#33561 = CARTESIAN_POINT ( 'NONE',  ( -11.57425499491753307, -18.65360305739656610, 64.74707076836355668 ) ) ;
#33562 = DIRECTION ( 'NONE',  ( -2.526377660313140381E-06, -1.273612632024531482E-05, 0.9999999999157043185 ) ) ;
#33563 = EDGE_LOOP ( 'NONE', ( #43382, #19179, #27654, #40273, #47946 ) ) ;
#33564 = FACE_OUTER_BOUND ( 'NONE', #19194, .T. ) ;
#33565 = CARTESIAN_POINT ( 'NONE',  ( -14.59990505495813728, -21.70320363700883703, 58.27279595847587501 ) ) ;
#33566 = ORIENTED_EDGE ( 'NONE', *, *, #47501, .T. ) ;
#33567 = ORIENTED_EDGE ( 'NONE', *, *, #40332, .F. ) ;
#33568 = CARTESIAN_POINT ( 'NONE',  ( -15.88659385650551670, -9.302874398569244363, 51.68646062012417985 ) ) ;
#33569 = CARTESIAN_POINT ( 'NONE',  ( -14.27319502748954783, -8.558459675072437989, 70.72957628730870283 ) ) ;
#33570 = FACE_OUTER_BOUND ( 'NONE', #41136, .T. ) ;
#33571 =( BOUNDED_SURFACE ( )  B_SPLINE_SURFACE ( 3, 1, ( 
 ( #37254, #41455 ),
 ( #29407, #30395 ),
 ( #36759, #37755 ),
 ( #19054, #22019 ),
 ( #4055, #34060 ),
 ( #15336, #44440 ),
 ( #3301, #37016 ) ),
 .UNSPECIFIED., .T., .F., .F. ) 
 B_SPLINE_SURFACE_WITH_KNOTS ( ( 4, 3, 4 ),
 ( 2, 2 ),
 ( 0.000000000000000000, 0.5000000000000000000, 1.000000000000000000 ),
 ( 0.000000000000000000, 1.000000000000000000 ),
 .UNSPECIFIED. ) 
 GEOMETRIC_REPRESENTATION_ITEM ( )  RATIONAL_B_SPLINE_SURFACE ( (
 ( 1.000000000000000000, 1.000000000000000000),
 ( 0.3333333333333335369, 0.3333333333333330373),
 ( 0.3333333333333335369, 0.3333333333333330373),
 ( 1.000000000000000000, 1.000000000000000000),
 ( 0.3333333333333333703, 0.3333333333333333703),
 ( 0.3333333333333333703, 0.3333333333333333703),
 ( 1.000000000000000000, 1.000000000000000000) ) ) 
 REPRESENTATION_ITEM ( '' )  SURFACE ( )  );
#33572 = CARTESIAN_POINT ( 'NONE',  ( -7.924093855413066656, -6.859206544744110623, 52.99999999999997868 ) ) ;
#33573 = CARTESIAN_POINT ( 'NONE',  ( -21.34582186320181307, -20.66775149956831115, 72.82446429489806405 ) ) ;
#33574 = ORIENTED_EDGE ( 'NONE', *, *, #21074, .T. ) ;
#33575 = VERTEX_POINT ( 'NONE', #2570 ) ;
#33576 = CARTESIAN_POINT ( 'NONE',  ( -15.29909385650551634, -8.114302828567740988, 52.18300498402516041 ) ) ;
#33577 = ADVANCED_FACE ( 'NONE', ( #29889 ), #25690, .T. ) ;
#33578 = EDGE_CURVE ( 'NONE', #44829, #23300, #44480, .T. ) ;
#33579 = CARTESIAN_POINT ( 'NONE',  ( -11.44414087091985621, -10.36592030450376711, 74.63873809041486140 ) ) ;
#33580 = CARTESIAN_POINT ( 'NONE',  ( -10.86049441902023460, -17.24231142387962024, 61.23031190884537978 ) ) ;
#33581 = CARTESIAN_POINT ( 'NONE',  ( -15.86159385650551634, -9.295667164867525756, 49.30633214617472504 ) ) ;
#33582 =( BOUNDED_CURVE ( )  B_SPLINE_CURVE ( 3, ( #24692, #13332, #20257, #16298 ),
 .UNSPECIFIED., .F., .F. ) 
 B_SPLINE_CURVE_WITH_KNOTS ( ( 4, 4 ),
 ( 0.5000000000000000000, 0.9074455897393632897 ),
 .UNSPECIFIED. ) 
 CURVE ( )  GEOMETRIC_REPRESENTATION_ITEM ( )  RATIONAL_B_SPLINE_CURVE ( ( 1.000000000000013989, 0.4567392136813422931, 0.3561768502900243827, 0.6983129098260750789 ) ) 
 REPRESENTATION_ITEM ( '' )  );
#33583 = VECTOR ( 'NONE', #41623, 1000.000000000000000 ) ;
#33584 = ADVANCED_FACE ( 'NONE', ( #21533 ), #6747, .T. ) ;
#33586 = ORIENTED_EDGE ( 'NONE', *, *, #28188, .F. ) ;
#33585 = EDGE_CURVE ( 'NONE', #42260, #42072, #3118, .T. ) ;
#33587 = CARTESIAN_POINT ( 'NONE',  ( -21.01124108229941001, -20.87838065962769463, 65.88453944495783787 ) ) ;
#33588 = EDGE_CURVE ( 'NONE', #44748, #21822, #5011, .T. ) ;
#33589 = CARTESIAN_POINT ( 'NONE',  ( -10.48860011681506599, -16.07550809128320424, 68.27208010408295991 ) ) ;
#33590 = AXIS2_PLACEMENT_3D ( 'NONE', #23845, #45779, #31218 ) ;
#33591 = EDGE_CURVE ( 'NONE', #45956, #1066, #6584, .T. ) ;
#33592 = CARTESIAN_POINT ( 'NONE',  ( -24.34278085428046268, -16.17909949234452682, 66.47813813521833026 ) ) ;
#33593 = ORIENTED_EDGE ( 'NONE', *, *, #26943, .T. ) ;
#33594 = CARTESIAN_POINT ( 'NONE',  ( -24.47368665962210343, -14.70950332193510590, 62.72768537250228604 ) ) ;
#33595 = ORIENTED_EDGE ( 'NONE', *, *, #19431, .T. ) ;
#33596 = CARTESIAN_POINT ( 'NONE',  ( -13.11130243257871264, -9.228466417706050251, 63.79457649077198056 ) ) ;
#33597 = CARTESIAN_POINT ( 'NONE',  ( -10.11537057477133139, -16.25405092646076710, 71.58717057996463495 ) ) ;
#33598 = DIRECTION ( 'NONE',  ( -3.071710424422018668E-17, 6.404604876783312462E-16, 1.000000000000000000 ) ) ;
#33599 = DIRECTION ( 'NONE',  ( 0.4846961512978548159, 0.8746825943832683414, 4.196010046976493442E-08 ) ) ;
#33600 = EDGE_CURVE ( 'NONE', #18426, #21687, #35656, .T. ) ;
#33601 = ORIENTED_EDGE ( 'NONE', *, *, #13096, .F. ) ;
#33602 = CARTESIAN_POINT ( 'NONE',  ( -10.40174226954351866, -17.29724918936392442, 61.34238429002267878 ) ) ;
#33603 = LINE ( 'NONE', #41021, #44659 ) ;
#33604 = DIRECTION ( 'NONE',  ( 3.549360974554993999E-17, -6.371834667797928663E-18, -1.000000000000000000 ) ) ;
#33605 = CARTESIAN_POINT ( 'NONE',  ( -10.64577744754535082, -11.71757184301072563, 74.67344733366148546 ) ) ;
#33606 = ORIENTED_EDGE ( 'NONE', *, *, #21745, .T. ) ;
#33607 = DIRECTION ( 'NONE',  ( 1.000000000000000000, 0.000000000000000000, -2.406186529621654018E-16 ) ) ;
#33608 = DIRECTION ( 'NONE',  ( 0.1666496227699783561, -0.9805797387979530155, 0.1033986416233892980 ) ) ;
#33609 = CARTESIAN_POINT ( 'NONE',  ( -10.72305181292425758, -11.55365095252855490, 71.28872070803703309 ) ) ;
#33610 = FACE_BOUND ( 'NONE', #25811, .T. ) ;
#33611 = EDGE_LOOP ( 'NONE', ( #3091, #31255, #2958, #22381, #41533 ) ) ;
#33612 = CARTESIAN_POINT ( 'NONE',  ( -21.37361950556103807, -20.65352744038741051, 69.05449913549048802 ) ) ;
#33613 = CARTESIAN_POINT ( 'NONE',  ( -10.81908394905857129, -17.27465539222630042, 64.63299147090781105 ) ) ;
#33614 = CARTESIAN_POINT ( 'NONE',  ( 18.87590614458706995, 1.902842057076367777, 48.83032374393989272 ) ) ;
#33615 = AXIS2_PLACEMENT_3D ( 'NONE', #27985, #10004, #40047 ) ;
#33616 = CARTESIAN_POINT ( 'NONE',  ( -21.50087588749055811, -8.572740410265922151, 73.71473348964758543 ) ) ;
#33617 = ORIENTED_EDGE ( 'NONE', *, *, #21097, .T. ) ;
#33618 = DIRECTION ( 'NONE',  ( 1.000000000000000000, 0.000000000000000000, 0.000000000000000000 ) ) ;
#33619 = ORIENTED_EDGE ( 'NONE', *, *, #27212, .T. ) ;
#33620 = CARTESIAN_POINT ( 'NONE',  ( -21.36489679027069499, -8.963475500412677377, 73.60128753237400190 ) ) ;
#33621 = CARTESIAN_POINT ( 'NONE',  ( -21.61813339613238227, -8.651787399021619862, 73.71633365192373333 ) ) ;
#33622 = ORIENTED_EDGE ( 'NONE', *, *, #21498, .T. ) ;
#33623 = CARTESIAN_POINT ( 'NONE',  ( -12.68532353738824803, -9.060482037740600347, 71.03420644255490402 ) ) ;
#33624 = MECHANICAL_DESIGN_GEOMETRIC_PRESENTATION_REPRESENTATION (  '', ( #43859 ), #5329 ) ;
#33625 = VECTOR ( 'NONE', #15139, 1000.000000000000000 ) ;
#33626 = CARTESIAN_POINT ( 'NONE',  ( -18.32164519516739531, -22.20506541443370452, 68.99327472290880792 ) ) ;
#33627 = ORIENTED_EDGE ( 'NONE', *, *, #12067, .T. ) ;
#33628 = ORIENTED_EDGE ( 'NONE', *, *, #31968, .F. ) ;
#33629 = ORIENTED_EDGE ( 'NONE', *, *, #40609, .T. ) ;
#33630 = CARTESIAN_POINT ( 'NONE',  ( -12.01648161716052776, -10.28590799842451098, 67.79896869921920199 ) ) ;
#33631 = CARTESIAN_POINT ( 'NONE',  ( -22.71446019751790502, -13.25678923272456977, 53.88362224778183673 ) ) ;
#33632 = CIRCLE ( 'NONE', #30549, 5.249999999999998224 ) ;
#33633 = CARTESIAN_POINT ( 'NONE',  ( -12.50776718604994109, -20.40684089597385764, 71.92158360616595303 ) ) ;
#33634 = PLANE ( 'NONE',  #38138 ) ;
#33635 = ADVANCED_FACE ( 'NONE', ( #26679 ), #12138, .T. ) ;
#33636 = CARTESIAN_POINT ( 'NONE',  ( -14.13370355700781822, -8.630624683693202570, 74.49954649408729779 ) ) ;
#33637 = CARTESIAN_POINT ( 'NONE',  ( -12.93659385759799285, -8.995762431863214559, 51.38120296130585274 ) ) ;
#33638 = AXIS2_PLACEMENT_3D ( 'NONE', #11605, #38422, #37944 ) ;
#33639 = ORIENTED_EDGE ( 'NONE', *, *, #4121, .F. ) ;
#33640 = ORIENTED_EDGE ( 'NONE', *, *, #41129, .T. ) ;
#33641 = CARTESIAN_POINT ( 'NONE',  ( -16.23115966991289127, -7.455249367085269974, 60.31533194998537084 ) ) ;
#33642 = EDGE_CURVE ( 'NONE', #41432, #15343, #37385, .T. ) ;
#33643 = CARTESIAN_POINT ( 'NONE',  ( -22.50034801104533599, -20.26212632374907230, 65.80447478980116216 ) ) ;
#33644 = DIRECTION ( 'NONE',  ( -0.3996021513128670266, -0.9166886716143755054, -9.834836654444679756E-09 ) ) ;
#33645 = CARTESIAN_POINT ( 'NONE',  ( -24.44689184067228638, -14.18710713894228270, 69.93803194250308763 ) ) ;
#33646 = ORIENTED_EDGE ( 'NONE', *, *, #30292, .T. ) ;
#33647 = CARTESIAN_POINT ( 'NONE',  ( -17.46159385650551599, -9.295667164867525756, 49.30633214617472504 ) ) ;
#33648 = ORIENTED_EDGE ( 'NONE', *, *, #35573, .T. ) ;
#33649 = CARTESIAN_POINT ( 'NONE',  ( -11.96181355942711910, -19.87549434724351727, 58.11177690156993947 ) ) ;
#33650 = EDGE_CURVE ( 'NONE', #15048, #32429, #19186, .T. ) ;
#33651 = VECTOR ( 'NONE', #44673, 1000.000000000000114 ) ;
#33652 = CARTESIAN_POINT ( 'NONE',  ( -15.29809733969474195, -21.47854975192407778, 68.87592918283094434 ) ) ;
#33653 = EDGE_CURVE ( 'NONE', #8529, #33207, #7383, .T. ) ;
#33654 = VECTOR ( 'NONE', #2219, 1000.000000000000000 ) ;
#33655 = ORIENTED_EDGE ( 'NONE', *, *, #33315, .F. ) ;
#33656 = CARTESIAN_POINT ( 'NONE',  ( -20.39526016292127863, -7.977138075681091678, 70.41246825231446849 ) ) ;
#33657 = CIRCLE ( 'NONE', #31297, 4.686500000000000554 ) ;
#33658 = VECTOR ( 'NONE', #41266, 1000.000000000000000 ) ;
#33659 = CARTESIAN_POINT ( 'NONE',  ( -22.96484172783137012, -19.08706962207428504, 58.88410642316259214 ) ) ;
#33660 = VERTEX_POINT ( 'NONE', #34786 ) ;
#33661 = CARTESIAN_POINT ( 'NONE',  ( -22.23733845922741637, -19.96043711175405733, 66.00421731380804147 ) ) ;
#33662 = EDGE_CURVE ( 'NONE', #44341, #28874, #7517, .T. ) ;
#33663 = CARTESIAN_POINT ( 'NONE',  ( -10.13542349758729522, -16.35201950153232175, 71.58603826798915293 ) ) ;
#33664 = CARTESIAN_POINT ( 'NONE',  ( -19.11145557798581152, -7.964112677450091660, 63.73089235102099792 ) ) ;
#33665 = ORIENTED_EDGE ( 'NONE', *, *, #34366, .F. ) ;
#33666 = LINE ( 'NONE', #33415, #14130 ) ;
#33667 = ORIENTED_EDGE ( 'NONE', *, *, #618, .F. ) ;
#33668 = CARTESIAN_POINT ( 'NONE',  ( -10.15133553508400510, -13.19036488398009510, 71.32173201719281508 ) ) ;
#33669 = CYLINDRICAL_SURFACE ( 'NONE', #30405, 0.1500000000000051847 ) ;
#33670 = EDGE_LOOP ( 'NONE', ( #12870, #11981, #37508, #23446 ) ) ;
#33671 = CARTESIAN_POINT ( 'NONE',  ( -12.90353999865511625, -8.887351178413068098, 67.49447498869417927 ) ) ;
#33672 = CARTESIAN_POINT ( 'NONE',  ( -20.01098570613759975, -18.73139293731311028, 52.02966884056656482 ) ) ;
#33673 = ORIENTED_EDGE ( 'NONE', *, *, #2469, .T. ) ;
#33674 = CARTESIAN_POINT ( 'NONE',  ( -22.13045097303941233, -9.033809248834419492, 63.33120398871400170 ) ) ;
#33675 = CARTESIAN_POINT ( 'NONE',  ( -22.30126494710644636, -19.83056690705673830, 65.93095126885788204 ) ) ;
#33676 = DIRECTION ( 'NONE',  ( 0.9687793358424821033, -0.2479245821708680464, 0.000000000000000000 ) ) ;
#33677 = EDGE_LOOP ( 'NONE', ( #24332, #3874 ) ) ;
#33678 = CARTESIAN_POINT ( 'NONE',  ( -12.74836358285320159, -20.08597126951521261, 71.82125749157572159 ) ) ;
#33679 = CARTESIAN_POINT ( 'NONE',  ( -20.81428279164019202, -20.99479176755810883, 65.88454167459703115 ) ) ;
#33680 = CARTESIAN_POINT ( 'NONE',  ( -20.19231657184298356, -8.325423463105360966, 70.25100341277898508 ) ) ;
#33681 = ORIENTED_EDGE ( 'NONE', *, *, #46762, .F. ) ;
#33682 = ORIENTED_EDGE ( 'NONE', *, *, #24409, .F. ) ;
#33683 = CARTESIAN_POINT ( 'NONE',  ( -18.72680909822608797, -7.880611277284092608, 70.52068030200462090 ) ) ;
#33684 = LINE ( 'NONE', #22387, #15540 ) ;
#33685 = FACE_OUTER_BOUND ( 'NONE', #28459, .T. ) ;
#33686 = CARTESIAN_POINT ( 'NONE',  ( -14.23034385759799036, -6.857644439848014528, 49.98602051094139398 ) ) ;
#33687 = CARTESIAN_POINT ( 'NONE',  ( -12.49904425988397705, -19.78361547748746219, 61.62352050562626005 ) ) ;
#33688 = CIRCLE ( 'NONE', #30569, 2.000000000000000888 ) ;
#33689 = EDGE_CURVE ( 'NONE', #28462, #42817, #39145, .T. ) ;
#33690 = CYLINDRICAL_SURFACE ( 'NONE', #20438, 0.1500000000000015488 ) ;
#33691 = CARTESIAN_POINT ( 'NONE',  ( -16.95315630909070848, -7.374056537354511498, 74.06679967459766090 ) ) ;
#33692 = B_SPLINE_CURVE_WITH_KNOTS ( 'NONE', 1,
 ( #37049, #22291 ),
 .UNSPECIFIED., .F., .F.,
 ( 2, 2 ),
 ( 0.000000000000000000, 1.000000000000000000 ),
 .UNSPECIFIED. ) ;
#33693 = AXIS2_PLACEMENT_3D ( 'NONE', #46965, #16180, #28261 ) ;
#33694 = CIRCLE ( 'NONE', #32150, 4.686499999999998778 ) ;
#33695 = CARTESIAN_POINT ( 'NONE',  ( -23.17409385650551457, -9.792211528768504536, 50.49490371617623197 ) ) ;
#33696 = EDGE_LOOP ( 'NONE', ( #5294, #18996, #40802, #5963 ) ) ;
#33697 = LINE ( 'NONE', #487, #47002 ) ;
#33698 = DIRECTION ( 'NONE',  ( 1.000000000000000000, 0.000000000000000000, 0.000000000000000000 ) ) ;
#33699 = VECTOR ( 'NONE', #48411, 1000.000000000000000 ) ;
#33700 = DIRECTION ( 'NONE',  ( 0.2466764125338440639, 0.9690979039805150963, -7.162324212090305750E-08 ) ) ;
#33701 = FACE_OUTER_BOUND ( 'NONE', #41717, .T. ) ;
#33702 = ORIENTED_EDGE ( 'NONE', *, *, #9495, .T. ) ;
#33703 = ORIENTED_EDGE ( 'NONE', *, *, #38701, .F. ) ;
#33704 = CARTESIAN_POINT ( 'NONE',  ( -17.42409385541299471, -14.80920654474435771, 49.52966884056655772 ) ) ;
#33705 = DIRECTION ( 'NONE',  ( 0.7915359335728472390, 0.6111226275167354061, 5.146443701300905010E-08 ) ) ;
#33706 = EDGE_CURVE ( 'NONE', #6465, #33919, #20394, .T. ) ;
#33707 = FACE_OUTER_BOUND ( 'NONE', #37462, .T. ) ;
#33708 = CARTESIAN_POINT ( 'NONE',  ( -11.49500183448702906, -10.99442376238782515, 57.22375354680192316 ) ) ;
#33709 = ADVANCED_FACE ( 'NONE', ( #23231 ), #31819, .F. ) ;
#33710 =( BOUNDED_CURVE ( )  B_SPLINE_CURVE ( 3, ( #30457, #22567, #15649, #26505 ),
 .UNSPECIFIED., .F., .F. ) 
 B_SPLINE_CURVE_WITH_KNOTS ( ( 4, 4 ),
 ( 4.712388980384690562, 4.921828490624009511 ),
 .UNSPECIFIED. ) 
 CURVE ( )  GEOMETRIC_REPRESENTATION_ITEM ( )  RATIONAL_B_SPLINE_CURVE ( ( 1.000000000000000000, 0.9963479302455156006, 0.9963479302455156006, 1.000000000000000000 ) ) 
 REPRESENTATION_ITEM ( '' )  );
#33711 = ORIENTED_EDGE ( 'NONE', *, *, #39967, .T. ) ;
#33712 = CARTESIAN_POINT ( 'NONE',  ( -13.56393070069739437, -8.909737636684434747, 57.26407933515372406 ) ) ;
#33713 = ADVANCED_FACE ( 'NONE', ( #9669 ), #43401, .F. ) ;
#33714 = CARTESIAN_POINT ( 'NONE',  ( -14.22441598498101989, -8.081217260141077219, 67.44470407312981308 ) ) ;
#33715 = ORIENTED_EDGE ( 'NONE', *, *, #41927, .T. ) ;
#33716 = DIRECTION ( 'NONE',  ( -3.071710424422018668E-17, 6.404604876783312462E-16, 1.000000000000000000 ) ) ;
#33717 = CIRCLE ( 'NONE', #43995, 4.686499999999997890 ) ;
#33718 = EDGE_CURVE ( 'NONE', #12524, #2153, #450, .T. ) ;
#33719 = CARTESIAN_POINT ( 'NONE',  ( -36.42409385541304800, -9.359200813967566646, 50.49621490985803263 ) ) ;
#33720 = CARTESIAN_POINT ( 'NONE',  ( -24.65023647254185590, -12.99629722456026393, 63.01759562046499497 ) ) ;
#33721 = CARTESIAN_POINT ( 'NONE',  ( -24.36611147337434957, -16.04009697885371111, 66.07797069094537790 ) ) ;
#33722 =( BOUNDED_SURFACE ( )  B_SPLINE_SURFACE ( 3, 1, ( 
 ( #33794, #44661 ),
 ( #37484, #21529 ),
 ( #18533, #10675 ),
 ( #3031, #3776 ),
 ( #25217, #36509 ),
 ( #6982, #7242 ),
 ( #10921, #47862 ) ),
 .UNSPECIFIED., .T., .F., .F. ) 
 B_SPLINE_SURFACE_WITH_KNOTS ( ( 4, 3, 4 ),
 ( 2, 2 ),
 ( 0.000000000000000000, 0.5000000000000000000, 1.000000000000000000 ),
 ( 0.000000000000000000, 1.000000000000000000 ),
 .UNSPECIFIED. ) 
 GEOMETRIC_REPRESENTATION_ITEM ( )  RATIONAL_B_SPLINE_SURFACE ( (
 ( 1.000000000000000000, 1.000000000000000000),
 ( 0.3333333333333335369, 0.3333333333333330373),
 ( 0.3333333333333335369, 0.3333333333333330373),
 ( 1.000000000000000000, 1.000000000000000000),
 ( 0.3333333333333333703, 0.3333333333333333703),
 ( 0.3333333333333333703, 0.3333333333333333703),
 ( 1.000000000000000000, 1.000000000000000000) ) ) 
 REPRESENTATION_ITEM ( '' )  SURFACE ( )  );
#33723 = VERTEX_POINT ( 'NONE', #39451 ) ;
#33724 =( BOUNDED_CURVE ( )  B_SPLINE_CURVE ( 3, ( #13618, #29383, #25680, #44654 ),
 .UNSPECIFIED., .F., .F. ) 
 B_SPLINE_CURVE_WITH_KNOTS ( ( 4, 4 ),
 ( 0.4074455897393692849, 0.5000000000000000000 ),
 .UNSPECIFIED. ) 
 CURVE ( )  GEOMETRIC_REPRESENTATION_ITEM ( )  RATIONAL_B_SPLINE_CURVE ( ( 0.6983129098261070533, 0.7760317562606993125, 0.8765941196519936307, 0.9999999999999824585 ) ) 
 REPRESENTATION_ITEM ( '' )  );
#33725 = CARTESIAN_POINT ( 'NONE',  ( -12.25434429315920859, -20.17366997322574562, 65.05170215947674706 ) ) ;
#33726 = AXIS2_PLACEMENT_3D ( 'NONE', #45113, #3728, #11359 ) ;
#33727 = EDGE_LOOP ( 'NONE', ( #2777, #5275 ) ) ;
#33728 = CARTESIAN_POINT ( 'NONE',  ( -19.64401462542318200, -21.92156298671864434, 62.10848288909245696 ) ) ;
#33729 = CARTESIAN_POINT ( 'NONE',  ( -24.72409385541305582, -15.80920654474410725, 65.99999999999998579 ) ) ;
#33730 = B_SPLINE_CURVE_WITH_KNOTS ( 'NONE', 1,
 ( #18146, #21390 ),
 .UNSPECIFIED., .F., .F.,
 ( 2, 2 ),
 ( 0.000000000000000000, 1.000000000000000000 ),
 .UNSPECIFIED. ) ;
#33731 = ORIENTED_EDGE ( 'NONE', *, *, #3935, .F. ) ;
#33732 = LINE ( 'NONE', #29, #47486 ) ;
#33733 = CARTESIAN_POINT ( 'NONE',  ( -19.90648311238531676, -10.83415612659009319, 49.52966884056655772 ) ) ;
#33734 = CARTESIAN_POINT ( 'NONE',  ( -19.68659385650551386, -9.302874398569244363, 51.68646062012417985 ) ) ;
#33735 = CARTESIAN_POINT ( 'NONE',  ( -10.35661233123872371, -12.45241144375540365, 60.91358254413026430 ) ) ;
#33736 = VECTOR ( 'NONE', #25957, 1000.000000000000000 ) ;
#33737 = EDGE_CURVE ( 'NONE', #44867, #10407, #2259, .T. ) ;
#33738 = FACE_OUTER_BOUND ( 'NONE', #6532, .T. ) ;
#33739 = CARTESIAN_POINT ( 'NONE',  ( 22.62590614458706639, 1.890747609047612077, 50.53028072113853142 ) ) ;
#33740 = PLANE ( 'NONE',  #5425 ) ;
#33741 = ORIENTED_EDGE ( 'NONE', *, *, #37904, .F. ) ;
#33742 = CARTESIAN_POINT ( 'NONE',  ( -22.41159385541302385, -8.990409506049225286, 49.61344411288072820 ) ) ;
#33743 =( BOUNDED_CURVE ( )  B_SPLINE_CURVE ( 3, ( #45649, #569, #4032, #11645 ),
 .UNSPECIFIED., .F., .F. ) 
 B_SPLINE_CURVE_WITH_KNOTS ( ( 4, 4 ),
 ( 4.712388980384690562, 4.921828490624010399 ),
 .UNSPECIFIED. ) 
 CURVE ( )  GEOMETRIC_REPRESENTATION_ITEM ( )  RATIONAL_B_SPLINE_CURVE ( ( 1.000000000000000000, 0.9963479302455154896, 0.9963479302455154896, 1.000000000000000000 ) ) 
 REPRESENTATION_ITEM ( '' )  );
#33744 = EDGE_CURVE ( 'NONE', #31776, #25382, #34073, .T. ) ;
#33745 = DIRECTION ( 'NONE',  ( -0.3478314405900307937, -0.9375570856950865561, 0.000000000000000000 ) ) ;
#33746 = CARTESIAN_POINT ( 'NONE',  ( -18.26273199447633999, -21.75878827259743886, 65.45418175178663489 ) ) ;
#33747 = CARTESIAN_POINT ( 'NONE',  ( -11.90657572125106967, -10.42057778141185231, 70.96893122942475429 ) ) ;
#33748 = DIRECTION ( 'NONE',  ( 1.000000000000000000, 0.000000000000000000, -5.466375705775733989E-17 ) ) ;
#33749 = CARTESIAN_POINT ( 'NONE',  ( -46.47622156840087371, -14.20920654474410760, 70.87000000000000455 ) ) ;
#33750 = ORIENTED_EDGE ( 'NONE', *, *, #28959, .T. ) ;
#33751 = ORIENTED_EDGE ( 'NONE', *, *, #15323, .F. ) ;
#33752 = CARTESIAN_POINT ( 'NONE',  ( -23.99387123153590551, -11.29613222128559258, 66.46568589023691231 ) ) ;
#33753 = CARTESIAN_POINT ( 'NONE',  ( -9.975693985146712350, -14.64899972753946145, 71.50595426662775367 ) ) ;
#33754 = ORIENTED_EDGE ( 'NONE', *, *, #18349, .F. ) ;
#33756 = CARTESIAN_POINT ( 'NONE',  ( -27.42409385541305511, -27.10920654474410796, 54.99999999999997868 ) ) ;
#33755 = DIRECTION ( 'NONE',  ( -3.071710424422018668E-17, 6.404604876783312462E-16, 1.000000000000000000 ) ) ;
#33757 = CARTESIAN_POINT ( 'NONE',  ( -24.20826218283995246, -13.07918557588831376, 66.53076680535011178 ) ) ;
#33758 = CARTESIAN_POINT ( 'NONE',  ( -22.97409385541299542, -6.859212275519753099, 50.50378509014307582 ) ) ;
#33759 = CYLINDRICAL_SURFACE ( 'NONE', #6164, 0.5000000000000004441 ) ;
#33760 = EDGE_CURVE ( 'NONE', #10444, #42299, #32032, .T. ) ;
#33761 = CARTESIAN_POINT ( 'NONE',  ( -12.06214182864563078, -19.98150860846456212, 61.59016925282919885 ) ) ;
#33762 = CARTESIAN_POINT ( 'NONE',  ( -17.42409385541299471, -14.80920654474435771, 49.52966884056655772 ) ) ;
#33763 = CARTESIAN_POINT ( 'NONE',  ( -13.96821274855622441, -8.721769818545135777, 74.30840771363131125 ) ) ;
#33764 = DIRECTION ( 'NONE',  ( 1.616182858256118783E-16, 0.003028072113822189229, -0.9999954153791275058 ) ) ;
#33765 = B_SPLINE_CURVE_WITH_KNOTS ( 'NONE', 1,
 ( #14995, #30548 ),
 .UNSPECIFIED., .F., .F.,
 ( 2, 2 ),
 ( 0.000000000000000000, 1.000000000000000000 ),
 .UNSPECIFIED. ) ;
#33766 = CARTESIAN_POINT ( 'NONE',  ( -17.11594671439511828, -7.315539529225059567, 47.99999999999994316 ) ) ;
#33767 = VERTEX_POINT ( 'NONE', #27876 ) ;
#33768 = CARTESIAN_POINT ( 'NONE',  ( -14.25068859620040840, -8.513811488652077486, 70.72957628655862550 ) ) ;
#33769 = CARTESIAN_POINT ( 'NONE',  ( -15.80034074178659331, -19.80179363221599331, 52.02966884056656482 ) ) ;
#33770 = AXIS2_PLACEMENT_3D ( 'NONE', #10918, #17563, #32594 ) ;
#33771 = CARTESIAN_POINT ( 'NONE',  ( -12.08969920365285944, -20.00986870243187710, 61.49655014346812720 ) ) ;
#33772 = CARTESIAN_POINT ( 'NONE',  ( -10.66703313327717240, -12.79807994555918960, 64.56836111017611302 ) ) ;
#33773 = CARTESIAN_POINT ( 'NONE',  ( -24.30998853687411554, -13.26019858907717897, 66.44679832887018733 ) ) ;
#33774 = CARTESIAN_POINT ( 'NONE',  ( -13.93897074462874919, -20.93787812888889377, 68.74153005185598886 ) ) ;
#33775 = ADVANCED_FACE ( 'NONE', ( #47334 ), #46362, .F. ) ;
#33776 = VECTOR ( 'NONE', #10166, 1000.000000000000000 ) ;
#33777 = EDGE_LOOP ( 'NONE', ( #7960, #2442, #19817, #24611, #8786 ) ) ;
#33778 = EDGE_LOOP ( 'NONE', ( #7372, #41511, #43646, #36418, #43791 ) ) ;
#33779 = PRESENTATION_STYLE_ASSIGNMENT (( #45371 ) ) ;
#33780 = EDGE_LOOP ( 'NONE', ( #40937, #10738, #40757, #27024, #7505 ) ) ;
#33781 = DIRECTION ( 'NONE',  ( 2.866981220435666553E-17, -1.000000000000000000, -1.190614954331866791E-16 ) ) ;
#33782 = VECTOR ( 'NONE', #26453, 1000.000000000000000 ) ;
#33783 = EDGE_CURVE ( 'NONE', #22563, #2683, #29375, .T. ) ;
#33784 = CARTESIAN_POINT ( 'NONE',  ( -11.23238687730323626, -11.54381762185194660, 64.25767991630246456 ) ) ;
#33785 = CARTESIAN_POINT ( 'NONE',  ( -17.19980177718173309, -7.762775310937220397, 70.49035839668022163 ) ) ;
#33786 = ORIENTED_EDGE ( 'NONE', *, *, #28521, .T. ) ;
#33787 = APPLICATION_CONTEXT ( 'automotive_design' ) ;
#33788 = EDGE_CURVE ( 'NONE', #4739, #44291, #27642, .T. ) ;
#33789 = CARTESIAN_POINT ( 'NONE',  ( -10.98557796499954087, -17.68114198556070349, 71.86718193507100239 ) ) ;
#33790 = ORIENTED_EDGE ( 'NONE', *, *, #20870, .F. ) ;
#33791 = CARTESIAN_POINT ( 'NONE',  ( -22.32470100883011099, -20.42066193515545791, 62.35722264172714802 ) ) ;
#33792 = CARTESIAN_POINT ( 'NONE',  ( -16.44703096029287437, -9.650926977002853846, 49.52966884056655772 ) ) ;
#33793 = EDGE_LOOP ( 'NONE', ( #3509, #5550, #34486, #47937, #26278 ) ) ;
#33794 = CARTESIAN_POINT ( 'NONE',  ( -19.49109506855409180, -21.54969648977046148, 62.28031529404344013 ) ) ;
#33795 = FACE_OUTER_BOUND ( 'NONE', #37501, .T. ) ;
#33796 = CARTESIAN_POINT ( 'NONE',  ( -9.981760932757149263, -14.47101872614397955, 67.95825874778591924 ) ) ;
#33797 = ORIENTED_EDGE ( 'NONE', *, *, #21964, .T. ) ;
#33798 = AXIS2_PLACEMENT_3D ( 'NONE', #34659, #27515, #5117 ) ;
#33799 = AXIS2_PLACEMENT_3D ( 'NONE', #4942, #34952, #16226 ) ;
#33800 = ADVANCED_FACE ( 'NONE', ( #24194, #46837 ), #13564, .T. ) ;
#33801 = CARTESIAN_POINT ( 'NONE',  ( -24.69856829750257177, -13.20119948815759159, 59.40621968628075678 ) ) ;
#33802 = CARTESIAN_POINT ( 'NONE',  ( -21.78444843227217120, -20.35286453386188299, 59.17931667745679647 ) ) ;
#33803 = ORIENTED_EDGE ( 'NONE', *, *, #9009, .F. ) ;
#33804 = FACE_OUTER_BOUND ( 'NONE', #10638, .T. ) ;
#33805 = DIRECTION ( 'NONE',  ( 1.927470528863119542E-16, 0.000000000000000000, -1.000000000000000000 ) ) ;
#33806 = AXIS2_PLACEMENT_3D ( 'NONE', #7766, #14854, #11936 ) ;
#33807 = DIRECTION ( 'NONE',  ( -1.075201462585828720E-05, 1.608194665399622665E-06, 0.9999999999409039386 ) ) ;
#33808 = ADVANCED_FACE ( 'NONE', ( #5731 ), #28375, .T. ) ;
#33809 = CARTESIAN_POINT ( 'NONE',  ( -17.99534012058598620, -21.78591885189985788, 61.89038380837850184 ) ) ;
#33810 = CARTESIAN_POINT ( 'NONE',  ( -23.89575787814031926, -11.11856224597834242, 70.08484892979208780 ) ) ;
#33811 = CARTESIAN_POINT ( 'NONE',  ( -10.47914989750023729, -15.69558448425602926, 64.73601526215637136 ) ) ;
#33812 = EDGE_CURVE ( 'NONE', #27713, #7442, #17435, .T. ) ;
#33813 = ADVANCED_FACE ( 'NONE', ( #2017 ), #35258, .T. ) ;
#33814 = CARTESIAN_POINT ( 'NONE',  ( -19.48659385650551457, -9.302874398569244363, 51.68646062012417985 ) ) ;
#33815 = EDGE_CURVE ( 'NONE', #42531, #35822, #13314, .T. ) ;
#33816 = VERTEX_POINT ( 'NONE', #12853 ) ;
#33817 = FACE_OUTER_BOUND ( 'NONE', #19952, .T. ) ;
#33818 = CARTESIAN_POINT ( 'NONE',  ( -14.35020019311386719, -8.022098033332648370, 63.90323595109556720 ) ) ;
#33819 = ORIENTED_EDGE ( 'NONE', *, *, #30844, .F. ) ;
#33820 = FACE_OUTER_BOUND ( 'NONE', #31432, .T. ) ;
#33821 = AXIS2_PLACEMENT_3D ( 'NONE', #2154, #43296, #9571 ) ;
#33822 = DIRECTION ( 'NONE',  ( 0.9687793358424821033, -0.2479245821708679909, 0.000000000000000000 ) ) ;
#33823 = DIRECTION ( 'NONE',  ( 0.3478314405900310158, 0.9375570856950865561, 6.371834667863454192E-18 ) ) ;
#33824 = B_SPLINE_CURVE_WITH_KNOTS ( 'NONE', 3,
 ( #20437, #1722, #16715, #16950, #20181, #24127, #12306, #43336, #42359, #4684 ),
 .UNSPECIFIED., .F., .F.,
 ( 4, 2, 2, 2, 4 ),
 ( 0.6272669072877878893, 0.7522669073072835166, 0.8772669073267791440, 1.002266907346274660, 1.127266907365770399 ),
 .UNSPECIFIED. ) ;
#33825 = VERTEX_POINT ( 'NONE', #36682 ) ;
#33826 = CARTESIAN_POINT ( 'NONE',  ( -24.47217469780903798, -14.64471797168181233, 63.01296487297644688 ) ) ;
#33827 = CARTESIAN_POINT ( 'NONE',  ( -10.39241571269986331, -17.41794234916963191, 54.27966884056652219 ) ) ;
#33828 = ORIENTED_EDGE ( 'NONE', *, *, #2789, .F. ) ;
#33829 = CARTESIAN_POINT ( 'NONE',  ( -15.54909385650551634, -8.104110260919579645, 48.81699501597546487 ) ) ;
#33830 =( BOUNDED_CURVE ( )  B_SPLINE_CURVE ( 3, ( #11943, #855, #31626, #27434 ),
 .UNSPECIFIED., .F., .F. ) 
 B_SPLINE_CURVE_WITH_KNOTS ( ( 4, 4 ),
 ( 0.4074455897393707282, 0.5000000000000000000 ),
 .UNSPECIFIED. ) 
 CURVE ( )  GEOMETRIC_REPRESENTATION_ITEM ( )  RATIONAL_B_SPLINE_CURVE ( ( 0.6983129098261023904, 0.7760317562606998676, 0.8765941196519971834, 0.9999999999999897859 ) ) 
 REPRESENTATION_ITEM ( '' )  );
#33831 = CARTESIAN_POINT ( 'NONE',  ( 23.52590614458706852, 3.890747609047893185, 50.53028072113869484 ) ) ;
#33832 = CARTESIAN_POINT ( 'NONE',  ( -14.36817892824948473, -8.455618309860652104, 67.54503025475186462 ) ) ;
#33833 = B_SPLINE_CURVE_WITH_KNOTS ( 'NONE', 1,
 ( #42675, #4503 ),
 .UNSPECIFIED., .F., .F.,
 ( 2, 2 ),
 ( 0.000000000000000000, 1.000000000000000000 ),
 .UNSPECIFIED. ) ;
#33834 = DIRECTION ( 'NONE',  ( 0.000000000000000000, 0.000000000000000000, -1.000000000000000000 ) ) ;
#33835 = CARTESIAN_POINT ( 'NONE',  ( -13.51640533490032503, -9.001381809737894812, 57.19640993782574157 ) ) ;
#33836 = EDGE_LOOP ( 'NONE', ( #37582, #4753, #22672, #10481, #24777 ) ) ;
#33837 = ORIENTED_EDGE ( 'NONE', *, *, #35252, .T. ) ;
#33838 = CARTESIAN_POINT ( 'NONE',  ( -13.66784385650551670, -6.428312510596451368, 51.20221977374900035 ) ) ;
#33839 = EDGE_CURVE ( 'NONE', #42725, #4116, #2505, .T. ) ;
#33840 = AXIS2_PLACEMENT_3D ( 'NONE', #31150, #5065, #11970 ) ;
#33841 = CARTESIAN_POINT ( 'NONE',  ( -23.34117154248328063, -11.06912743251672104, 73.47079241152631823 ) ) ;
#33842 = CARTESIAN_POINT ( 'NONE',  ( -21.81933826130772047, -16.43558560955401404, 49.52966884056655772 ) ) ;
#33843 = CARTESIAN_POINT ( 'NONE',  ( -15.13034385650551528, -9.794322478646142471, 51.19202720610083901 ) ) ;
#33844 = AXIS2_PLACEMENT_3D ( 'NONE', #23484, #42440, #34056 ) ;
#33845 = PRODUCT ( 'Tuned Steel Comb Vibration Teeth', 'Tuned Steel Comb Vibration Teeth', '', ( #45718 ) ) ;
#33846 = ORIENTED_EDGE ( 'NONE', *, *, #3901, .F. ) ;
#33847 = CARTESIAN_POINT ( 'NONE',  ( -15.79261328423922706, -21.67602794760135154, 72.20142491214876657 ) ) ;
#33848 = EDGE_CURVE ( 'NONE', #39290, #42831, #8925, .T. ) ;
#33849 = DIRECTION ( 'NONE',  ( -3.071710424422018668E-17, 6.404604876783312462E-16, 1.000000000000000000 ) ) ;
#33850 = CIRCLE ( 'NONE', #22852, 1.999999999999999112 ) ;
#33851 = DIRECTION ( 'NONE',  ( 0.000000000000000000, -0.007114381193220190198, 0.9999746924698832418 ) ) ;
#33852 = ORIENTED_EDGE ( 'NONE', *, *, #45557, .T. ) ;
#33853 = CARTESIAN_POINT ( 'NONE',  ( -50.42609385541305755, -14.80920654474414810, 61.02352941176469869 ) ) ;
#33854 = VERTEX_POINT ( 'NONE', #22190 ) ;
#33855 = CARTESIAN_POINT ( 'NONE',  ( -12.53168694236654979, -9.190697399280059798, 74.51197142868565493 ) ) ;
#33856 = DIRECTION ( 'NONE',  ( -2.699622400625883127E-06, 1.161037828378819543E-05, 0.9999999999289554964 ) ) ;
#33857 = DIRECTION ( 'NONE',  ( -3.071710424422018668E-17, 6.404604876783312462E-16, 1.000000000000000000 ) ) ;
#33858 = CARTESIAN_POINT ( 'NONE',  ( -21.54575282610021247, -21.01526529837170543, 72.71784754957664632 ) ) ;
#33859 = VECTOR ( 'NONE', #37893, 1000.000000000000000 ) ;
#33860 = ORIENTED_EDGE ( 'NONE', *, *, #25648, .T. ) ;
#33861 = CARTESIAN_POINT ( 'NONE',  ( -10.74628672884880309, -17.07053172313825939, 61.17215199736627795 ) ) ;
#33862 = DIRECTION ( 'NONE',  ( 0.000000000000000000, 0.000000000000000000, 1.000000000000000000 ) ) ;
#33863 = CARTESIAN_POINT ( 'NONE',  ( -23.54569140518488624, -19.05536029250058050, 65.93894040291287695 ) ) ;
#33864 = CARTESIAN_POINT ( 'NONE',  ( -24.37683854932038585, -15.97618581480151434, 66.21324926630431662 ) ) ;
#33865 = EDGE_LOOP ( 'NONE', ( #27721, #19277, #10887, #45893 ) ) ;
#33866 = CARTESIAN_POINT ( 'NONE',  ( -19.55370996603141975, -21.94834978302637651, 62.19492417698030806 ) ) ;
#33867 = CARTESIAN_POINT ( 'NONE',  ( -18.30602013973305020, -21.80685202924323463, 72.69999788315199396 ) ) ;
#33868 = CARTESIAN_POINT ( 'NONE',  ( -24.72409385541305582, -14.90920654474424190, 70.97647058823527288 ) ) ;
#33869 = FACE_BOUND ( 'NONE', #37087, .T. ) ;
#33870 = ORIENTED_EDGE ( 'NONE', *, *, #3198, .T. ) ;
#33871 = AXIS2_PLACEMENT_3D ( 'NONE', #29488, #25795, #36609 ) ;
#33872 = EDGE_CURVE ( 'NONE', #34362, #31797, #37043, .T. ) ;
#33873 = EDGE_CURVE ( 'NONE', #10223, #34949, #2968, .T. ) ;
#33874 = CARTESIAN_POINT ( 'NONE',  ( -16.57554889599778747, -22.21081103083016117, 65.41059783760971413 ) ) ;
#33875 = CARTESIAN_POINT ( 'NONE',  ( -10.55057824423783153, -16.13620093359754293, 71.73133888826306759 ) ) ;
#33876 = CARTESIAN_POINT ( 'NONE',  ( -22.02670722051955465, -15.75340237016373202, 49.52966884056655772 ) ) ;
#33877 = AXIS2_PLACEMENT_3D ( 'NONE', #15155, #30215, #29960 ) ;
#33878 = CARTESIAN_POINT ( 'NONE',  ( -12.90354087724769272, -8.887350501024684490, 67.49447389996370816 ) ) ;
#33879 = ORIENTED_EDGE ( 'NONE', *, *, #15456, .T. ) ;
#33880 = CARTESIAN_POINT ( 'NONE',  ( -11.21157628577468657, -11.58358644131346082, 67.61864608155907774 ) ) ;
#33881 = VERTEX_POINT ( 'NONE', #40408 ) ;
#33882 = CARTESIAN_POINT ( 'NONE',  ( -12.67437386012394640, -9.069420147667823784, 70.98778821476909684 ) ) ;
#33883 = CARTESIAN_POINT ( 'NONE',  ( -17.42409385541299471, -14.80920654474435771, 49.52966884056655772 ) ) ;
#33884 =( BOUNDED_CURVE ( )  B_SPLINE_CURVE ( 3, ( #1068, #31108, #16066, #5017 ),
 .UNSPECIFIED., .F., .F. ) 
 B_SPLINE_CURVE_WITH_KNOTS ( ( 4, 4 ),
 ( 0.000000000000000000, 0.4074455897393629011 ),
 .UNSPECIFIED. ) 
 CURVE ( )  GEOMETRIC_REPRESENTATION_ITEM ( )  RATIONAL_B_SPLINE_CURVE ( ( 1.000000000000000000, 0.4567392136813334669, 0.3561768502900308775, 0.6983129098260921763 ) ) 
 REPRESENTATION_ITEM ( '' )  );
#33885 = CARTESIAN_POINT ( 'NONE',  ( -14.41574869888453136, -7.993524183322376686, 63.83332938139840707 ) ) ;
#33886 = EDGE_LOOP ( 'NONE', ( #5174, #23109, #41783, #39373, #17879 ) ) ;
#33887 = CARTESIAN_POINT ( 'NONE',  ( -21.53994948931798703, -21.01915008201228474, 72.78092378945153484 ) ) ;
#33888 = CIRCLE ( 'NONE', #7945, 5.249999999999998224 ) ;
#33889 = EDGE_CURVE ( 'NONE', #25029, #17399, #32527, .T. ) ;
#33890 = EDGE_CURVE ( 'NONE', #9441, #26904, #18642, .T. ) ;
#33891 = DIRECTION ( 'NONE',  ( -3.071710424422018668E-17, 6.404604876783312462E-16, 1.000000000000000000 ) ) ;
#33892 = VERTEX_POINT ( 'NONE', #47566 ) ;
#33893 = ORIENTED_EDGE ( 'NONE', *, *, #25095, .F. ) ;
#33894 = ORIENTED_EDGE ( 'NONE', *, *, #41120, .F. ) ;
#33895 = CARTESIAN_POINT ( 'NONE',  ( -18.37786432726835883, -21.79469297182707521, 69.10042588711679912 ) ) ;
#33896 = CARTESIAN_POINT ( 'NONE',  ( -18.12273401612753077, -22.22646211661374593, 65.46036745194116691 ) ) ;
#33897 = CIRCLE ( 'NONE', #48025, 2.000000000000000888 ) ;
#33898 = CARTESIAN_POINT ( 'NONE',  ( -12.50897416063251733, -20.40789074996439112, 72.06299591474957822 ) ) ;
#33899 = CARTESIAN_POINT ( 'NONE',  ( -10.58706297158214404, -13.30549792062637593, 74.69434300862685916 ) ) ;
#33900 = CARTESIAN_POINT ( 'NONE',  ( -19.26159385541296487, -7.228003583438021629, 51.38655588711996103 ) ) ;
#33901 = CARTESIAN_POINT ( 'NONE',  ( -14.03871066829747249, -8.172719617054283958, 70.91452941929576070 ) ) ;
#33902 = CARTESIAN_POINT ( 'NONE',  ( -19.28939690137687535, -8.062307696266060475, 59.96092997387292201 ) ) ;
#33903 =( BOUNDED_CURVE ( )  B_SPLINE_CURVE ( 3, ( #16210, #31016, #23641, #5404 ),
 .UNSPECIFIED., .F., .F. ) 
 B_SPLINE_CURVE_WITH_KNOTS ( ( 4, 4 ),
 ( 1.570796326794897002, 1.780235837034216617 ),
 .UNSPECIFIED. ) 
 CURVE ( )  GEOMETRIC_REPRESENTATION_ITEM ( )  RATIONAL_B_SPLINE_CURVE ( ( 1.000000000000000000, 0.9963479302455154896, 0.9963479302455154896, 1.000000000000000000 ) ) 
 REPRESENTATION_ITEM ( '' )  );
#33904 = ORIENTED_EDGE ( 'NONE', *, *, #20607, .T. ) ;
#33905 = ORIENTED_EDGE ( 'NONE', *, *, #7569, .T. ) ;
#33906 = CARTESIAN_POINT ( 'NONE',  ( -12.13107248898915635, -10.22829150951328003, 64.31448999593079918 ) ) ;
#33907 = EDGE_CURVE ( 'NONE', #10902, #35257, #12729, .T. ) ;
#33908 = AXIS2_PLACEMENT_3D ( 'NONE', #34345, #23781, #38534 ) ;
#33909 = CARTESIAN_POINT ( 'NONE',  ( -13.92930047287831741, -8.229585886706207276, 74.36101136741100959 ) ) ;
#33910 = CYLINDRICAL_SURFACE ( 'NONE', #863, 0.1500000000000059897 ) ;
#33911 = CARTESIAN_POINT ( 'NONE',  ( -10.74573065459234478, -12.54952415110468422, 60.81325645027152405 ) ) ;
#33912 = VERTEX_POINT ( 'NONE', #3223 ) ;
#33913 = CARTESIAN_POINT ( 'NONE',  ( -17.01159385650551670, -6.922745924619793101, 51.69366785382590024 ) ) ;
#33914 = EDGE_LOOP ( 'NONE', ( #45010, #41823 ) ) ;
#33915 = AXIS2_PLACEMENT_3D ( 'NONE', #44960, #25487, #26224 ) ;
#33916 = CARTESIAN_POINT ( 'NONE',  ( -14.80056043599933524, -21.78207186541723317, 61.82095768364339960 ) ) ;
#33917 = DIRECTION ( 'NONE',  ( -0.6408936281290997794, -0.7676297007174210929, -4.260501105223894736E-08 ) ) ;
#33918 = CARTESIAN_POINT ( 'NONE',  ( -15.78771722930723875, -7.541141403809244359, 67.29007275881872374 ) ) ;
#33919 = VERTEX_POINT ( 'NONE', #6679 ) ;
#33920 = CARTESIAN_POINT ( 'NONE',  ( -23.46901572703396255, -18.44427995754907457, 69.29371686567111510 ) ) ;
#33921 = VECTOR ( 'NONE', #3088, 1000.000000000000000 ) ;
#33922 = CARTESIAN_POINT ( 'NONE',  ( -10.95467737376780271, -17.63084047650967889, 64.78306623841410783 ) ) ;
#33923 = ORIENTED_EDGE ( 'NONE', *, *, #16982, .T. ) ;
#33924 = VECTOR ( 'NONE', #14800, 1000.000000000000000 ) ;
#33925 = CARTESIAN_POINT ( 'NONE',  ( -23.91010245674826251, -17.57297063409389537, 62.75888927877479517 ) ) ;
#33926 = PLANE ( 'NONE',  #18090 ) ;
#33927 = CARTESIAN_POINT ( 'NONE',  ( -19.42896492416523913, -21.56812594671148275, 61.99503644571810668 ) ) ;
#33928 = VERTEX_POINT ( 'NONE', #37174 ) ;
#33929 = CARTESIAN_POINT ( 'NONE',  ( -24.68106799395027906, -16.49464666695222803, 59.24615566633954700 ) ) ;
#33930 = ORIENTED_EDGE ( 'NONE', *, *, #3655, .F. ) ;
#33931 = LINE ( 'NONE', #45282, #43110 ) ;
#33932 = CARTESIAN_POINT ( 'NONE',  ( -11.55268793888200918, -18.62078556539334073, 64.74707126777444444 ) ) ;
#33933 = ORIENTED_EDGE ( 'NONE', *, *, #38444, .T. ) ;
#33934 = EDGE_CURVE ( 'NONE', #21199, #36781, #13798, .T. ) ;
#33935 = CARTESIAN_POINT ( 'NONE',  ( -12.90227214125716237, -8.888328675545798419, 67.63588728319849963 ) ) ;
#33936 = CARTESIAN_POINT ( 'NONE',  ( -24.51735291603774058, -12.52900075589524498, 69.88587656176791540 ) ) ;
#33937 = VERTEX_POINT ( 'NONE', #25396 ) ;
#33938 = LINE ( 'NONE', #48721, #17269 ) ;
#33939 = CARTESIAN_POINT ( 'NONE',  ( -23.80321451250838649, -17.81075939459467961, 59.00378417737415049 ) ) ;
#33940 = ORIENTED_EDGE ( 'NONE', *, *, #16188, .F. ) ;
#33941 = CYLINDRICAL_SURFACE ( 'NONE', #8228, 0.1500000000000035749 ) ;
#33942 = EDGE_CURVE ( 'NONE', #13213, #15728, #3459, .T. ) ;
#33943 = CARTESIAN_POINT ( 'NONE',  ( -21.76846758817612937, -8.757014937261180521, 70.33143745189734375 ) ) ;
#33944 = AXIS2_PLACEMENT_3D ( 'NONE', #39058, #6305, #5594 ) ;
#33945 = ORIENTED_EDGE ( 'NONE', *, *, #8908, .F. ) ;
#33946 = VERTEX_POINT ( 'NONE', #6451 ) ;
#33947 = EDGE_CURVE ( 'NONE', #31415, #28201, #25425, .T. ) ;
#33948 = AXIS2_PLACEMENT_3D ( 'NONE', #9328, #39357, #35645 ) ;
#33949 = CARTESIAN_POINT ( 'NONE',  ( -10.47299139157196990, -15.63514485490427575, 61.03789045487297926 ) ) ;
#33950 = CARTESIAN_POINT ( 'NONE',  ( -11.79630000206883977, -19.05592701419838519, 71.97213747039440079 ) ) ;
#33951 = CARTESIAN_POINT ( 'NONE',  ( -23.38417127501956116, -19.28035200660907122, 62.54062256979923973 ) ) ;
#33952 = ORIENTED_EDGE ( 'NONE', *, *, #20631, .F. ) ;
#33953 = CARTESIAN_POINT ( 'NONE',  ( -22.80534385650551599, -8.801233750844183135, 48.81488406609782515 ) ) ;
#33954 = ADVANCED_FACE ( 'NONE', ( #6198 ), #32997, .T. ) ;
#33955 = CARTESIAN_POINT ( 'NONE',  ( -10.55500638036946448, -13.20637168857014387, 67.94652154688694168 ) ) ;
#33956 = CARTESIAN_POINT ( 'NONE',  ( -11.59906938467913484, -10.16455840884576389, 71.22539037155303276 ) ) ;
#33957 = CARTESIAN_POINT ( 'NONE',  ( -14.56784385759798894, -9.357632978295830739, 49.97845033065683396 ) ) ;
#33958 = CARTESIAN_POINT ( 'NONE',  ( -9.974987818700082443, -14.92776730449068445, 74.90440581841637879 ) ) ;
#33959 = ORIENTED_EDGE ( 'NONE', *, *, #17688, .T. ) ;
#33960 = LINE ( 'NONE', #15231, #35185 ) ;
#33961 =( NAMED_UNIT ( * ) PLANE_ANGLE_UNIT ( ) SI_UNIT ( $, .RADIAN. ) );
#33962 = CARTESIAN_POINT ( 'NONE',  ( -9.975093145215874202, -14.93635225021824198, 74.98274299234972773 ) ) ;
#33963 = CARTESIAN_POINT ( 'NONE',  ( -13.59121753182073178, -8.949892528329046471, 60.55023482345360719 ) ) ;
#33964 = EDGE_LOOP ( 'NONE', ( #29213, #4621, #32616, #48181, #43138 ) ) ;
#33965 = ORIENTED_EDGE ( 'NONE', *, *, #38381, .T. ) ;
#33966 = CARTESIAN_POINT ( 'NONE',  ( -19.87909365843526643, -21.36461952118570196, 68.96923927572292712 ) ) ;
#33967 = LINE ( 'NONE', #7156, #37852 ) ;
#33968 = LINE ( 'NONE', #738, #28424 ) ;
#33969 = CARTESIAN_POINT ( 'NONE',  ( -8.621879165042305004, -16.10189953769286575, 53.49999999999995026 ) ) ;
#33970 = ORIENTED_EDGE ( 'NONE', *, *, #7226, .F. ) ;
#33971 = CARTESIAN_POINT ( 'NONE',  ( -10.96069643151774109, -18.51437482595545347, 57.92219192461608657 ) ) ;
#33972 = CARTESIAN_POINT ( 'NONE',  ( -14.35241195940507808, -8.021096776717739019, 67.44630344931481147 ) ) ;
#33973 = ORIENTED_EDGE ( 'NONE', *, *, #41849, .F. ) ;
#33974 = CARTESIAN_POINT ( 'NONE',  ( -22.80070500595625660, -9.652102806524988310, 73.52515182072782807 ) ) ;
#33975 = FACE_OUTER_BOUND ( 'NONE', #46196, .T. ) ;
#33976 = CARTESIAN_POINT ( 'NONE',  ( -23.25646303129147441, -19.44570675813884009, 59.07065992548621125 ) ) ;
#33977 = ADVANCED_FACE ( 'NONE', ( #36454 ), #36221, .T. ) ;
#33978 = EDGE_LOOP ( 'NONE', ( #19895, #20272, #29098, #13100, #36913 ) ) ;
#33979 = CARTESIAN_POINT ( 'NONE',  ( -17.47591156279055724, -7.808960447294257534, 67.03656176308530235 ) ) ;
#33980 = ORIENTED_EDGE ( 'NONE', *, *, #43115, .F. ) ;
#33981 = CARTESIAN_POINT ( 'NONE',  ( -22.82985190038863621, -19.93574988146554006, 72.68754644230530459 ) ) ;
#33982 = DIRECTION ( 'NONE',  ( 0.4846961512978548159, 0.8746825943832683414, 4.196010046976494103E-08 ) ) ;
#33983 = VERTEX_POINT ( 'NONE', #41376 ) ;
#33984 = CARTESIAN_POINT ( 'NONE',  ( -13.47433711440449144, -8.491526086692950059, 57.15623147539552917 ) ) ;
#33985 = LINE ( 'NONE', #15260, #10066 ) ;
#33986 = CARTESIAN_POINT ( 'NONE',  ( -20.47409385650551528, -9.792211528768504536, 50.49490371617623197 ) ) ;
#33987 = DIRECTION ( 'NONE',  ( 0.9687793358424821033, -0.2479245821708680464, 0.000000000000000000 ) ) ;
#33988 = DIRECTION ( 'NONE',  ( 0.000000000000000000, 1.000000000000000000, -0.000000000000000000 ) ) ;
#33989 = CARTESIAN_POINT ( 'NONE',  ( -10.51977190731649614, -16.25273689702515156, 68.18587563686374153 ) ) ;
#33990 = DIRECTION ( 'NONE',  ( 3.071710424422018668E-17, -6.404604876783312462E-16, -1.000000000000000000 ) ) ;
#33991 = VERTEX_POINT ( 'NONE', #19221 ) ;
#33992 = CARTESIAN_POINT ( 'NONE',  ( -22.24284385541302456, -7.587656875400178080, 49.25157356644810136 ) ) ;
#33993 = CARTESIAN_POINT ( 'NONE',  ( -15.12009195233319936, -21.89411708065309625, 68.69876018860922784 ) ) ;
#33994 = CARTESIAN_POINT ( 'NONE',  ( -13.33151401730585306, -20.55006798877650454, 58.06122216312902395 ) ) ;
#33995 = CARTESIAN_POINT ( 'NONE',  ( -22.37756982068451705, -20.37394496578614422, 62.34100857704530796 ) ) ;
#33996 = CARTESIAN_POINT ( 'NONE',  ( -18.45552443373157914, -21.73280034295336449, 68.92400672263725880 ) ) ;
#33997 = CARTESIAN_POINT ( 'NONE',  ( -23.77758468005085390, -18.69975821216192813, 72.95706560366770077 ) ) ;
#33998 = ORIENTED_EDGE ( 'NONE', *, *, #13071, .T. ) ;
#33999 = ORIENTED_EDGE ( 'NONE', *, *, #39665, .T. ) ;
#34000 = EDGE_CURVE ( 'NONE', #38039, #19164, #30966, .T. ) ;
#34001 = CARTESIAN_POINT ( 'NONE',  ( -24.02655244371635845, -11.35792869308308717, 66.53719207489109522 ) ) ;
#34002 = CARTESIAN_POINT ( 'NONE',  ( -14.84764829735760649, -8.246537290690364230, 60.33468334944129197 ) ) ;
#34003 = EDGE_LOOP ( 'NONE', ( #17437, #11295 ) ) ;
#34004 = CARTESIAN_POINT ( 'NONE',  ( -12.84615363328625648, -20.17103110633857455, 72.09181604382622766 ) ) ;
#34005 = CARTESIAN_POINT ( 'NONE',  ( -16.31932525666466915, -22.17685042118995398, 61.85593892610445010 ) ) ;
#34006 = DIRECTION ( 'NONE',  ( 8.478320013641884810E-07, -8.009068454735622942E-06, 0.9999999999675679430 ) ) ;
#34007 = EDGE_CURVE ( 'NONE', #39596, #29232, #7671, .T. ) ;
#34008 = CARTESIAN_POINT ( 'NONE',  ( -17.33515904569749466, -7.808492149107161495, 70.71865624139128670 ) ) ;
#34009 = CARTESIAN_POINT ( 'NONE',  ( -21.55686273300884181, -21.00782827186807467, 72.62472190808057348 ) ) ;
#34010 = CARTESIAN_POINT ( 'NONE',  ( -23.58616520728616806, -18.99640775243969060, 66.00884813586510802 ) ) ;
#34011 = DIRECTION ( 'NONE',  ( -3.071710424422018668E-17, 6.404604876783312462E-16, 1.000000000000000000 ) ) ;
#34012 = ADVANCED_FACE ( 'NONE', ( #22676 ), #48709, .T. ) ;
#34013 = CARTESIAN_POINT ( 'NONE',  ( 10.57590614458695377, -0.1092432217106413528, 50.52422457691089619 ) ) ;
#34014 = LINE ( 'NONE', #33766, #28871 ) ;
#34015 = DIRECTION ( 'NONE',  ( -1.000000000000000000, 1.224646799147353207E-16, -3.435970187611875923E-15 ) ) ;
#34016 = FACE_OUTER_BOUND ( 'NONE', #19939, .T. ) ;
#34017 = CARTESIAN_POINT ( 'NONE',  ( -12.11130846069154288, -20.03210741469327871, 61.57395550916974969 ) ) ;
#34018 = CARTESIAN_POINT ( 'NONE',  ( -13.90530646979310525, -20.92243618544410921, 65.19448602716460073 ) ) ;
#34019 = CARTESIAN_POINT ( 'NONE',  ( -21.56784385541339688, -9.357632978298600079, 49.97845033065944875 ) ) ;
#34020 = EDGE_CURVE ( 'NONE', #21415, #16499, #26363, .T. ) ;
#34021 =( BOUNDED_SURFACE ( )  B_SPLINE_SURFACE ( 3, 1, ( 
 ( #25790, #43792 ),
 ( #25071, #7089 ),
 ( #32221, #6355 ),
 ( #47237, #13483 ),
 ( #43554, #21386 ),
 ( #23087, #22849 ),
 ( #15667, #30721 ) ),
 .UNSPECIFIED., .T., .F., .F. ) 
 B_SPLINE_SURFACE_WITH_KNOTS ( ( 4, 3, 4 ),
 ( 2, 2 ),
 ( 0.000000000000000000, 0.5000000000000000000, 1.000000000000000000 ),
 ( 0.000000000000000000, 1.000000000000000000 ),
 .UNSPECIFIED. ) 
 GEOMETRIC_REPRESENTATION_ITEM ( )  RATIONAL_B_SPLINE_SURFACE ( (
 ( 1.000000000000000000, 1.000000000000000000),
 ( 0.3333333333333335369, 0.3333333333333330373),
 ( 0.3333333333333335369, 0.3333333333333330373),
 ( 1.000000000000000000, 1.000000000000000000),
 ( 0.3333333333333333703, 0.3333333333333333703),
 ( 0.3333333333333333703, 0.3333333333333333703),
 ( 1.000000000000000000, 1.000000000000000000) ) ) 
 REPRESENTATION_ITEM ( '' )  SURFACE ( )  );
#34022 = CARTESIAN_POINT ( 'NONE',  ( -24.72409385541305582, -14.80920654474427423, 73.09411764705880898 ) ) ;
#34023 = EDGE_LOOP ( 'NONE', ( #13852, #10396, #34184, #43830 ) ) ;
#34024 = VERTEX_POINT ( 'NONE', #4691 ) ;
#34025 = CARTESIAN_POINT ( 'NONE',  ( -14.64909385541304410, -8.112991634885936776, 51.74999426922421719 ) ) ;
#34026 = ORIENTED_EDGE ( 'NONE', *, *, #10234, .F. ) ;
#34027 = CARTESIAN_POINT ( 'NONE',  ( -23.25534385541299898, -8.623186033802600292, 49.24843789510458691 ) ) ;
#34028 = B_SPLINE_CURVE_WITH_KNOTS ( 'NONE', 3,
 ( #5654, #40336, #20664, #21629, #21397, #35659, #31744, #28037, #43061, #16938 ),
 .UNSPECIFIED., .F., .F.,
 ( 4, 2, 2, 2, 4 ),
 ( 0.6272669072877513630, 0.7522669073072717483, 0.8772669073267922446, 1.002266907346312630, 1.127266907365833015 ),
 .UNSPECIFIED. ) ;
#34029 = CARTESIAN_POINT ( 'NONE',  ( -10.03904583415351581, -13.82694187778184158, 57.56329747881408565 ) ) ;
#34030 =( BOUNDED_CURVE ( )  B_SPLINE_CURVE ( 3, ( #28255, #12747, #24576, #27999 ),
 .UNSPECIFIED., .F., .F. ) 
 B_SPLINE_CURVE_WITH_KNOTS ( ( 4, 4 ),
 ( 0.000000000000000000, 0.4074455897393731707 ),
 .UNSPECIFIED. ) 
 CURVE ( )  GEOMETRIC_REPRESENTATION_ITEM ( )  RATIONAL_B_SPLINE_CURVE ( ( 1.000000000000000000, 0.4567392136813203107, 0.3561768502900259925, 0.6983129098261171563 ) ) 
 REPRESENTATION_ITEM ( '' )  );
#34031 = CARTESIAN_POINT ( 'NONE',  ( -13.62591331635612057, -20.69068061466207453, 65.21458850650557793 ) ) ;
#34032 = CARTESIAN_POINT ( 'NONE',  ( -16.13987559120563731, -22.14769509179112106, 58.48574339058551885 ) ) ;
#34033 = VECTOR ( 'NONE', #45636, 999.9999999999998863 ) ;
#34034 = ORIENTED_EDGE ( 'NONE', *, *, #10297, .F. ) ;
#34035 = CARTESIAN_POINT ( 'NONE',  ( -15.94958553992630002, -7.506453220755747502, 63.84727885063741581 ) ) ;
#34036 = ORIENTED_EDGE ( 'NONE', *, *, #19938, .T. ) ;
#34037 = EDGE_CURVE ( 'NONE', #47981, #31013, #19144, .T. ) ;
#34038 = CYLINDRICAL_SURFACE ( 'NONE', #4726, 4.686499999999997002 ) ;
#34039 =( BOUNDED_SURFACE ( )  B_SPLINE_SURFACE ( 3, 1, ( 
 ( #29392, #33060 ),
 ( #6745, #14818 ),
 ( #26190, #21759 ),
 ( #36745, #48103 ),
 ( #3521, #44424 ),
 ( #7488, #40708 ),
 ( #22003, #37001 ) ),
 .UNSPECIFIED., .T., .F., .F. ) 
 B_SPLINE_SURFACE_WITH_KNOTS ( ( 4, 3, 4 ),
 ( 2, 2 ),
 ( 0.000000000000000000, 0.5000000000000000000, 1.000000000000000000 ),
 ( 0.000000000000000000, 1.000000000000000000 ),
 .UNSPECIFIED. ) 
 GEOMETRIC_REPRESENTATION_ITEM ( )  RATIONAL_B_SPLINE_SURFACE ( (
 ( 1.000000000000000000, 1.000000000000000000),
 ( 0.3333333333333335369, 0.3333333333333330373),
 ( 0.3333333333333335369, 0.3333333333333330373),
 ( 1.000000000000000000, 1.000000000000000000),
 ( 0.3333333333333333703, 0.3333333333333333703),
 ( 0.3333333333333333703, 0.3333333333333333703),
 ( 1.000000000000000000, 1.000000000000000000) ) ) 
 REPRESENTATION_ITEM ( '' )  SURFACE ( )  );
#34040 = ORIENTED_EDGE ( 'NONE', *, *, #28138, .T. ) ;
#34041 = DIRECTION ( 'NONE',  ( -0.7847243476406476903, -0.6198448985189423110, 4.433022207822355740E-08 ) ) ;
#34042 = CARTESIAN_POINT ( 'NONE',  ( -14.07761835836965858, -20.95746660330474143, 72.22607703844037985 ) ) ;
#34043 = CARTESIAN_POINT ( 'NONE',  ( -22.44685545595405785, -12.53547801027385766, 53.69233794759168887 ) ) ;
#34044 = ORIENTED_EDGE ( 'NONE', *, *, #43383, .F. ) ;
#34045 = CARTESIAN_POINT ( 'NONE',  ( -23.25757785049868787, -10.17517560731475967, 63.18690593950643120 ) ) ;
#34046 = FACE_OUTER_BOUND ( 'NONE', #45738, .T. ) ;
#34047 = DIRECTION ( 'NONE',  ( 0.4461977533475104396, 0.8949343913984053600, 0.000000000000000000 ) ) ;
#34048 = CARTESIAN_POINT ( 'NONE',  ( -24.51865387586880729, -12.53305138704347144, 73.42880879726919829 ) ) ;
#34049 = ORIENTED_EDGE ( 'NONE', *, *, #17824, .T. ) ;
#34050 = CARTESIAN_POINT ( 'NONE',  ( -11.75774095458083224, -19.00383931511213120, 71.68685884783836570 ) ) ;
#34051 = CARTESIAN_POINT ( 'NONE',  ( -10.98602742111231478, -11.93616459261413354, 74.85840217524429363 ) ) ;
#34052 = EDGE_CURVE ( 'NONE', #21243, #15104, #45280, .T. ) ;
#34053 = DIRECTION ( 'NONE',  ( 0.000000000000000000, 0.007114381193220285608, -0.9999746924698833528 ) ) ;
#34054 = CARTESIAN_POINT ( 'NONE',  ( -10.38078067960954520, -14.50222210708341741, 68.15800126083217947 ) ) ;
#34055 = CARTESIAN_POINT ( 'NONE',  ( -20.81696448553514855, -20.93198605141084201, 62.41471400679856885 ) ) ;
#34056 = DIRECTION ( 'NONE',  ( 0.9687793358424822143, -0.2479245821708672415, 0.000000000000000000 ) ) ;
#34057 = CARTESIAN_POINT ( 'NONE',  ( -21.56784385650551883, -6.428312510596449592, 51.20221977374900035 ) ) ;
#34058 = ORIENTED_EDGE ( 'NONE', *, *, #32912, .T. ) ;
#34059 = ADVANCED_FACE ( 'NONE', ( #4213 ), #45099, .T. ) ;
#34060 = CARTESIAN_POINT ( 'NONE',  ( -24.68398957063837074, -13.13362340124566785, 63.01919566578877152 ) ) ;
#34061 = CARTESIAN_POINT ( 'NONE',  ( -17.15134030326023051, -7.364115279526828317, 70.67531275522621570 ) ) ;
#34062 = VERTEX_POINT ( 'NONE', #11586 ) ;
#34063 = B_SPLINE_CURVE_WITH_KNOTS ( 'NONE', 1,
 ( #27236, #8524 ),
 .UNSPECIFIED., .F., .F.,
 ( 2, 2 ),
 ( 0.000000000000000000, 1.000000000000000000 ),
 .UNSPECIFIED. ) ;
#34064 = CARTESIAN_POINT ( 'NONE',  ( -18.44824984440512594, -7.884471009248593454, 74.12598989606129862 ) ) ;
#34065 = CARTESIAN_POINT ( 'NONE',  ( -24.45777360974264170, -14.27930545299182619, 73.21451642246609026 ) ) ;
#34066 = CARTESIAN_POINT ( 'NONE',  ( -24.33254494401252188, -16.21558397985894473, 62.59888500697857694 ) ) ;
#34067 = ORIENTED_EDGE ( 'NONE', *, *, #22323, .F. ) ;
#34068 = CARTESIAN_POINT ( 'NONE',  ( -14.78754716229542687, -8.270772359302402066, 60.31996282000579157 ) ) ;
#34069 = CARTESIAN_POINT ( 'NONE',  ( -10.03804196927290882, -15.78895246822652076, 64.69426957934942379 ) ) ;
#34070 = EDGE_CURVE ( 'NONE', #20521, #15515, #3421, .T. ) ;
#34071 = CARTESIAN_POINT ( 'NONE',  ( -10.67174945191680813, -12.96329562009371550, 67.73832382197451807 ) ) ;
#34072 = ORIENTED_EDGE ( 'NONE', *, *, #15513, .T. ) ;
#34073 = CIRCLE ( 'NONE', #15995, 0.5560000000000009379 ) ;
#34074 = CARTESIAN_POINT ( 'NONE',  ( -13.74909385650551563, -8.104110260919579645, 48.81699501597546487 ) ) ;
#34075 = EDGE_CURVE ( 'NONE', #3502, #19604, #11612, .T. ) ;
#34076 = CARTESIAN_POINT ( 'NONE',  ( -20.92409385541305511, -25.10920654474410441, 80.49999999999998579 ) ) ;
#34077 = DIRECTION ( 'NONE',  ( -5.731567514496413899E-31, -1.020425574103664789E-16, -1.000000000000000000 ) ) ;
#34078 = CARTESIAN_POINT ( 'NONE',  ( -17.26457240846633923, -7.760713630915982542, 70.50507891880883449 ) ) ;
#34079 = CARTESIAN_POINT ( 'NONE',  ( -13.59468179584094472, -8.949401161162814589, 56.96967704137573207 ) ) ;
#34080 = ORIENTED_EDGE ( 'NONE', *, *, #13785, .T. ) ;
#34081 = VERTEX_POINT ( 'NONE', #512 ) ;
#34082 = CARTESIAN_POINT ( 'NONE',  ( -13.44284385650551705, -8.811426318492348031, 52.18089403414752070 ) ) ;
#34083 = APPLICATION_CONTEXT ( 'automotive_design' ) ;
#34084 = CARTESIAN_POINT ( 'NONE',  ( -20.13271805750754595, -8.299978134201072777, 70.53628287813307907 ) ) ;
#34085 = DIRECTION ( 'NONE',  ( 0.9687793358424821033, -0.2479245821708677133, 0.000000000000000000 ) ) ;
#34087 = EDGE_CURVE ( 'NONE', #32823, #1260, #14906, .T. ) ;
#34086 = CARTESIAN_POINT ( 'NONE',  ( -15.29909385650551634, -8.114302828567740988, 52.18300498402516041 ) ) ;
#34088 = EDGE_CURVE ( 'NONE', #3266, #5301, #34881, .T. ) ;
#34089 = CARTESIAN_POINT ( 'NONE',  ( -14.97035482569482312, -21.41873484682592377, 61.92128389535452015 ) ) ;
#34090 = EDGE_CURVE ( 'NONE', #33928, #37274, #33732, .T. ) ;
#34091 = FACE_OUTER_BOUND ( 'NONE', #45464, .T. ) ;
#34092 = DIRECTION ( 'NONE',  ( 0.9087012777736581670, -0.4174469879787381932, -4.853707507795077342E-09 ) ) ;
#34093 = CARTESIAN_POINT ( 'NONE',  ( -13.60236376389480384, -20.73382277062339085, 61.80174179654961364 ) ) ;
#34094 = VERTEX_POINT ( 'NONE', #30076 ) ;
#34095 = CARTESIAN_POINT ( 'NONE',  ( -23.03651554467916185, -18.99332579461250603, 62.37023563316526520 ) ) ;
#34096 = EDGE_LOOP ( 'NONE', ( #36396, #2852, #34339, #18181 ) ) ;
#34097 = CARTESIAN_POINT ( 'NONE',  ( -24.06787342886325121, -18.28917680027896608, 53.49999999999994316 ) ) ;
#34098 = DIRECTION ( 'NONE',  ( 0.9687793358424821033, -0.2479245821708677133, 0.000000000000000000 ) ) ;
#34099 = FACE_OUTER_BOUND ( 'NONE', #34297, .T. ) ;
#34100 = CARTESIAN_POINT ( 'NONE',  ( -14.19282086353638661, -8.542981675383003903, 71.01485553001869278 ) ) ;
#34101 = AXIS2_PLACEMENT_3D ( 'NONE', #1850, #6021, #47399 ) ;
#34102 = ORIENTED_EDGE ( 'NONE', *, *, #21303, .F. ) ;
#34103 = CARTESIAN_POINT ( 'NONE',  ( -10.35515617550548306, -17.16373074020370737, 61.34398415755805445 ) ) ;
#34104 = CARTESIAN_POINT ( 'NONE',  ( -24.03160980685186487, -17.26750534774173929, 69.41339792588559021 ) ) ;
#34105 = CARTESIAN_POINT ( 'NONE',  ( -13.15570000409499229, -9.198020586789933617, 67.38502599777598334 ) ) ;
#34106 = CYLINDRICAL_SURFACE ( 'NONE', #22139, 0.5000000000000004441 ) ;
#34107 = VERTEX_POINT ( 'NONE', #11348 ) ;
#34108 = FACE_BOUND ( 'NONE', #37151, .T. ) ;
#34109 = CARTESIAN_POINT ( 'NONE',  ( -17.15134030326023051, -7.364115279526828317, 70.67531275522621570 ) ) ;
#34110 = FACE_OUTER_BOUND ( 'NONE', #2784, .T. ) ;
#34111 = FACE_BOUND ( 'NONE', #18411, .T. ) ;
#34112 = CONTEXT_DEPENDENT_SHAPE_REPRESENTATION ( #19643, #44884 ) ;
#34113 = B_SPLINE_CURVE_WITH_KNOTS ( 'NONE', 1,
 ( #29648, #33557 ),
 .UNSPECIFIED., .F., .F.,
 ( 2, 2 ),
 ( 0.000000000000000000, 1.000000000000000000 ),
 .UNSPECIFIED. ) ;
#34114 = EDGE_LOOP ( 'NONE', ( #1375, #37666, #13992, #27776, #28696 ) ) ;
#34115 = CARTESIAN_POINT ( 'NONE',  ( -10.72530867274958233, -17.00760959713300480, 57.97288447305808745 ) ) ;
#34116 = DIRECTION ( 'NONE',  ( 0.9687793358424821033, -0.2479245821708677133, 0.000000000000000000 ) ) ;
#34117 = CARTESIAN_POINT ( 'NONE',  ( -23.54569203310520464, -19.05535937789667145, 65.93894149164137275 ) ) ;
#34118 = FACE_OUTER_BOUND ( 'NONE', #29337, .T. ) ;
#34119 = ORIENTED_EDGE ( 'NONE', *, *, #1837, .T. ) ;
#34120 = DIRECTION ( 'NONE',  ( 0.1571515419521612722, -0.9875744999047174622, 7.433889655140131751E-08 ) ) ;
#34121 = ORIENTED_EDGE ( 'NONE', *, *, #5266, .T. ) ;
#34122 = CARTESIAN_POINT ( 'NONE',  ( -12.28110100360571444, -10.05819353197068722, 64.21841333961458531 ) ) ;
#34123 = CARTESIAN_POINT ( 'NONE',  ( -15.92409385541305333, -15.80920654474410725, 48.99999999999997868 ) ) ;
#34124 = CARTESIAN_POINT ( 'NONE',  ( -14.99706828511980916, -21.85287925006270626, 65.29092110561946072 ) ) ;
#34125 = VERTEX_POINT ( 'NONE', #32428 ) ;
#34126 = CARTESIAN_POINT ( 'NONE',  ( -13.41327373486474883, -20.54621981236622830, 58.04650078084816300 ) ) ;
#34127 = EDGE_CURVE ( 'NONE', #32748, #27679, #25444, .T. ) ;
#34128 = ORIENTED_EDGE ( 'NONE', *, *, #15946, .F. ) ;
#34129 = ORIENTED_EDGE ( 'NONE', *, *, #22863, .T. ) ;
#34130 = ORIENTED_EDGE ( 'NONE', *, *, #36754, .F. ) ;
#34131 = CARTESIAN_POINT ( 'NONE',  ( -15.40811923343076906, -21.56513327689926030, 72.06047564147742435 ) ) ;
#34132 = B_SPLINE_CURVE_WITH_KNOTS ( 'NONE', 3,
 ( #5727, #43142, #9665, #17262, #13319, #43397, #24679, #39683, #20973, #32305 ),
 .UNSPECIFIED., .F., .F.,
 ( 4, 2, 2, 2, 4 ),
 ( 0.1272669073658627692, 0.2522669073463418843, 0.3772669073268209994, 0.5022669073073000590, 0.6272669072877792296 ),
 .UNSPECIFIED. ) ;
#34133 = LINE ( 'NONE', #3369, #26521 ) ;
#34134 = CARTESIAN_POINT ( 'NONE',  ( -12.64201450438284624, -19.99346662158319887, 72.22142341168820678 ) ) ;
#34135 = DIRECTION ( 'NONE',  ( 1.684279440454093594E-06, -5.535644408139047379E-06, 0.9999999999832598352 ) ) ;
#34136 = CARTESIAN_POINT ( 'NONE',  ( -10.37588343406238067, -17.22313626567787992, 61.33555868484288709 ) ) ;
#34137 = PLANE ( 'NONE',  #10593 ) ;
#34138 = DIRECTION ( 'NONE',  ( -0.3478314405900310713, -0.9375570856950864451, 0.000000000000000000 ) ) ;
#34139 = ORIENTED_EDGE ( 'NONE', *, *, #17312, .F. ) ;
#34140 = ORIENTED_EDGE ( 'NONE', *, *, #31494, .F. ) ;
#34141 = VECTOR ( 'NONE', #19247, 1000.000000000000227 ) ;
#34142 = CARTESIAN_POINT ( 'NONE',  ( -17.92858306677455715, -7.769287621248931686, 63.69489771833700331 ) ) ;
#34143 = CARTESIAN_POINT ( 'NONE',  ( -11.85153772408746065, -9.864590794909398497, 64.22925524624133686 ) ) ;
#34144 = FACE_OUTER_BOUND ( 'NONE', #3680, .T. ) ;
#34145 = CARTESIAN_POINT ( 'NONE',  ( -19.63983784775455987, -21.44940190450812167, 65.46486191127920051 ) ) ;
#34146 = ORIENTED_EDGE ( 'NONE', *, *, #29042, .T. ) ;
#34147 = CARTESIAN_POINT ( 'NONE',  ( -16.56159385650551386, -9.295667164867525756, 49.30633214617472504 ) ) ;
#34148 = ADVANCED_FACE ( 'NONE', ( #47449 ), #6321, .F. ) ;
#34149 = ORIENTED_EDGE ( 'NONE', *, *, #9343, .F. ) ;
#34150 = EDGE_CURVE ( 'NONE', #6133, #43308, #8754, .T. ) ;
#34151 = EDGE_CURVE ( 'NONE', #38159, #36571, #8448, .T. ) ;
#34152 = LINE ( 'NONE', #4609, #21738 ) ;
#34153 = CARTESIAN_POINT ( 'NONE',  ( -12.22456126456390280, -19.57467567670336450, 61.81167242413056329 ) ) ;
#34154 = DIRECTION ( 'NONE',  ( -1.259531062706796257E-05, 2.755480462148206820E-06, -0.9999999999168825981 ) ) ;
#34155 = ORIENTED_EDGE ( 'NONE', *, *, #16484, .T. ) ;
#34156 = CARTESIAN_POINT ( 'NONE',  ( -10.61330258792943226, -12.98832159324075874, 68.03832347271723791 ) ) ;
#34157 = CARTESIAN_POINT ( 'NONE',  ( -11.21783165637758550, -18.93062460193366192, 64.93202459354702683 ) ) ;
#34158 = ORIENTED_EDGE ( 'NONE', *, *, #48193, .T. ) ;
#34159 = CARTESIAN_POINT ( 'NONE',  ( -10.43949455435184603, -13.84896052950683476, 57.46297163929641982 ) ) ;
#34160 =( BOUNDED_CURVE ( )  B_SPLINE_CURVE ( 3, ( #46620, #31830, #1793, #15388 ),
 .UNSPECIFIED., .F., .F. ) 
 B_SPLINE_CURVE_WITH_KNOTS ( ( 4, 4 ),
 ( 0.000000000000000000, 0.4074455897393616244 ),
 .UNSPECIFIED. ) 
 CURVE ( )  GEOMETRIC_REPRESENTATION_ITEM ( )  RATIONAL_B_SPLINE_CURVE ( ( 1.000000000000000000, 0.4567392136813359094, 0.3561768502900317657, 0.6983129098260875134 ) ) 
 REPRESENTATION_ITEM ( '' )  );
#34161 = CARTESIAN_POINT ( 'NONE',  ( -10.04821616988549593, -15.85811384580076933, 64.62276300976363075 ) ) ;
#34162 = FACE_OUTER_BOUND ( 'NONE', #18321, .T. ) ;
#34163 = VERTEX_POINT ( 'NONE', #16482 ) ;
#34164 = CARTESIAN_POINT ( 'NONE',  ( -11.18189852286175956, -11.63857423012741421, 71.31690716596565949 ) ) ;
#34165 = ORIENTED_EDGE ( 'NONE', *, *, #14225, .F. ) ;
#34166 = AXIS2_PLACEMENT_3D ( 'NONE', #30473, #45254, #26038 ) ;
#34167 = CARTESIAN_POINT ( 'NONE',  ( -10.16786014542261007, -13.12079378898483384, 71.25182636653194379 ) ) ;
#34168 = CARTESIAN_POINT ( 'NONE',  ( -14.80072874354800305, -7.836285926156586257, 56.89354091526551116 ) ) ;
#34169 = ORIENTED_EDGE ( 'NONE', *, *, #47741, .F. ) ;
#34170 = CARTESIAN_POINT ( 'NONE',  ( -22.11774618123879677, -15.02177039319221308, 49.52966884056655772 ) ) ;
#34171 = EDGE_CURVE ( 'NONE', #6304, #30207, #17582, .T. ) ;
#34172 = AXIS2_PLACEMENT_3D ( 'NONE', #10878, #44876, #40200 ) ;
#34173 = CARTESIAN_POINT ( 'NONE',  ( -11.08846142298070880, -18.82290330472913098, 54.27966884056657904 ) ) ;
#34174 = ORIENTED_EDGE ( 'NONE', *, *, #36337, .F. ) ;
#34175 = FACE_OUTER_BOUND ( 'NONE', #16817, .T. ) ;
#34176 = CARTESIAN_POINT ( 'NONE',  ( -10.63004074901718532, -12.92571453866564823, 67.75304464120749515 ) ) ;
#34177 = PLANE ( 'NONE',  #10176 ) ;
#34178 = VERTEX_POINT ( 'NONE', #38660 ) ;
#34179 = CARTESIAN_POINT ( 'NONE',  ( -19.17551097150447603, -8.031399452544897954, 63.71472721929436034 ) ) ;
#34180 =( BOUNDED_CURVE ( )  B_SPLINE_CURVE ( 3, ( #42331, #8604, #23867, #34433 ),
 .UNSPECIFIED., .F., .F. ) 
 B_SPLINE_CURVE_WITH_KNOTS ( ( 4, 4 ),
 ( 0.5000000000000000000, 0.9074455897393601811 ),
 .UNSPECIFIED. ) 
 CURVE ( )  GEOMETRIC_REPRESENTATION_ITEM ( )  RATIONAL_B_SPLINE_CURVE ( ( 1.000000000000003331, 0.4567392136813360204, 0.3561768502900293232, 0.6983129098260867362 ) ) 
 REPRESENTATION_ITEM ( '' )  );
#34181 = CARTESIAN_POINT ( 'NONE',  ( -13.19964055691519533, -20.45787379516043814, 58.13830346053801890 ) ) ;
#34182 = ADVANCED_FACE ( 'NONE', ( #13683 ), #1540, .T. ) ;
#34183 = EDGE_LOOP ( 'NONE', ( #4532, #36812, #26613, #12841, #48671 ) ) ;
#34184 = ORIENTED_EDGE ( 'NONE', *, *, #31100, .F. ) ;
#34185 = CARTESIAN_POINT ( 'NONE',  ( -21.91034708787274710, -20.18261625685872218, 59.06442899735736773 ) ) ;
#34186 = DIRECTION ( 'NONE',  ( 1.000000000000000000, 2.866981220435666553E-17, 0.000000000000000000 ) ) ;
#34187 = CARTESIAN_POINT ( 'NONE',  ( -14.41069671968389265, -11.21995593321280182, 52.02966884056656482 ) ) ;
#34188 = PLANE ( 'NONE',  #845 ) ;
#34189 = CARTESIAN_POINT ( 'NONE',  ( -21.17409385650551812, -9.792211528768504536, 50.49490371617623197 ) ) ;
#34190 = LINE ( 'NONE', #38363, #39979 ) ;
#34191 = CARTESIAN_POINT ( 'NONE',  ( -12.01932494161596487, -10.27783711031607261, 71.38381879606350822 ) ) ;
#34192 = CARTESIAN_POINT ( 'NONE',  ( -23.12302852889637350, -18.95946475466559633, 62.65406880579606508 ) ) ;
#34193 = CARTESIAN_POINT ( 'NONE',  ( -12.38096385557255807, -9.882601854136318309, 57.38375773230528409 ) ) ;
#34194 = ORIENTED_EDGE ( 'NONE', *, *, #25081, .F. ) ;
#34195 = CARTESIAN_POINT ( 'NONE',  ( -10.40888601095206134, -14.10966482229656194, 61.21821293885882653 ) ) ;
#34196 = CARTESIAN_POINT ( 'NONE',  ( -10.37541943412130863, -14.96049300415475614, 75.08306784598362071 ) ) ;
#34197 = DIRECTION ( 'NONE',  ( 1.000000000000000000, 2.866981220435666553E-17, 0.000000000000000000 ) ) ;
#34198 = ORIENTED_EDGE ( 'NONE', *, *, #42756, .T. ) ;
#34199 = AXIS2_PLACEMENT_3D ( 'NONE', #31063, #41659, #30835 ) ;
#34200 = EDGE_LOOP ( 'NONE', ( #844, #920 ) ) ;
#34201 = EDGE_CURVE ( 'NONE', #16040, #11402, #45908, .T. ) ;
#34202 = CARTESIAN_POINT ( 'NONE',  ( -19.85890256509918572, -21.37233786973231275, 68.95612130754568625 ) ) ;
#34203 = CARTESIAN_POINT ( 'NONE',  ( -10.61357223164714902, -13.19155561173493219, 71.20828586568362084 ) ) ;
#34204 = B_SPLINE_CURVE_WITH_KNOTS ( 'NONE', 3,
 ( #13362, #32574, #43678, #10180, #21507, #40443, #28410, #36718, #5765, #20770 ),
 .UNSPECIFIED., .F., .F.,
 ( 4, 2, 2, 2, 4 ),
 ( 0.000000000000000000, 0.2500000000000000000, 0.5000000000000000000, 0.7500000000000000000, 1.000000000000000000 ),
 .UNSPECIFIED. ) ;
#34205 = CARTESIAN_POINT ( 'NONE',  ( -11.71852041784209497, -10.01868235693899933, 67.59922621222234795 ) ) ;
#34206 = CARTESIAN_POINT ( 'NONE',  ( -15.04284385541304481, -7.587656875400194068, 49.25157356644814399 ) ) ;
#34207 = EDGE_LOOP ( 'NONE', ( #30681, #9460, #39673, #36159, #47464 ) ) ;
#34208 = CARTESIAN_POINT ( 'NONE',  ( -17.42409385541299471, -14.80920654474435771, 49.52966884056655772 ) ) ;
#34209 = EDGE_CURVE ( 'NONE', #18111, #11672, #19953, .T. ) ;
#34210 = ADVANCED_FACE ( 'NONE', ( #47681 ), #16637, .T. ) ;
#34211 = CARTESIAN_POINT ( 'NONE',  ( -14.28913779072144230, -8.050817036395716997, 67.37479760520351135 ) ) ;
#34212 = VERTEX_POINT ( 'NONE', #42619 ) ;
#34213 = ADVANCED_FACE ( 'NONE', ( #8878 ), #21676, .T. ) ;
#34214 = CARTESIAN_POINT ( 'NONE',  ( -22.92319755143357085, -10.39759026177046763, 63.37185995336191979 ) ) ;
#34215 = EDGE_CURVE ( 'NONE', #39854, #11424, #3855, .T. ) ;
#34216 = CARTESIAN_POINT ( 'NONE',  ( -23.64508914155128139, -11.49223708805166311, 66.72214503450521761 ) ) ;
#34217 = VERTEX_POINT ( 'NONE', #44252 ) ;
#34218 = CARTESIAN_POINT ( 'NONE',  ( -11.65643154663995595, -18.86968838501740109, 64.95526796013899684 ) ) ;
#34219 = VERTEX_POINT ( 'NONE', #15145 ) ;
#34220 = DIRECTION ( 'NONE',  ( 1.000000000000000000, 0.000000000000000000, 0.000000000000000000 ) ) ;
#34221 = B_SPLINE_CURVE_WITH_KNOTS ( 'NONE', 3,
 ( #40389, #47776, #10118, #28594, #14016, #9878, #17247, #29067, #29309, #24896 ),
 .UNSPECIFIED., .F., .F.,
 ( 4, 2, 2, 2, 4 ),
 ( 0.6272669072878390706, 0.7522669073073260382, 0.8772669073268131168, 1.002266907346299973, 1.127266907365787052 ),
 .UNSPECIFIED. ) ;
#34222 = CARTESIAN_POINT ( 'NONE',  ( -20.40573040493966772, -8.475905570818413892, 63.53794860803412092 ) ) ;
#34223 = ORIENTED_EDGE ( 'NONE', *, *, #32287, .F. ) ;
#34224 = DIRECTION ( 'NONE',  ( 0.7300417127692488961, 0.6834025882427879894, 6.612978994660554254E-09 ) ) ;
#34225 = DIRECTION ( 'NONE',  ( -3.413470714839332458E-33, 1.190614954331866791E-16, -1.000000000000000000 ) ) ;
#34226 = EDGE_CURVE ( 'NONE', #20348, #13463, #6739, .T. ) ;
#34227 = CARTESIAN_POINT ( 'NONE',  ( -21.76784385650551457, -6.428312510596451368, 51.20221977374900035 ) ) ;
#34228 = CARTESIAN_POINT ( 'NONE',  ( -22.66727108289645543, -10.09628893573625064, 70.01178520457129650 ) ) ;
#34229 = CARTESIAN_POINT ( 'NONE',  ( -19.17247957453286844, -7.567181637230756763, 63.61584517348745038 ) ) ;
#34230 = CARTESIAN_POINT ( 'NONE',  ( -17.21153000696512336, -19.50285887057015444, 49.52966884056656482 ) ) ;
#34231 = ORIENTED_EDGE ( 'NONE', *, *, #33, .T. ) ;
#34232 = CARTESIAN_POINT ( 'NONE',  ( -15.22116837037893866, -21.50650591823945845, 68.59065000974109694 ) ) ;
#34233 = DIRECTION ( 'NONE',  ( -5.731567514496413899E-31, -1.020425574103664789E-16, -1.000000000000000000 ) ) ;
#34234 = AXIS2_PLACEMENT_3D ( 'NONE', #4300, #23258, #34564 ) ;
#34235 = CARTESIAN_POINT ( 'NONE',  ( -45.92409385541306222, -14.80920654474410725, 70.50000000000000000 ) ) ;
#34236 = CARTESIAN_POINT ( 'NONE',  ( -24.63822977646513834, -12.69227384653554047, 54.02312124697525064 ) ) ;
#34237 = CARTESIAN_POINT ( 'NONE',  ( -16.06904075904983031, -7.890656793283918446, 63.97011029956862416 ) ) ;
#34238 = ORIENTED_EDGE ( 'NONE', *, *, #39179, .T. ) ;
#34239 = ORIENTED_EDGE ( 'NONE', *, *, #15939, .T. ) ;
#34240 = CARTESIAN_POINT ( 'NONE',  ( -24.49361813620984663, -12.45866096502549603, 73.43563874794485002 ) ) ;
#34241 = CARTESIAN_POINT ( 'NONE',  ( -14.73594855369633905, -7.860282982240396343, 60.50651534380390473 ) ) ;
#34242 = VERTEX_POINT ( 'NONE', #10737 ) ;
#34243 = CARTESIAN_POINT ( 'NONE',  ( -12.83178440107774065, -20.15853244757020590, 72.10093902957984824 ) ) ;
#34244 = CARTESIAN_POINT ( 'NONE',  ( -15.75283589881223278, -7.548994832054173543, 67.32502661251716347 ) ) ;
#34245 = CARTESIAN_POINT ( 'NONE',  ( -21.14909385759798965, -8.112991634885936776, 51.74999426922421719 ) ) ;
#34246 = CARTESIAN_POINT ( 'NONE',  ( -13.90805003106573068, -20.86209311441256986, 68.75625137331327608 ) ) ;
#34247 = B_SPLINE_CURVE_WITH_KNOTS ( 'NONE', 1,
 ( #28456, #24992 ),
 .UNSPECIFIED., .F., .F.,
 ( 2, 2 ),
 ( 0.000000000000000000, 1.000000000000000000 ),
 .UNSPECIFIED. ) ;
#34248 = CARTESIAN_POINT ( 'NONE',  ( -12.05615918852498680, -19.97535170061420828, 61.51183199568394144 ) ) ;
#34249 = CARTESIAN_POINT ( 'NONE',  ( -18.50162202296811742, -21.72577595440482057, 72.28510940981611554 ) ) ;
#34250 = CARTESIAN_POINT ( 'NONE',  ( -20.34472269902922292, -8.388554739717058339, 63.31121412747268096 ) ) ;
#34251 = PRODUCT_DEFINITION_SHAPE ( 'NONE', 'NONE',  #48741 ) ;
#34252 = CARTESIAN_POINT ( 'NONE',  ( 8.575906144586950219, 2.110465741754207425, 60.53099189295826221 ) ) ;
#34253 =( NAMED_UNIT ( * ) SI_UNIT ( $, .STERADIAN. ) SOLID_ANGLE_UNIT ( ) );
#34254 = CARTESIAN_POINT ( 'NONE',  ( -10.51205449915416068, -13.40259651842557531, 71.20828329199629536 ) ) ;
#34255 =( BOUNDED_CURVE ( )  B_SPLINE_CURVE ( 3, ( #35769, #13359, #10174, #17298 ),
 .UNSPECIFIED., .F., .F. ) 
 B_SPLINE_CURVE_WITH_KNOTS ( ( 4, 4 ),
 ( 0.5000000000000000000, 0.9074455897393680637 ),
 .UNSPECIFIED. ) 
 CURVE ( )  GEOMETRIC_REPRESENTATION_ITEM ( )  RATIONAL_B_SPLINE_CURVE ( ( 1.000000000000016653, 0.4567392136813376302, 0.3561768502900207745, 0.6983129098260839607 ) ) 
 REPRESENTATION_ITEM ( '' )  );
#34256 = CARTESIAN_POINT ( 'NONE',  ( -13.90804716676048258, -20.86209139562971160, 68.45625137333186672 ) ) ;
#34257 = CARTESIAN_POINT ( 'NONE',  ( -12.87649578556737318, -13.67667219862660843, 52.02966884056656482 ) ) ;
#34258 = EDGE_CURVE ( 'NONE', #14388, #467, #45102, .T. ) ;
#34259 = CYLINDRICAL_SURFACE ( 'NONE', #42567, 5.000000000000001776 ) ;
#34260 = VERTEX_POINT ( 'NONE', #33868 ) ;
#34261 = EDGE_LOOP ( 'NONE', ( #10078, #27334, #3014, #36430, #19 ) ) ;
#34262 = CARTESIAN_POINT ( 'NONE',  ( -22.46784385650551741, -6.428312510596450480, 51.20221977374900035 ) ) ;
#34263 = EDGE_LOOP ( 'NONE', ( #28966, #38150, #7104, #6319 ) ) ;
#34264 = ADVANCED_FACE ( 'NONE', ( #14636 ), #48651, .T. ) ;
#34265 = CARTESIAN_POINT ( 'NONE',  ( -46.92409385541305511, -17.80920654474410370, 61.49999999999999289 ) ) ;
#34266 = CARTESIAN_POINT ( 'NONE',  ( -16.47526054104836746, -21.74466271362331682, 61.77070513569444188 ) ) ;
#34267 = VECTOR ( 'NONE', #31373, 1000.000000000000000 ) ;
#34268 = CARTESIAN_POINT ( 'NONE',  ( -13.34343926350448584, -8.575967577738570213, 57.13001076993559479 ) ) ;
#34269 = CARTESIAN_POINT ( 'NONE',  ( -16.77411572588129118, -21.83219480353551134, 72.58031927177887610 ) ) ;
#34270 = ORIENTED_EDGE ( 'NONE', *, *, #36550, .F. ) ;
#34271 = EDGE_CURVE ( 'NONE', #1779, #12574, #46077, .T. ) ;
#34272 = CARTESIAN_POINT ( 'NONE',  ( -13.83248983650026709, -21.33638410845934885, 72.18253639678975730 ) ) ;
#34273 = CARTESIAN_POINT ( 'NONE',  ( -17.55282127470103504, -7.360150197541120320, 63.71090416642158516 ) ) ;
#34274 = EDGE_CURVE ( 'NONE', #2663, #25694, #41027, .T. ) ;
#34275 = ORIENTED_EDGE ( 'NONE', *, *, #26167, .F. ) ;
#34276 = CARTESIAN_POINT ( 'NONE',  ( -11.96084830514426400, -9.743959610980004626, 60.74413522332266524 ) ) ;
#34277 = B_SPLINE_CURVE_WITH_KNOTS ( 'NONE', 1,
 ( #38477, #19048 ),
 .UNSPECIFIED., .F., .F.,
 ( 2, 2 ),
 ( 0.000000000000000000, 1.000000000000000000 ),
 .UNSPECIFIED. ) ;
#34278 = CARTESIAN_POINT ( 'NONE',  ( -10.37497030826117417, -14.69804335084345759, 71.32782692816427073 ) ) ;
#34279 = ORIENTED_EDGE ( 'NONE', *, *, #27008, .T. ) ;
#34280 = EDGE_CURVE ( 'NONE', #9420, #40683, #2616, .T. ) ;
#34281 = CARTESIAN_POINT ( 'NONE',  ( -24.47498361611929596, -14.63661054434306763, 59.12811639263489383 ) ) ;
#34282 = CARTESIAN_POINT ( 'NONE',  ( -21.36420383812641077, -21.13211724076752773, 69.31096130815059553 ) ) ;
#34283 = CARTESIAN_POINT ( 'NONE',  ( -17.85261197751258067, -25.23011165689956670, 54.58422952202461431 ) ) ;
#34284 = VERTEX_POINT ( 'NONE', #37302 ) ;
#34285 = CARTESIAN_POINT ( 'NONE',  ( -23.20384594580217552, -10.10819856274111039, 63.23219334867470565 ) ) ;
#34286 = LINE ( 'NONE', #8215, #24978 ) ;
#34287 = EDGE_CURVE ( 'NONE', #16467, #46532, #42105, .T. ) ;
#34288 = CARTESIAN_POINT ( 'NONE',  ( -14.54176566789882585, -21.67913831930545854, 58.28122448549703449 ) ) ;
#34289 = CARTESIAN_POINT ( 'NONE',  ( -21.06702863216100141, -20.84540773593991148, 65.86981821684420879 ) ) ;
#34290 = ORIENTED_EDGE ( 'NONE', *, *, #20587, .T. ) ;
#34291 = CARTESIAN_POINT ( 'NONE',  ( -15.75283589881223278, -7.548994832054173543, 67.32502661251716347 ) ) ;
#34292 = FACE_OUTER_BOUND ( 'NONE', #21459, .T. ) ;
#34293 = CARTESIAN_POINT ( 'NONE',  ( -22.07864594086649390, -14.26292169798353981, 49.52966884056655772 ) ) ;
#34294 = DIRECTION ( 'NONE',  ( 1.190035119058586791E-06, 1.172070126139376962E-06, 0.9999999999986050048 ) ) ;
#34295 = PLANE ( 'NONE',  #41704 ) ;
#34296 = CARTESIAN_POINT ( 'NONE',  ( -19.82409385650551670, -6.426201560718813433, 50.50509628382439331 ) ) ;
#34297 = EDGE_LOOP ( 'NONE', ( #29224, #3649, #34861, #46824 ) ) ;
#34298 = CARTESIAN_POINT ( 'NONE',  ( -24.05059659118241555, -17.06519001246171996, 72.88336032079776317 ) ) ;
#34299 = ORIENTED_EDGE ( 'NONE', *, *, #15208, .F. ) ;
#34300 = CYLINDRICAL_SURFACE ( 'NONE', #44183, 0.1499999999999992173 ) ;
#34301 = CARTESIAN_POINT ( 'NONE',  ( -22.98865682493615381, -9.855478938366896813, 70.12683207277369490 ) ) ;
#34302 = CARTESIAN_POINT ( 'NONE',  ( -14.60831023476407786, -21.21965601727942996, 58.35544853774701579 ) ) ;
#34303 =( BOUNDED_CURVE ( )  B_SPLINE_CURVE ( 3, ( #48347, #3298, #18545, #18297 ),
 .UNSPECIFIED., .F., .F. ) 
 B_SPLINE_CURVE_WITH_KNOTS ( ( 4, 4 ),
 ( 1.570796326794896558, 1.780235837034217727 ),
 .UNSPECIFIED. ) 
 CURVE ( )  GEOMETRIC_REPRESENTATION_ITEM ( )  RATIONAL_B_SPLINE_CURVE ( ( 1.000000000000000000, 0.9963479302455154896, 0.9963479302455154896, 1.000000000000000000 ) ) 
 REPRESENTATION_ITEM ( '' )  );
#34304 = EDGE_LOOP ( 'NONE', ( #22337, #3656, #1486, #46421, #36645 ) ) ;
#34305 = CARTESIAN_POINT ( 'NONE',  ( -18.39951258112534305, -22.19516185762106275, 69.00009993223443416 ) ) ;
#34306 = AXIS2_PLACEMENT_3D ( 'NONE', #18921, #48712, #7120 ) ;
#34307 = CARTESIAN_POINT ( 'NONE',  ( -46.47622156840087371, -14.20920654474410760, 70.13000000000000966 ) ) ;
#34308 = CARTESIAN_POINT ( 'NONE',  ( -23.47609061619699844, -18.32690069530191579, 72.83656187062067033 ) ) ;
#34309 = ORIENTED_EDGE ( 'NONE', *, *, #36837, .T. ) ;
#34310 = CARTESIAN_POINT ( 'NONE',  ( -16.05534385650551243, -7.417179338643134834, 52.18511593390279302 ) ) ;
#34311 = DIRECTION ( 'NONE',  ( 1.000000000000000000, 0.000000000000000000, 0.000000000000000000 ) ) ;
#34312 = CARTESIAN_POINT ( 'NONE',  ( -36.42409385541304800, -8.109206544743658540, 50.50000000000030553 ) ) ;
#34313 = EDGE_CURVE ( 'NONE', #17093, #33155, #1399, .T. ) ;
#34314 = CARTESIAN_POINT ( 'NONE',  ( -14.09575362490740602, -8.143965183153959231, 70.83683468466919919 ) ) ;
#34315 = CARTESIAN_POINT ( 'NONE',  ( -13.50402399543905929, -9.009805505539487669, 57.16070831537086860 ) ) ;
#34316 = B_SPLINE_CURVE_WITH_KNOTS ( 'NONE', 3,
 ( #35658, #1938, #23879, #38882, #31743, #5160, #24841, #35177, #46763, #16937 ),
 .UNSPECIFIED., .F., .F.,
 ( 4, 2, 2, 2, 4 ),
 ( 0.000000000000000000, 0.2500000000000000000, 0.5000000000000000000, 0.7500000000000000000, 1.000000000000000000 ),
 .UNSPECIFIED. ) ;
#34317 =( BOUNDED_CURVE ( )  B_SPLINE_CURVE ( 3, ( #28991, #32683, #13475, #13223 ),
 .UNSPECIFIED., .F., .F. ) 
 B_SPLINE_CURVE_WITH_KNOTS ( ( 4, 4 ),
 ( 0.5000000000000000000, 0.9074455897393649551 ),
 .UNSPECIFIED. ) 
 CURVE ( )  GEOMETRIC_REPRESENTATION_ITEM ( )  RATIONAL_B_SPLINE_CURVE ( ( 1.000000000000004441, 0.4567392136813354098, 0.3561768502900284350, 0.6983129098260884016 ) ) 
 REPRESENTATION_ITEM ( '' )  );
#34318 = ORIENTED_EDGE ( 'NONE', *, *, #14465, .F. ) ;
#34319 = ORIENTED_EDGE ( 'NONE', *, *, #13591, .F. ) ;
#34320 = CARTESIAN_POINT ( 'NONE',  ( -14.56784385650551528, -6.428312510596451368, 51.20221977374900035 ) ) ;
#34321 = CARTESIAN_POINT ( 'NONE',  ( -22.99375746295947209, -9.861153455744265273, 70.13461618218333626 ) ) ;
#34322 = CARTESIAN_POINT ( 'NONE',  ( -23.81024829756716343, -18.64597716098235836, 72.94863620959463901 ) ) ;
#34323 = CARTESIAN_POINT ( 'NONE',  ( -15.74909385650551386, -8.104110260919579645, 48.81699501597546487 ) ) ;
#34324 =( BOUNDED_CURVE ( )  B_SPLINE_CURVE ( 3, ( #17852, #28953, #6312, #32874 ),
 .UNSPECIFIED., .F., .F. ) 
 B_SPLINE_CURVE_WITH_KNOTS ( ( 4, 4 ),
 ( 0.5000000000000000000, 0.9074455897393627346 ),
 .UNSPECIFIED. ) 
 CURVE ( )  GEOMETRIC_REPRESENTATION_ITEM ( )  RATIONAL_B_SPLINE_CURVE ( ( 1.000000000000033973, 0.4567392136813449577, 0.3561768502900111155, 0.6983129098260696388 ) ) 
 REPRESENTATION_ITEM ( '' )  );
#34325 = FACE_OUTER_BOUND ( 'NONE', #23255, .T. ) ;
#34326 = CARTESIAN_POINT ( 'NONE',  ( -20.48833060507423909, -8.513735687714852673, 66.89177111435644463 ) ) ;
#34327 = EDGE_CURVE ( 'NONE', #43290, #7311, #19844, .T. ) ;
#34328 = CARTESIAN_POINT ( 'NONE',  ( -9.982647249627337516, -14.45068338159927990, 68.11446040317247252 ) ) ;
#34329 = DIRECTION ( 'NONE',  ( -3.071710424422018668E-17, 6.404604876783312462E-16, 1.000000000000000000 ) ) ;
#34330 = EDGE_CURVE ( 'NONE', #28874, #44341, #10828, .T. ) ;
#34331 = ORIENTED_EDGE ( 'NONE', *, *, #36696, .F. ) ;
#34332 = AXIS2_PLACEMENT_3D ( 'NONE', #27541, #39100, #1684 ) ;
#34333 = ORIENTED_EDGE ( 'NONE', *, *, #7514, .F. ) ;
#34334 = ADVANCED_FACE ( 'NONE', ( #8768 ), #30476, .T. ) ;
#34335 = CARTESIAN_POINT ( 'NONE',  ( -13.00647906721701297, -9.304695462141918227, 64.06513368409466125 ) ) ;
#34336 = CARTESIAN_POINT ( 'NONE',  ( -9.974999579213063683, -14.92872621805817879, 74.99053041033617717 ) ) ;
#34337 = CARTESIAN_POINT ( 'NONE',  ( -12.57425161569036653, -9.153915111069411026, 74.42648864573870071 ) ) ;
#34338 = CARTESIAN_POINT ( 'NONE',  ( -13.27770465421436619, -9.107456272842560097, 64.20946529204060482 ) ) ;
#34339 = ORIENTED_EDGE ( 'NONE', *, *, #6886, .T. ) ;
#34340 = CARTESIAN_POINT ( 'NONE',  ( -10.74573065459234478, -12.54952415110468422, 60.81325645027152405 ) ) ;
#34341 = CARTESIAN_POINT ( 'NONE',  ( -10.78031428196279329, -11.32923628920978487, 47.99999999999994316 ) ) ;
#34342 = EDGE_CURVE ( 'NONE', #29174, #19773, #27222, .T. ) ;
#34343 = VECTOR ( 'NONE', #8035, 1000.000000000000000 ) ;
#34344 = CARTESIAN_POINT ( 'NONE',  ( -10.32984062102020850, -12.53399622812623448, 60.95886941719668073 ) ) ;
#34345 = CARTESIAN_POINT ( 'NONE',  ( -45.92409385541305511, -17.80920654474410370, 70.50000000000000000 ) ) ;
#34346 = ORIENTED_EDGE ( 'NONE', *, *, #8322, .F. ) ;
#34347 = DIRECTION ( 'NONE',  ( -0.3739781583979218671, -0.9274375111247652459, -6.296758467538797382E-09 ) ) ;
#34348 = PLANE ( 'NONE',  #18722 ) ;
#34349 = DIRECTION ( 'NONE',  ( 0.000000000000000000, 1.000000000000000000, -0.000000000000000000 ) ) ;
#34350 = FACE_BOUND ( 'NONE', #16665, .T. ) ;
#34351 = ORIENTED_EDGE ( 'NONE', *, *, #44845, .F. ) ;
#34352 = CARTESIAN_POINT ( 'NONE',  ( -22.17032154447610282, -19.95442984834653188, 62.34325199807766182 ) ) ;
#34353 = CARTESIAN_POINT ( 'NONE',  ( -18.11889201384288128, -21.82488578508536747, 65.34532159284481168 ) ) ;
#34354 = CARTESIAN_POINT ( 'NONE',  ( -23.50612575731066656, -19.11299006986292071, 66.01044822673141255 ) ) ;
#34355 = CARTESIAN_POINT ( 'NONE',  ( -15.73993337224566247, -7.955115359200574332, 63.82577855974437853 ) ) ;
#34356 = ORIENTED_EDGE ( 'NONE', *, *, #31434, .F. ) ;
#34357 = PLANE ( 'NONE',  #2429 ) ;
#34358 = VERTEX_POINT ( 'NONE', #15885 ) ;
#34359 = PLANE ( 'NONE',  #25038 ) ;
#34360 = CARTESIAN_POINT ( 'NONE',  ( -20.03282965983824226, -21.84088468745754597, 77.49999999999994316 ) ) ;
#34361 = ADVANCED_FACE ( 'NONE', ( #15382 ), #4335, .T. ) ;
#34362 = VERTEX_POINT ( 'NONE', #38047 ) ;
#34363 = EDGE_CURVE ( 'NONE', #25136, #25847, #22302, .T. ) ;
#34364 = CARTESIAN_POINT ( 'NONE',  ( -23.07130679197163659, -10.58859284808890422, 59.60763246093404177 ) ) ;
#34365 = ORIENTED_EDGE ( 'NONE', *, *, #3073, .T. ) ;
#34366 = EDGE_CURVE ( 'NONE', #1168, #25404, #38538, .T. ) ;
#34367 = VERTEX_POINT ( 'NONE', #12438 ) ;
#34368 = ORIENTED_EDGE ( 'NONE', *, *, #36048, .T. ) ;
#34369 = CARTESIAN_POINT ( 'NONE',  ( -20.63628304827270199, -8.086446354347476273, 66.96759359044023086 ) ) ;
#34370 = EDGE_CURVE ( 'NONE', #25725, #15450, #2681, .T. ) ;
#34371 = CARTESIAN_POINT ( 'NONE',  ( -21.21817610565444667, -20.69187580328668119, 69.33984775460822902 ) ) ;
#34372 = CARTESIAN_POINT ( 'NONE',  ( -15.56465948913147557, -7.543361525925788236, 54.27966884056655061 ) ) ;
#34373 = CARTESIAN_POINT ( 'NONE',  ( -24.13123319531394273, -12.80563922725783144, 66.49349849057904294 ) ) ;
#34374 = CARTESIAN_POINT ( 'NONE',  ( -12.68381388925888587, -19.95990997655619381, 68.63657438305759229 ) ) ;
#34375 = CARTESIAN_POINT ( 'NONE',  ( -22.37499513144005903, -19.83249348569362880, 73.05889139438880875 ) ) ;
#34376 = VECTOR ( 'NONE', #1025, 1000.000000000000114 ) ;
#34377 = AXIS2_PLACEMENT_3D ( 'NONE', #26181, #19511, #325 ) ;
#34378 = ORIENTED_EDGE ( 'NONE', *, *, #16423, .T. ) ;
#34379 = ORIENTED_EDGE ( 'NONE', *, *, #43969, .F. ) ;
#34380 = CARTESIAN_POINT ( 'NONE',  ( -12.15425132636677219, -10.20155252404504331, 64.02914322084043874 ) ) ;
#34381 = CARTESIAN_POINT ( 'NONE',  ( -14.09463846823036981, -8.088735815341543400, 53.49999999999994316 ) ) ;
#34382 = FACE_OUTER_BOUND ( 'NONE', #37105, .T. ) ;
#34383 = AXIS2_PLACEMENT_3D ( 'NONE', #37288, #3573, #7532 ) ;
#34384 = DIRECTION ( 'NONE',  ( 3.071710424422018668E-17, -6.404604876783312462E-16, -1.000000000000000000 ) ) ;
#34385 = ORIENTED_EDGE ( 'NONE', *, *, #33812, .T. ) ;
#34386 = CARTESIAN_POINT ( 'NONE',  ( -17.23659385650551812, -6.915538690918074494, 49.31353937987644542 ) ) ;
#34387 = EDGE_LOOP ( 'NONE', ( #21751, #13646, #22000, #5689, #30556 ) ) ;
#34388 = CARTESIAN_POINT ( 'NONE',  ( -11.75774308769439003, -19.00384223356172697, 71.98685884781657762 ) ) ;
#34389 = CARTESIAN_POINT ( 'NONE',  ( -10.50429924535250414, -16.15944446069506668, 71.46222527016213633 ) ) ;
#34390 = CARTESIAN_POINT ( 'NONE',  ( -10.40511033146429831, -14.11732416830307280, 57.33336190745325212 ) ) ;
#34391 = ORIENTED_EDGE ( 'NONE', *, *, #44535, .F. ) ;
#34392 = EDGE_CURVE ( 'NONE', #31657, #27248, #27706, .T. ) ;
#34393 = PLANE ( 'NONE',  #13839 ) ;
#34394 = CARTESIAN_POINT ( 'NONE',  ( -24.17607580446128068, -11.66038665607651836, 59.60422999760712059 ) ) ;
#34395 = ADVANCED_FACE ( 'NONE', ( #37809 ), #19340, .T. ) ;
#34396 = EDGE_LOOP ( 'NONE', ( #14726, #44619 ) ) ;
#34397 = CARTESIAN_POINT ( 'NONE',  ( -24.47368665962210343, -14.70950332193510590, 62.72768537250228604 ) ) ;
#34398 = DIRECTION ( 'NONE',  ( 0.9687793358424817702, -0.2479245821708684905, 0.000000000000000000 ) ) ;
#34399 = CARTESIAN_POINT ( 'NONE',  ( -15.56465948913149155, -7.543361525925791788, 54.27966884056655061 ) ) ;
#34400 = VERTEX_POINT ( 'NONE', #30689 ) ;
#34401 = CARTESIAN_POINT ( 'NONE',  ( -11.15769924256992951, -11.68856090084249999, 71.37244301326146001 ) ) ;
#34402 = AXIS2_PLACEMENT_3D ( 'NONE', #21412, #36877, #17201 ) ;
#34403 = CIRCLE ( 'NONE', #29714, 5.249999999999998224 ) ;
#34404 = ORIENTED_EDGE ( 'NONE', *, *, #41291, .T. ) ;
#34405 = CARTESIAN_POINT ( 'NONE',  ( -10.16749015965427105, -13.12235144340169235, 71.39323866028058774 ) ) ;
#34406 = CARTESIAN_POINT ( 'NONE',  ( -24.38111619087839799, -15.96880572012975286, 62.47839786477943136 ) ) ;
#34407 = ORIENTED_EDGE ( 'NONE', *, *, #43829, .F. ) ;
#34408 = DIRECTION ( 'NONE',  ( -0.9998756790481366785, -0.01576789294826319923, -3.907472230461692677E-09 ) ) ;
#34409 = CARTESIAN_POINT ( 'NONE',  ( -24.53780083649505173, -12.59584922708229904, 69.95738295622972203 ) ) ;
#34410 = LINE ( 'NONE', #12503, #39129 ) ;
#34411 = EDGE_LOOP ( 'NONE', ( #9330, #30127, #9995, #10133, #23316 ) ) ;
#34412 = DIRECTION ( 'NONE',  ( -0.1186632576870824130, 0.9929345553837299887, 6.051931679537041823E-08 ) ) ;
#34413 = AXIS2_PLACEMENT_3D ( 'NONE', #44921, #15322, #19042 ) ;
#34414 = CARTESIAN_POINT ( 'NONE',  ( -10.67239429020883890, -12.76729606296974140, 68.03832549181448996 ) ) ;
#34415 = CARTESIAN_POINT ( 'NONE',  ( -10.93882906647579922, -17.44414160026099125, 68.39721938813583790 ) ) ;
#34416 = ORIENTED_EDGE ( 'NONE', *, *, #33265, .F. ) ;
#34417 = CARTESIAN_POINT ( 'NONE',  ( -22.97409385650551528, -9.792211528768504536, 50.49490371617623197 ) ) ;
#34418 = ADVANCED_FACE ( 'NONE', ( #34110 ), #41765, .T. ) ;
#34419 = CARTESIAN_POINT ( 'NONE',  ( -23.58390325158506329, -11.37972522600045089, 69.89770551021980793 ) ) ;
#34420 = EDGE_CURVE ( 'NONE', #10683, #19164, #15637, .T. ) ;
#34421 = ADVANCED_FACE ( 'NONE', ( #24753 ), #16917, .T. ) ;
#34422 = EDGE_CURVE ( 'NONE', #43983, #1692, #32134, .T. ) ;
#34423 = VERTEX_POINT ( 'NONE', #43222 ) ;
#34424 = ORIENTED_EDGE ( 'NONE', *, *, #12866, .F. ) ;
#34425 = CARTESIAN_POINT ( 'NONE',  ( -19.80886856394220175, -10.13209743873031954, 52.02966884056656482 ) ) ;
#34426 = CARTESIAN_POINT ( 'NONE',  ( -22.09287085128708839, -15.21639644245407297, 49.52966884056655772 ) ) ;
#34427 = FACE_OUTER_BOUND ( 'NONE', #42534, .T. ) ;
#34428 = CARTESIAN_POINT ( 'NONE',  ( -20.55534385650551599, -7.417179338643134834, 52.18511593390279302 ) ) ;
#34429 = CARTESIAN_POINT ( 'NONE',  ( -10.55421158500719336, -13.20934456994658035, 67.73832145363171264 ) ) ;
#34430 = B_SPLINE_CURVE_WITH_KNOTS ( 'NONE', 3,
 ( #8872, #35670, #16474, #39134, #34718, #1953, #1461, #43076, #47010, #38653 ),
 .UNSPECIFIED., .F., .F.,
 ( 4, 2, 2, 2, 4 ),
 ( 0.000000000000000000, 0.2500000000000000000, 0.5000000000000000000, 0.7500000000000000000, 1.000000000000000000 ),
 .UNSPECIFIED. ) ;
#34431 = LINE ( 'NONE', #30531, #18889 ) ;
#34432 = DIRECTION ( 'NONE',  ( -3.071710424422018668E-17, 6.404604876783312462E-16, 1.000000000000000000 ) ) ;
#34433 = CARTESIAN_POINT ( 'NONE',  ( -23.80321479583337307, -17.81075880182941873, 59.30378417737342289 ) ) ;
#34434 = ORIENTED_EDGE ( 'NONE', *, *, #31105, .T. ) ;
#34435 = CARTESIAN_POINT ( 'NONE',  ( -22.89412281574421471, -9.750308782327882895, 70.12523226502652562 ) ) ;
#34436 = SHAPE_REPRESENTATION_RELATIONSHIP ( 'NONE' , 'NONE' ,  #22625, #23202 ) ;
#34437 = VECTOR ( 'NONE', #29454, 1000.000000000000000 ) ;
#34438 = CARTESIAN_POINT ( 'NONE',  ( -24.53575672594257995, -12.58916661682799898, 69.89430231120414305 ) ) ;
#34439 = CARTESIAN_POINT ( 'NONE',  ( -21.90064967531214890, -9.427635609301674435, 60.00705870275116638 ) ) ;
#34440 = VECTOR ( 'NONE', #41959, 1000.000000000000000 ) ;
#34441 = VECTOR ( 'NONE', #45661, 1000.000000000000000 ) ;
#34442 = ORIENTED_EDGE ( 'NONE', *, *, #40191, .F. ) ;
#34443 = AXIS2_PLACEMENT_3D ( 'NONE', #20861, #21108, #13691 ) ;
#34444 = VERTEX_POINT ( 'NONE', #1603 ) ;
#34445 = EDGE_CURVE ( 'NONE', #41130, #14380, #33139, .T. ) ;
#34446 = CARTESIAN_POINT ( 'NONE',  ( -21.41863048803932656, -8.999699081277377388, 73.61600897546567523 ) ) ;
#34447 = PLANE ( 'NONE',  #123 ) ;
#34448 = CARTESIAN_POINT ( 'NONE',  ( -13.29262146975105274, -21.00882449603590985, 61.69459112368684117 ) ) ;
#34449 = CARTESIAN_POINT ( 'NONE',  ( -10.17310289001843948, -13.09872099292910264, 71.40817355644446707 ) ) ;
#34450 = AXIS2_PLACEMENT_3D ( 'NONE', #10149, #43897, #10630 ) ;
#34451 = B_SPLINE_CURVE_WITH_KNOTS ( 'NONE', 3,
 ( #44792, #22368, #26306, #25814, #19401, #22615, #37613, #48457, #11046, #225 ),
 .UNSPECIFIED., .F., .F.,
 ( 4, 2, 2, 2, 4 ),
 ( 0.1272669073658194150, 0.2522669073463100209, 0.3772669073268006823, 0.5022669073072912882, 0.6272669072877818941 ),
 .UNSPECIFIED. ) ;
#34452 =( BOUNDED_CURVE ( )  B_SPLINE_CURVE ( 2, ( #47677, #44009, #6069, #28723, #44247, #17857, #2377, #32880, #29211 ),
 .UNSPECIFIED., .F., .F. ) 
 B_SPLINE_CURVE_WITH_KNOTS ( ( 3, 2, 2, 2, 3 ),
 ( 0.05507682622128801109, 0.05606042056139406982, 0.05704401490150013548, 0.05802760924160620809, 0.05901120358171226682 ),
 .UNSPECIFIED. ) 
 CURVE ( )  GEOMETRIC_REPRESENTATION_ITEM ( )  RATIONAL_B_SPLINE_CURVE ( ( 0.9999999999993087751, 0.9238795325119779633, 1.000000000000000000, 0.9238795325112867385, 1.000000000000000000, 0.9238795325112867385, 1.000000000000000000, 0.9238795325111853751, 1.000000000000101474 ) ) 
 REPRESENTATION_ITEM ( '' )  );
#34453 = ORIENTED_EDGE ( 'NONE', *, *, #23381, .T. ) ;
#34454 = CARTESIAN_POINT ( 'NONE',  ( -20.17037934351568751, -8.316057459223078041, 70.55100343557511167 ) ) ;
#34455 = CARTESIAN_POINT ( 'NONE',  ( -13.46025101761997078, -8.974705932511858109, 64.00126803586600488 ) ) ;
#34456 = ORIENTED_EDGE ( 'NONE', *, *, #39390, .F. ) ;
#34457 = EDGE_CURVE ( 'NONE', #24815, #25854, #28445, .T. ) ;
#34458 = CARTESIAN_POINT ( 'NONE',  ( -12.94403785604389867, -20.18778427150672883, 71.91539741676557185 ) ) ;
#34459 = B_SPLINE_CURVE_WITH_KNOTS ( 'NONE', 3,
 ( #1903, #43526, #9305, #35626, #16906, #8831, #31943, #24804, #39813, #46957 ),
 .UNSPECIFIED., .F., .F.,
 ( 4, 2, 2, 2, 4 ),
 ( 0.000000000000000000, 0.2500000000000000000, 0.5000000000000000000, 0.7500000000000000000, 1.000000000000000000 ),
 .UNSPECIFIED. ) ;
#34460 = ORIENTED_EDGE ( 'NONE', *, *, #31030, .T. ) ;
#34461 = CARTESIAN_POINT ( 'NONE',  ( -21.77428020737724523, -9.323007506576582060, 66.77223141407961293 ) ) ;
#34462 =( BOUNDED_CURVE ( )  B_SPLINE_CURVE ( 3, ( #1634, #20602, #35599, #21568 ),
 .UNSPECIFIED., .F., .F. ) 
 B_SPLINE_CURVE_WITH_KNOTS ( ( 4, 4 ),
 ( 0.4074455897393726156, 0.5000000000000000000 ),
 .UNSPECIFIED. ) 
 CURVE ( )  GEOMETRIC_REPRESENTATION_ITEM ( )  RATIONAL_B_SPLINE_CURVE ( ( 0.6983129098261142698, 0.7760317562607251807, 0.8765941196520231626, 1.000000000000013989 ) ) 
 REPRESENTATION_ITEM ( '' )  );
#34463 = ORIENTED_EDGE ( 'NONE', *, *, #30232, .T. ) ;
#34464 = CARTESIAN_POINT ( 'NONE',  ( -24.53780051168580911, -12.59584816521350348, 69.95738404390658616 ) ) ;
#34465 = CARTESIAN_POINT ( 'NONE',  ( -11.10300763040008398, -10.86615618544839457, 57.39398486019972268 ) ) ;
#34466 = B_SPLINE_CURVE_WITH_KNOTS ( 'NONE', 3,
 ( #29320, #40397, #33223, #18219, #21688, #17969, #21924, #25615, #40628, #36928 ),
 .UNSPECIFIED., .F., .F.,
 ( 4, 2, 2, 2, 4 ),
 ( 0.1272669073658077854, 0.2522669073439209875, 0.3772669073220341618, 0.5022669073001474471, 0.6272669072782606214 ),
 .UNSPECIFIED. ) ;
#34467 = ORIENTED_EDGE ( 'NONE', *, *, #7017, .T. ) ;
#34468 = DIRECTION ( 'NONE',  ( -0.06357898915124166050, 0.9979768094191900918, 0.000000000000000000 ) ) ;
#34469 = DIRECTION ( 'NONE',  ( -2.866981220435666553E-17, 1.000000000000000000, 1.190614954331866791E-16 ) ) ;
#34470 = CARTESIAN_POINT ( 'NONE',  ( -15.91784385650552025, -9.790100578890868377, 49.79778022625163203 ) ) ;
#34471 = VECTOR ( 'NONE', #45171, 1000.000000000000000 ) ;
#34472 = DIRECTION ( 'NONE',  ( -0.9687793358424823253, 0.2479245821708663811, 0.000000000000000000 ) ) ;
#34473 = CARTESIAN_POINT ( 'NONE',  ( -33.52409385541305653, -2.423472813913224222, 52.29999999999998295 ) ) ;
#34474 = CARTESIAN_POINT ( 'NONE',  ( -21.70399976399352937, -9.206932529385648323, 66.66150014529212342 ) ) ;
#34475 = ORIENTED_EDGE ( 'NONE', *, *, #45709, .T. ) ;
#34476 = CARTESIAN_POINT ( 'NONE',  ( -19.22579309969192707, -21.57336792462666253, 58.52507384993226225 ) ) ;
#34477 = CIRCLE ( 'NONE', #19557, 2.000000000000000888 ) ;
#34478 = CIRCLE ( 'NONE', #15636, 5.249999999999998224 ) ;
#34479 = CARTESIAN_POINT ( 'NONE',  ( -16.50534385541304161, -7.595227055684746098, 51.75156210489594599 ) ) ;
#34480 = DIRECTION ( 'NONE',  ( 0.3636930986378154040, 0.9315188296557533887, -1.850371886801397658E-09 ) ) ;
#34481 = CYLINDRICAL_SURFACE ( 'NONE', #44777, 0.1499999999999998002 ) ;
#34482 = DIRECTION ( 'NONE',  ( 0.9687793358424821033, -0.2479245821708677133, 0.000000000000000000 ) ) ;
#34483 = EDGE_CURVE ( 'NONE', #1731, #10912, #35475, .T. ) ;
#34484 = ADVANCED_FACE ( 'NONE', ( #24027 ), #2330, .T. ) ;
#34485 = ORIENTED_EDGE ( 'NONE', *, *, #18102, .T. ) ;
#34486 = ORIENTED_EDGE ( 'NONE', *, *, #6952, .T. ) ;
#34487 = CYLINDRICAL_SURFACE ( 'NONE', #14084, 0.1500000000000054068 ) ;
#34488 = LINE ( 'NONE', #45608, #10839 ) ;
#34489 = ORIENTED_EDGE ( 'NONE', *, *, #7793, .F. ) ;
#34490 = CARTESIAN_POINT ( 'NONE',  ( -21.05967961157278268, -21.31196033385931443, 62.30745545902120597 ) ) ;
#34491 = CARTESIAN_POINT ( 'NONE',  ( -15.12736151640637416, -21.89643440865206614, 68.69097607374993686 ) ) ;
#34492 = AXIS2_PLACEMENT_3D ( 'NONE', #24262, #28673, #24514 ) ;
#34493 = CARTESIAN_POINT ( 'NONE',  ( -22.38659385759799036, -7.222650657624104298, 49.61879703869476543 ) ) ;
#34494 = CARTESIAN_POINT ( 'NONE',  ( -24.72409385541305582, -14.80920654474411613, 58.00588235294116402 ) ) ;
#34495 = CARTESIAN_POINT ( 'NONE',  ( -14.12328906776938631, -8.570644558479624919, 67.41542347112275024 ) ) ;
#34496 = CARTESIAN_POINT ( 'NONE',  ( -10.86088752666615065, -11.28245350497684818, 67.80519939327926693 ) ) ;
#34497 = LINE ( 'NONE', #22964, #30298 ) ;
#34498 = B_SPLINE_CURVE_WITH_KNOTS ( 'NONE', 3,
 ( #21670, #10109, #32743, #36425, #2939, #2703, #36909, #40148, #25369, #36658 ),
 .UNSPECIFIED., .F., .F.,
 ( 4, 2, 2, 2, 4 ),
 ( 0.000000000000000000, 0.2500000000000000000, 0.5000000000000000000, 0.7500000000000000000, 1.000000000000000000 ),
 .UNSPECIFIED. ) ;
#34499 = VERTEX_POINT ( 'NONE', #21046 ) ;
#34500 = ADVANCED_FACE ( 'NONE', ( #35806 ), #2083, .T. ) ;
#34501 = EDGE_CURVE ( 'NONE', #9962, #23568, #39024, .T. ) ;
#34502 = CARTESIAN_POINT ( 'NONE',  ( -22.50076973789108692, -19.70108052134635557, 72.64400543415067091 ) ) ;
#34503 = CARTESIAN_POINT ( 'NONE',  ( -11.56046518335400286, -10.21343137625755482, 71.16167249782886017 ) ) ;
#34504 = EDGE_CURVE ( 'NONE', #48202, #33991, #47140, .T. ) ;
#34505 = CARTESIAN_POINT ( 'NONE',  ( -13.90805003106573068, -20.86209311441256986, 68.75625137331327608 ) ) ;
#34506 = CARTESIAN_POINT ( 'NONE',  ( -12.80044327789678249, -20.06500310223181671, 71.80653684543825932 ) ) ;
#34507 = CARTESIAN_POINT ( 'NONE',  ( -18.12432747636454877, -22.22630431188652977, 65.60178084401016463 ) ) ;
#34508 = EDGE_LOOP ( 'NONE', ( #7958, #39789 ) ) ;
#34509 = ORIENTED_EDGE ( 'NONE', *, *, #34127, .F. ) ;
#34510 = CARTESIAN_POINT ( 'NONE',  ( -20.04849592361258104, -21.35284569240296548, 72.69006679631316103 ) ) ;
#34511 = VERTEX_POINT ( 'NONE', #13394 ) ;
#34512 = EDGE_CURVE ( 'NONE', #12297, #29684, #26719, .T. ) ;
#34513 = CARTESIAN_POINT ( 'NONE',  ( -12.01952932525029816, -9.681273877180114340, 60.69884694392221292 ) ) ;
#34514 = CIRCLE ( 'NONE', #41593, 1.999999999999999778 ) ;
#34515 = CARTESIAN_POINT ( 'NONE',  ( -10.02995829593802668, -13.89786868041111667, 57.63320316755233819 ) ) ;
#34516 = CIRCLE ( 'NONE', #2297, 1.999999999999999112 ) ;
#34517 = VECTOR ( 'NONE', #23177, 1000.000000000000000 ) ;
#34518 = LINE ( 'NONE', #1517, #12485 ) ;
#34519 = CARTESIAN_POINT ( 'NONE',  ( -11.30361347545239958, -11.41219030243732391, 64.14882039658046153 ) ) ;
#34520 = CARTESIAN_POINT ( 'NONE',  ( -17.31415506352089650, -21.86632207739205569, 72.32110344861041540 ) ) ;
#34521 = ORIENTED_EDGE ( 'NONE', *, *, #36383, .T. ) ;
#34522 = CARTESIAN_POINT ( 'NONE',  ( -14.34827028450108344, -21.16170790896200060, 72.08174668229233362 ) ) ;
#34523 = AXIS2_PLACEMENT_3D ( 'NONE', #35391, #33988, #46498 ) ;
#34524 = CARTESIAN_POINT ( 'NONE',  ( -19.67760665824181388, -21.48965406232008490, 65.75014118398131302 ) ) ;
#34525 = VERTEX_POINT ( 'NONE', #16848 ) ;
#34526 = CARTESIAN_POINT ( 'NONE',  ( -11.36856108582972702, -11.29517246406753195, 64.22052367023555064 ) ) ;
#34527 = ORIENTED_EDGE ( 'NONE', *, *, #46240, .T. ) ;
#34528 = DIRECTION ( 'NONE',  ( -3.071710424422018668E-17, 6.404604876783312462E-16, 1.000000000000000000 ) ) ;
#34529 = CARTESIAN_POINT ( 'NONE',  ( -16.84865286310842336, -21.83598151670433296, 68.98088545748413480 ) ) ;
#34530 = DIRECTION ( 'NONE',  ( -0.04086606279947146980, -0.9938001236776475844, 0.1033986416233891037 ) ) ;
#34531 = ORIENTED_EDGE ( 'NONE', *, *, #3603, .T. ) ;
#34532 = CARTESIAN_POINT ( 'NONE',  ( -23.20845821660187980, -10.11394778068016898, 63.19373217977586421 ) ) ;
#34533 = CARTESIAN_POINT ( 'NONE',  ( -24.09286991228532315, -11.48796221018129238, 63.05879980478538727 ) ) ;
#34534 = CARTESIAN_POINT ( 'NONE',  ( -18.35897211656709160, -21.79709577657633446, 69.10954899396081430 ) ) ;
#34535 = CARTESIAN_POINT ( 'NONE',  ( -24.21281492007539526, -12.87834259335418530, 73.38658464541695992 ) ) ;
#34536 = CARTESIAN_POINT ( 'NONE',  ( -17.60534385759799036, -7.595227055684746986, 51.75156210489594599 ) ) ;
#34537 = CARTESIAN_POINT ( 'NONE',  ( -12.23220206747518013, -19.57856285391799034, 58.22682373937799838 ) ) ;
#34538 = CARTESIAN_POINT ( 'NONE',  ( -22.33041777183100507, -20.41561037748852669, 62.34943743628787161 ) ) ;
#34539 = DIRECTION ( 'NONE',  ( 0.7506333037770493988, -0.6607190350373991494, 0.000000000000000000 ) ) ;
#34540 = B_SPLINE_CURVE_WITH_KNOTS ( 'NONE', 3,
 ( #35051, #28412, #12889, #1315 ),
 .UNSPECIFIED., .F., .F.,
 ( 4, 4 ),
 ( 0.001041996463599131851, 0.002493317452641906698 ),
 .UNSPECIFIED. ) ;
#34541 = FACE_OUTER_BOUND ( 'NONE', #19600, .T. ) ;
#34542 = CARTESIAN_POINT ( 'NONE',  ( -20.10534385650552025, -8.801233750844183135, 48.81488406609782515 ) ) ;
#34543 = EDGE_CURVE ( 'NONE', #47823, #46955, #40505, .T. ) ;
#34544 = ORIENTED_EDGE ( 'NONE', *, *, #40997, .F. ) ;
#34545 = AXIS2_PLACEMENT_3D ( 'NONE', #45057, #15449, #7868 ) ;
#34546 = CARTESIAN_POINT ( 'NONE',  ( -43.17409385541305511, -15.80920654474410725, 56.99999999999998579 ) ) ;
#34547 = CARTESIAN_POINT ( 'NONE',  ( -24.28028284729623465, -16.22112348152082362, 59.19620387435347197 ) ) ;
#34548 = ORIENTED_EDGE ( 'NONE', *, *, #47400, .F. ) ;
#34549 = DIRECTION ( 'NONE',  ( 0.9710973231077276724, -0.2386838684389877008, 7.431671637556431570E-08 ) ) ;
#34550 = SHAPE_REPRESENTATION ( 'Speed Governor Worm Gear Train', ( #29031 ), #9367 ) ;
#34551 = CARTESIAN_POINT ( 'NONE',  ( -23.24167040808332985, -10.15534690731836065, 63.27197199642595393 ) ) ;
#34552 = CARTESIAN_POINT ( 'NONE',  ( -14.74690658000796439, -21.27702444416618732, 58.16617884968206198 ) ) ;
#34553 = ORIENTED_EDGE ( 'NONE', *, *, #28959, .F. ) ;
#34554 = CARTESIAN_POINT ( 'NONE',  ( -17.04978450098071718, -7.769001547375945727, 73.96578056985927674 ) ) ;
#34555 = AXIS2_PLACEMENT_3D ( 'NONE', #33379, #45479, #7074 ) ;
#34556 = CARTESIAN_POINT ( 'NONE',  ( -15.28291166272248169, -21.52618791248891128, 68.87592918174580348 ) ) ;
#34557 = EDGE_CURVE ( 'NONE', #22030, #17855, #27234, .T. ) ;
#34558 = CARTESIAN_POINT ( 'NONE',  ( -12.05749060505181269, -9.640721912800795934, 60.74573338552316670 ) ) ;
#34559 = VERTEX_POINT ( 'NONE', #47873 ) ;
#34560 = CARTESIAN_POINT ( 'NONE',  ( -18.60622205832422082, -22.16490843864383109, 72.47006330605313451 ) ) ;
#34561 = ADVANCED_FACE ( 'NONE', ( #21539 ), #6994, .T. ) ;
#34562 = VECTOR ( 'NONE', #17343, 1000.000000000000227 ) ;
#34563 = EDGE_CURVE ( 'NONE', #34852, #12698, #318, .T. ) ;
#34564 = DIRECTION ( 'NONE',  ( 0.000000000000000000, 0.000000000000000000, -1.000000000000000000 ) ) ;
#34565 = CARTESIAN_POINT ( 'NONE',  ( -10.01440776720603765, -14.03439672543145988, 61.03325998023760235 ) ) ;
#34566 = DIRECTION ( 'NONE',  ( 1.389773841562029912E-07, 3.718553644687884925E-07, -0.9999999999999211742 ) ) ;
#34567 = CARTESIAN_POINT ( 'NONE',  ( -13.24129617563109740, -8.644154241298165786, 60.69596227262822907 ) ) ;
#34568 = ORIENTED_EDGE ( 'NONE', *, *, #32363, .F. ) ;
#34569 = VERTEX_POINT ( 'NONE', #40970 ) ;
#34570 = CARTESIAN_POINT ( 'NONE',  ( -21.73659385541304090, -8.995762431863214559, 51.38120296130585274 ) ) ;
#34571 = CARTESIAN_POINT ( 'NONE',  ( -24.40026719341414108, -15.82783281859430780, 69.53867305742785732 ) ) ;
#34572 = CARTESIAN_POINT ( 'NONE',  ( -23.39840055413978348, -11.16100488844999994, 73.36193259119190202 ) ) ;
#34573 = CARTESIAN_POINT ( 'NONE',  ( -11.46044050272623416, -11.04924139602722377, 57.20903212151935691 ) ) ;
#34574 = CARTESIAN_POINT ( 'NONE',  ( -10.76542905790024385, -16.97361952088028758, 61.26816177302506361 ) ) ;
#34575 = CARTESIAN_POINT ( 'NONE',  ( 18.87590614458706995, 1.890747609047893185, 50.53028072113869484 ) ) ;
#34576 = CIRCLE ( 'NONE', #17246, 1.999999999999999112 ) ;
#34577 = LINE ( 'NONE', #39008, #35427 ) ;
#34578 = CYLINDRICAL_SURFACE ( 'NONE', #17811, 1.999999999999999112 ) ;
#34579 = VERTEX_POINT ( 'NONE', #36520 ) ;
#34580 = CARTESIAN_POINT ( 'NONE',  ( -21.89953879547803695, -8.853196296446007807, 66.70504049802050872 ) ) ;
#34581 = AXIS2_PLACEMENT_3D ( 'NONE', #13417, #32157, #44226 ) ;
#34582 = CARTESIAN_POINT ( 'NONE',  ( -50.42409385541304800, -25.10920654474410441, 56.99999999999999289 ) ) ;
#34583 = B_SPLINE_CURVE_WITH_KNOTS ( 'NONE', 1,
 ( #25318, #7090 ),
 .UNSPECIFIED., .F., .F.,
 ( 2, 2 ),
 ( 0.000000000000000000, 1.000000000000000000 ),
 .UNSPECIFIED. ) ;
#34584 = EDGE_LOOP ( 'NONE', ( #39499, #31084, #15400, #42862 ) ) ;
#34585 = DIRECTION ( 'NONE',  ( 0.000000000000000000, 0.000000000000000000, 1.000000000000000000 ) ) ;
#34586 = PLANE ( 'NONE',  #19475 ) ;
#34587 = CARTESIAN_POINT ( 'NONE',  ( -12.10131192688100299, -10.18592936015514816, 64.31442259820508411 ) ) ;
#34588 = LINE ( 'NONE', #8041, #4990 ) ;
#34589 = ORIENTED_EDGE ( 'NONE', *, *, #45271, .T. ) ;
#34590 = CARTESIAN_POINT ( 'NONE',  ( -22.58065782673598676, -12.89613362149922438, 54.07175714974875547 ) ) ;
#34591 = AXIS2_PLACEMENT_3D ( 'NONE', #44944, #595, #22776 ) ;
#34592 =( BOUNDED_CURVE ( )  B_SPLINE_CURVE ( 3, ( #16932, #13001, #43315, #1932 ),
 .UNSPECIFIED., .F., .F. ) 
 B_SPLINE_CURVE_WITH_KNOTS ( ( 4, 4 ),
 ( 0.4074455897393606807, 0.5000000000000000000 ),
 .UNSPECIFIED. ) 
 CURVE ( )  GEOMETRIC_REPRESENTATION_ITEM ( )  RATIONAL_B_SPLINE_CURVE ( ( 0.6983129098260772993, 0.7760317562606969810, 0.8765941196520082856, 1.000000000000019762 ) ) 
 REPRESENTATION_ITEM ( '' )  );
#34593 = ADVANCED_FACE ( 'NONE', ( #10685 ), #44436, .T. ) ;
#34594 = CARTESIAN_POINT ( 'NONE',  ( -21.73099075187129614, -8.730192115828774746, 70.31627817507801126 ) ) ;
#34595 = CARTESIAN_POINT ( 'NONE',  ( -20.90213356920466126, -8.220891710688713161, 59.94101618556534561 ) ) ;
#34596 = VERTEX_POINT ( 'NONE', #3043 ) ;
#34597 = CARTESIAN_POINT ( 'NONE',  ( -10.33743488275009526, -17.10781281734085724, 57.80947783183761146 ) ) ;
#34598 = CARTESIAN_POINT ( 'NONE',  ( -45.92409385541306222, -13.70421070448077039, 70.50000000000000000 ) ) ;
#34599 = CARTESIAN_POINT ( 'NONE',  ( -23.81024772113315890, -18.64597811008791695, 72.94863512192290500 ) ) ;
#34600 = CARTESIAN_POINT ( 'NONE',  ( -19.52100072682865672, -19.90831991051152627, 53.88362224778185805 ) ) ;
#34601 = APPLICATION_PROTOCOL_DEFINITION ( 'draft international standard', 'automotive_design', 1998, #34083 ) ;
#34602 = CARTESIAN_POINT ( 'NONE',  ( -22.81278634540432648, -10.26332246522033032, 66.54182271920811331 ) ) ;
#34603 = CARTESIAN_POINT ( 'NONE',  ( -14.51638892016982219, -21.23572161159003713, 58.46617851441119029 ) ) ;
#34604 = EDGE_LOOP ( 'NONE', ( #15471, #13684, #22161, #19549, #43122 ) ) ;
#34605 = DIRECTION ( 'NONE',  ( -6.471065199890530885E-06, -1.909039593073236381E-06, 0.9999999999772404280 ) ) ;
#34606 = ORIENTED_EDGE ( 'NONE', *, *, #19074, .T. ) ;
#34607 = CARTESIAN_POINT ( 'NONE',  ( -22.79734292848665334, -10.24514101169484270, 66.84182257473257494 ) ) ;
#34608 = CARTESIAN_POINT ( 'NONE',  ( -13.18108784799495936, -9.241582085570342997, 67.67942828295852564 ) ) ;
#34609 = ORIENTED_EDGE ( 'NONE', *, *, #34982, .T. ) ;
#34610 =( BOUNDED_CURVE ( )  B_SPLINE_CURVE ( 3, ( #36246, #9198, #39953, #9444 ),
 .UNSPECIFIED., .F., .F. ) 
 B_SPLINE_CURVE_WITH_KNOTS ( ( 4, 4 ),
 ( 0.4074455897393677306, 0.5000000000000000000 ),
 .UNSPECIFIED. ) 
 CURVE ( )  GEOMETRIC_REPRESENTATION_ITEM ( )  RATIONAL_B_SPLINE_CURVE ( ( 0.6983129098261039447, 0.7760317562607236264, 0.8765941196520269374, 1.000000000000025313 ) ) 
 REPRESENTATION_ITEM ( '' )  );
#34611 = CARTESIAN_POINT ( 'NONE',  ( -24.71334378318632830, -13.26952680650525274, 59.47772536435775947 ) ) ;
#34612 = FACE_BOUND ( 'NONE', #35969, .T. ) ;
#34613 = VERTEX_POINT ( 'NONE', #29159 ) ;
#34614 = ORIENTED_EDGE ( 'NONE', *, *, #46523, .T. ) ;
#34615 = ORIENTED_EDGE ( 'NONE', *, *, #9148, .F. ) ;
#34616 = ADVANCED_FACE ( 'NONE', ( #2805 ), #7254, .T. ) ;
#34618 = CARTESIAN_POINT ( 'NONE',  ( -10.46291082975850806, -15.97406517396614944, 61.19356052171543325 ) ) ;
#34617 = CIRCLE ( 'NONE', #14944, 2.000000000000002665 ) ;
#34619 = AXIS2_PLACEMENT_3D ( 'NONE', #10922, #4031, #45389 ) ;
#34620 = CARTESIAN_POINT ( 'NONE',  ( -21.90534385541302598, -7.595227055684733664, 51.75156210489598152 ) ) ;
#34621 = ADVANCED_FACE ( 'NONE', ( #29401 ), #48594, .T. ) ;
#34622 = CARTESIAN_POINT ( 'NONE',  ( -24.34138173484705803, -16.17068648017255583, 62.59328676670276792 ) ) ;
#34623 = CARTESIAN_POINT ( 'NONE',  ( -17.43166586245951422, -7.359124596637800053, 67.13544155391683432 ) ) ;
#34624 = CARTESIAN_POINT ( 'NONE',  ( -11.81636632494307015, -9.904339708471926684, 64.15101585200166312 ) ) ;
#34625 = CARTESIAN_POINT ( 'NONE',  ( -19.41839014062696123, -8.097970103967929489, 60.18922903702627281 ) ) ;
#34626 = CIRCLE ( 'NONE', #15737, 0.5000000000000004441 ) ;
#34627 =( BOUNDED_CURVE ( )  B_SPLINE_CURVE ( 3, ( #24498, #32588, #32113, #17559 ),
 .UNSPECIFIED., .F., .F. ) 
 B_SPLINE_CURVE_WITH_KNOTS ( ( 4, 4 ),
 ( 0.9074455897393698400, 1.000000000000000000 ),
 .UNSPECIFIED. ) 
 CURVE ( )  GEOMETRIC_REPRESENTATION_ITEM ( )  RATIONAL_B_SPLINE_CURVE ( ( 0.6983129098261089407, 0.7760317562607119690, 0.8765941196520089518, 1.000000000000000000 ) ) 
 REPRESENTATION_ITEM ( '' )  );
#34628 = EDGE_LOOP ( 'NONE', ( #19474, #31028, #33017, #9686, #47839 ) ) ;
#34629 = ORIENTED_EDGE ( 'NONE', *, *, #11857, .T. ) ;
#34630 = EDGE_CURVE ( 'NONE', #31526, #3895, #33549, .T. ) ;
#34631 = CARTESIAN_POINT ( 'NONE',  ( -22.72409385650551528, -6.426201560718813433, 50.50509628382439331 ) ) ;
#34632 = CARTESIAN_POINT ( 'NONE',  ( -13.76849323099554567, -20.83774554052356009, 65.27156739751333703 ) ) ;
#34633 = DIRECTION ( 'NONE',  ( -0.9501515917649785425, -0.3117883138709295898, 1.594035198720926202E-08 ) ) ;
#34634 = AXIS2_PLACEMENT_3D ( 'NONE', #1371, #12938, #28216 ) ;
#34635 = CARTESIAN_POINT ( 'NONE',  ( -19.74220741432039716, -21.41423112065765011, 65.57372225646707875 ) ) ;
#34636 = ORIENTED_EDGE ( 'NONE', *, *, #23010, .T. ) ;
#34637 = EDGE_CURVE ( 'NONE', #23016, #24237, #17809, .T. ) ;
#34638 = CARTESIAN_POINT ( 'NONE',  ( -15.71784385650551741, -9.790100578890868377, 49.79778022625163203 ) ) ;
#34639 = EDGE_CURVE ( 'NONE', #14925, #4590, #10933, .T. ) ;
#34640 = VERTEX_POINT ( 'NONE', #6518 ) ;
#34641 = DIRECTION ( 'NONE',  ( -0.9774082387306984865, 0.2113602016968848529, -7.903122840838824810E-08 ) ) ;
#34642 = CARTESIAN_POINT ( 'NONE',  ( -15.33758281339130036, -21.49113659546963362, 68.87592903483572115 ) ) ;
#34643 = VECTOR ( 'NONE', #7606, 1000.000000000000000 ) ;
#34644 = B_SPLINE_CURVE_WITH_KNOTS ( 'NONE', 1,
 ( #3149, #7352 ),
 .UNSPECIFIED., .F., .F.,
 ( 2, 2 ),
 ( 0.000000000000000000, 1.000000000000000000 ),
 .UNSPECIFIED. ) ;
#34645 = CARTESIAN_POINT ( 'NONE',  ( -12.44661342226983969, -19.73288402143430886, 64.93845064584576221 ) ) ;
#34646 = EDGE_LOOP ( 'NONE', ( #23001, #8170, #23013, #11606 ) ) ;
#34647 = CARTESIAN_POINT ( 'NONE',  ( -23.34481426128875015, -18.63642081788813343, 69.29371984264746231 ) ) ;
#34648 = AXIS2_PLACEMENT_3D ( 'NONE', #12778, #45802, #23636 ) ;
#34649 = CARTESIAN_POINT ( 'NONE',  ( -10.44881520703817479, -17.42631679175528703, 64.74244059074541724 ) ) ;
#34650 = CYLINDRICAL_SURFACE ( 'NONE', #43655, 2.000000000000001332 ) ;
#34651 = AXIS2_PLACEMENT_3D ( 'NONE', #5302, #38045, #35328 ) ;
#34652 = VERTEX_POINT ( 'NONE', #43958 ) ;
#34653 = CARTESIAN_POINT ( 'NONE',  ( -21.68499601416157674, -9.192516039336664946, 66.66149992327366647 ) ) ;
#34654 = EDGE_CURVE ( 'NONE', #47654, #46361, #35511, .T. ) ;
#34655 = CARTESIAN_POINT ( 'NONE',  ( -22.96484172783137012, -19.08706962207428504, 58.88410642316259214 ) ) ;
#34656 = CARTESIAN_POINT ( 'NONE',  ( -36.42409385541304800, -8.109206544743658540, 50.50000000000030553 ) ) ;
#34657 = ORIENTED_EDGE ( 'NONE', *, *, #39803, .T. ) ;
#34658 = B_SPLINE_CURVE_WITH_KNOTS ( 'NONE', 3,
 ( #37072, #22558, #26251, #29956, #3105, #3858, #18863, #30209, #11474, #26498 ),
 .UNSPECIFIED., .F., .F.,
 ( 4, 2, 2, 2, 4 ),
 ( 0.1272669073658397321, 0.2522669073463245093, 0.3772669073268092310, 0.5022669073072940638, 0.6272669072877787855 ),
 .UNSPECIFIED. ) ;
#34659 = CARTESIAN_POINT ( 'NONE',  ( -22.51043027204183034, -20.25270558619591910, 65.85421731173748583 ) ) ;
#34660 = AXIS2_PLACEMENT_3D ( 'NONE', #6501, #36503, #2785 ) ;
#34661 = VERTEX_POINT ( 'NONE', #26199 ) ;
#34662 = FACE_OUTER_BOUND ( 'NONE', #31874, .T. ) ;
#34663 = PRODUCT_DEFINITION_SHAPE ( 'NONE', 'NONE',  #37283 ) ;
#34664 = CARTESIAN_POINT ( 'NONE',  ( -14.79922921121938195, -7.836842249070715916, 57.03495322699122738 ) ) ;
#34665 = VERTEX_POINT ( 'NONE', #37247 ) ;
#34666 = CARTESIAN_POINT ( 'NONE',  ( -16.36675962830097930, -22.18387328577503581, 61.79922180027413958 ) ) ;
#34667 = CARTESIAN_POINT ( 'NONE',  ( -23.84761967927745374, -12.02338244726358596, 59.67162711403931752 ) ) ;
#34668 = DIRECTION ( 'NONE',  ( -3.071710424422018668E-17, 6.404604876783312462E-16, 1.000000000000000000 ) ) ;
#34669 = VERTEX_POINT ( 'NONE', #44207 ) ;
#34670 = CARTESIAN_POINT ( 'NONE',  ( -9.995124286023395754, -14.24916261073750334, 64.58142169135716415 ) ) ;
#34671 = AXIS2_PLACEMENT_3D ( 'NONE', #68, #38439, #43796 ) ;
#34672 = DIRECTION ( 'NONE',  ( -1.000000000000000000, -2.866981220435666553E-17, 0.000000000000000000 ) ) ;
#34673 = CARTESIAN_POINT ( 'NONE',  ( -17.42409385541299471, -14.80920654474435594, 52.02966884056656482 ) ) ;
#34674 = ORIENTED_EDGE ( 'NONE', *, *, #13139, .F. ) ;
#34675 = EDGE_CURVE ( 'NONE', #22785, #37281, #19997, .T. ) ;
#34676 = CARTESIAN_POINT ( 'NONE',  ( -19.22943505703176115, -8.044692082162882230, 63.50259577331515715 ) ) ;
#34677 = DIRECTION ( 'NONE',  ( -5.731567514496413899E-31, -1.020425574103664789E-16, -1.000000000000000000 ) ) ;
#34679 = ORIENTED_EDGE ( 'NONE', *, *, #2049, .T. ) ;
#34678 = VECTOR ( 'NONE', #43882, 1000.000000000000000 ) ;
#34680 = VERTEX_POINT ( 'NONE', #10216 ) ;
#34681 = CARTESIAN_POINT ( 'NONE',  ( -45.92409385541306222, -14.20920654474410760, 70.50000000000000000 ) ) ;
#34682 = DIRECTION ( 'NONE',  ( 0.000000000000000000, 0.007114381193220324640, -0.9999746924698832418 ) ) ;
#34683 = CARTESIAN_POINT ( 'NONE',  ( -10.42496409799848323, -14.69883155267435626, 71.62782692796884021 ) ) ;
#34684 = CARTESIAN_POINT ( 'NONE',  ( -21.79284385650551314, -7.406986770994973490, 48.81910596585309747 ) ) ;
#34685 = CARTESIAN_POINT ( 'NONE',  ( -24.41160895735743352, -13.85031893932584701, 73.00782755091154286 ) ) ;
#34686 = CARTESIAN_POINT ( 'NONE',  ( -11.60006141122767609, -10.16330251221877390, 71.08397807149754044 ) ) ;
#34687 = CARTESIAN_POINT ( 'NONE',  ( -18.55956930788366677, -7.446158750330262421, 74.02559786541287679 ) ) ;
#34688 = DIRECTION ( 'NONE',  ( -3.071710424422018668E-17, 6.404604876783312462E-16, 1.000000000000000000 ) ) ;
#34689 = ORIENTED_EDGE ( 'NONE', *, *, #48623, .F. ) ;
#34690 = EDGE_LOOP ( 'NONE', ( #16525, #34719, #6548, #31573, #30618 ) ) ;
#34691 = EDGE_CURVE ( 'NONE', #12901, #7006, #14107, .T. ) ;
#34692 = CARTESIAN_POINT ( 'NONE',  ( -22.98865682493615381, -9.855478938366896813, 70.12683207277369490 ) ) ;
#34693 =( NAMED_UNIT ( * ) SI_UNIT ( $, .STERADIAN. ) SOLID_ANGLE_UNIT ( ) );
#34694 = EDGE_CURVE ( 'NONE', #8655, #40234, #24366, .T. ) ;
#34695 = AXIS2_PLACEMENT_3D ( 'NONE', #45235, #48659, #25766 ) ;
#34696 = CARTESIAN_POINT ( 'NONE',  ( -11.51319708992055801, -18.65819952746894472, 68.30869917720363560 ) ) ;
#34697 = DIRECTION ( 'NONE',  ( 1.224646799147353207E-16, 1.000000000000000000, -1.912410701131276611E-32 ) ) ;
#34698 = EDGE_CURVE ( 'NONE', #38602, #20878, #48417, .T. ) ;
#34699 = CARTESIAN_POINT ( 'NONE',  ( -18.76715758977493209, -7.481188742717107765, 70.41422074109146934 ) ) ;
#34700 = ORIENTED_EDGE ( 'NONE', *, *, #15305, .T. ) ;
#34701 = EDGE_LOOP ( 'NONE', ( #41712, #28623, #32153, #36694, #26993 ) ) ;
#34702 = CYLINDRICAL_SURFACE ( 'NONE', #33519, 0.1500000000000008826 ) ;
#34703 = DIRECTION ( 'NONE',  ( 0.6043825497304157190, -0.7966942535134532433, 5.656674838975381179E-08 ) ) ;
#34704 = CARTESIAN_POINT ( 'NONE',  ( -46.92409385541305511, -17.80920654474410370, 61.49999999999999289 ) ) ;
#34705 = CARTESIAN_POINT ( 'NONE',  ( -23.98984720795339243, -17.39877237835929691, 73.02768823732557735 ) ) ;
#34706 = VECTOR ( 'NONE', #38253, 1000.000000000000000 ) ;
#34707 = EDGE_CURVE ( 'NONE', #8636, #32302, #34277, .T. ) ;
#34708 = ORIENTED_EDGE ( 'NONE', *, *, #8186, .T. ) ;
#34709 = ADVANCED_FACE ( 'NONE', ( #34292 ), #45177, .T. ) ;
#34710 = CARTESIAN_POINT ( 'NONE',  ( -10.53709656823301799, -16.06259630760735035, 68.27767780832155609 ) ) ;
#34711 = DIRECTION ( 'NONE',  ( 1.674255585786183705E-21, -0.9999746924698832418, -0.007114381193220357599 ) ) ;
#34712 = EDGE_CURVE ( 'NONE', #2810, #33723, #31099, .T. ) ;
#34713 = EDGE_CURVE ( 'NONE', #36372, #34714, #44352, .T. ) ;
#34714 = VERTEX_POINT ( 'NONE', #23238 ) ;
#34715 = CARTESIAN_POINT ( 'NONE',  ( -22.66727051383977809, -10.09628829486277546, 70.31178520457007153 ) ) ;
#34716 = CARTESIAN_POINT ( 'NONE',  ( -17.56717507065399531, -7.360494836047319467, 63.73552460944732445 ) ) ;
#34717 = VERTEX_POINT ( 'NONE', #22757 ) ;
#34718 = CARTESIAN_POINT ( 'NONE',  ( -10.49991634527385287, -13.77081010382293158, 57.55898204955100539 ) ) ;
#34719 = ORIENTED_EDGE ( 'NONE', *, *, #17763, .T. ) ;
#34720 = CYLINDRICAL_SURFACE ( 'NONE', #14133, 0.1500000000000079881 ) ;
#34721 = B_SPLINE_CURVE_WITH_KNOTS ( 'NONE', 3,
 ( #12858, #9183, #47341, #24200, #2512, #17515, #16787, #39209, #5738, #28127 ),
 .UNSPECIFIED., .F., .F.,
 ( 4, 2, 2, 2, 4 ),
 ( 0.6272669072877680163, 0.7522669073072806301, 0.8772669073267931328, 1.002266907346305747, 1.127266907365818360 ),
 .UNSPECIFIED. ) ;
#34723 = CARTESIAN_POINT ( 'NONE',  ( -20.49049834636491596, -8.516442497579440385, 63.31121494938373928 ) ) ;
#34722 = VECTOR ( 'NONE', #40040, 1000.000000000000000 ) ;
#34724 = ORIENTED_EDGE ( 'NONE', *, *, #33578, .F. ) ;
#34725 = DIRECTION ( 'NONE',  ( 0.9687793358424821033, -0.2479245821708677133, 0.000000000000000000 ) ) ;
#34726 = PLANE ( 'NONE',  #43895 ) ;
#34727 = CARTESIAN_POINT ( 'NONE',  ( -16.14284385650551812, -8.811426318492348031, 52.18089403414751359 ) ) ;
#34728 = DIRECTION ( 'NONE',  ( -0.8604039311673230550, -0.5096126717731922495, 7.110477544621476444E-08 ) ) ;
#34729 = CARTESIAN_POINT ( 'NONE',  ( 18.82590614458706924, 1.904976371434334181, 48.53033133619892681 ) ) ;
#34730 = DIRECTION ( 'NONE',  ( -3.071710424422018668E-17, 6.404604876783312462E-16, 1.000000000000000000 ) ) ;
#34731 = ORIENTED_EDGE ( 'NONE', *, *, #46092, .F. ) ;
#34732 = CARTESIAN_POINT ( 'NONE',  ( -19.18784946220089083, -21.58347464219594514, 58.82507428380127834 ) ) ;
#34733 = CARTESIAN_POINT ( 'NONE',  ( -18.19071170428347273, -21.76716127234782761, 65.36034592301929536 ) ) ;
#34734 = CARTESIAN_POINT ( 'NONE',  ( -14.72744631621160494, -8.295007313424175521, 60.60524229057013201 ) ) ;
#34735 = CARTESIAN_POINT ( 'NONE',  ( -18.53201708017407157, -7.846807123103141102, 74.14064401780551350 ) ) ;
#34736 = CARTESIAN_POINT ( 'NONE',  ( -17.67903503446239455, -25.24601286685181023, 54.49999999999995026 ) ) ;
#34737 = ADVANCED_FACE ( 'NONE', ( #11657 ), #20019, .F. ) ;
#34738 = ORIENTED_EDGE ( 'NONE', *, *, #3210, .F. ) ;
#34739 = ORIENTED_EDGE ( 'NONE', *, *, #17839, .T. ) ;
#34740 = DIRECTION ( 'NONE',  ( -3.084459869131082876E-06, 5.853393715878419656E-06, -0.9999999999781118420 ) ) ;
#34741 = CARTESIAN_POINT ( 'NONE',  ( -12.03169470190467827, -10.26217700280571421, 71.06073263571943244 ) ) ;
#34742 = EDGE_LOOP ( 'NONE', ( #24209, #1359, #38057, #27615 ) ) ;
#34743 = CARTESIAN_POINT ( 'NONE',  ( -22.53655392111809164, -20.22829597721307948, 65.88917050827579658 ) ) ;
#34744 = AXIS2_PLACEMENT_3D ( 'NONE', #21991, #18029, #21273 ) ;
#34745 = CYLINDRICAL_SURFACE ( 'NONE', #1947, 2.000000000000003553 ) ;
#34746 = CARTESIAN_POINT ( 'NONE',  ( -11.07857854458970692, -11.73724703412850801, 71.08860870961423473 ) ) ;
#34747 = CARTESIAN_POINT ( 'NONE',  ( -21.01123855637963089, -20.87838213191899683, 65.58453944497207999 ) ) ;
#34748 = CARTESIAN_POINT ( 'NONE',  ( -15.73542338568409349, -8.015832264148292197, 70.60989886599207921 ) ) ;
#34749 = CYLINDRICAL_SURFACE ( 'NONE', #34199, 1.249999999999999334 ) ;
#34750 = ORIENTED_EDGE ( 'NONE', *, *, #27552, .F. ) ;
#34751 = EDGE_CURVE ( 'NONE', #44591, #33352, #32570, .T. ) ;
#34752 = CARTESIAN_POINT ( 'NONE',  ( -24.38143503755601316, -15.58083059521001168, 73.30303748419844112 ) ) ;
#34753 = DIRECTION ( 'NONE',  ( 0.000000000000000000, 1.000000000000000000, 0.000000000000000000 ) ) ;
#34754 = CARTESIAN_POINT ( 'NONE',  ( -17.59211729576255934, -7.811223397794364587, 63.55057029380298417 ) ) ;
#34755 = CARTESIAN_POINT ( 'NONE',  ( -19.94917705995926482, -8.226604131702123013, 74.00624557436877637 ) ) ;
#34756 =( BOUNDED_SURFACE ( )  B_SPLINE_SURFACE ( 3, 1, ( 
 ( #30998, #477 ),
 ( #41845, #31236 ),
 ( #8118, #42324 ),
 ( #8592, #23134 ),
 ( #38124, #4904 ),
 ( #4401, #19915 ),
 ( #46259, #26326 ) ),
 .UNSPECIFIED., .T., .F., .F. ) 
 B_SPLINE_SURFACE_WITH_KNOTS ( ( 4, 3, 4 ),
 ( 2, 2 ),
 ( 0.000000000000000000, 0.5000000000000000000, 1.000000000000000000 ),
 ( 0.000000000000000000, 1.000000000000000000 ),
 .UNSPECIFIED. ) 
 GEOMETRIC_REPRESENTATION_ITEM ( )  RATIONAL_B_SPLINE_SURFACE ( (
 ( 1.000000000000000000, 1.000000000000000000),
 ( 0.3333333333333335369, 0.3333333333333330373),
 ( 0.3333333333333335369, 0.3333333333333330373),
 ( 1.000000000000000000, 1.000000000000000000),
 ( 0.3333333333333333703, 0.3333333333333333703),
 ( 0.3333333333333333703, 0.3333333333333333703),
 ( 1.000000000000000000, 1.000000000000000000) ) ) 
 REPRESENTATION_ITEM ( '' )  SURFACE ( )  );
#34757 = CARTESIAN_POINT ( 'NONE',  ( -19.84080129957490612, -21.85712737670714390, 65.57830891090566183 ) ) ;
#34758 = ORIENTED_EDGE ( 'NONE', *, *, #21891, .F. ) ;
#34759 = ORIENTED_EDGE ( 'NONE', *, *, #25951, .F. ) ;
#34760 = CARTESIAN_POINT ( 'NONE',  ( -19.92776479198160189, -21.39998277484045275, 72.41950795000725805 ) ) ;
#34761 = B_SPLINE_CURVE_WITH_KNOTS ( 'NONE', 3,
 ( #31499, #31018, #38385, #12782, #31745, #46039, #16940, #27316, #12061, #23384 ),
 .UNSPECIFIED., .F., .F.,
 ( 4, 2, 2, 2, 4 ),
 ( 0.1272669073658920791, 0.2522669073463494893, 0.3772669073268068995, 0.5022669073072643098, 0.6272669072877217200 ),
 .UNSPECIFIED. ) ;
#34762 = ORIENTED_EDGE ( 'NONE', *, *, #26891, .F. ) ;
#34763 = CARTESIAN_POINT ( 'NONE',  ( -17.25805186741143871, -7.753187986760909034, 63.70624286928425306 ) ) ;
#34764 = VECTOR ( 'NONE', #1993, 1000.000000000000000 ) ;
#34765 = CARTESIAN_POINT ( 'NONE',  ( -12.77013062424865630, -8.927826924028671840, 53.49999999999994316 ) ) ;
#34766 = ORIENTED_EDGE ( 'NONE', *, *, #19621, .T. ) ;
#34767 =( BOUNDED_CURVE ( )  B_SPLINE_CURVE ( 3, ( #2790, #18283, #21754, #3029 ),
 .UNSPECIFIED., .F., .F. ) 
 B_SPLINE_CURVE_WITH_KNOTS ( ( 4, 4 ),
 ( 4.712388980384690562, 4.921828490624010399 ),
 .UNSPECIFIED. ) 
 CURVE ( )  GEOMETRIC_REPRESENTATION_ITEM ( )  RATIONAL_B_SPLINE_CURVE ( ( 1.000000000000000000, 0.9963479302455154896, 0.9963479302455154896, 1.000000000000000000 ) ) 
 REPRESENTATION_ITEM ( '' )  );
#34768 = EDGE_CURVE ( 'NONE', #37232, #21212, #18501, .T. ) ;
#34769 = CARTESIAN_POINT ( 'NONE',  ( -10.43073325114686511, -14.50439929630985603, 68.15800126138398696 ) ) ;
#34770 = CARTESIAN_POINT ( 'NONE',  ( -13.40918607372062610, -8.533554674359928427, 57.07693621075073054 ) ) ;
#34771 = EDGE_CURVE ( 'NONE', #24347, #44341, #19648, .T. ) ;
#34772 = EDGE_CURVE ( 'NONE', #25179, #27516, #31933, .T. ) ;
#34773 = ORIENTED_EDGE ( 'NONE', *, *, #42205, .T. ) ;
#34774 = CARTESIAN_POINT ( 'NONE',  ( -17.75017200679030083, -21.85170198611075065, 58.70553379369455627 ) ) ;
#34775 = B_SPLINE_CURVE_WITH_KNOTS ( 'NONE', 3,
 ( #20810, #24030, #9500, #35809, #39521, #28452, #27709, #43474, #9736, #31161 ),
 .UNSPECIFIED., .F., .F.,
 ( 4, 2, 2, 2, 4 ),
 ( 0.000000000000000000, 0.2500000000000000000, 0.5000000000000000000, 0.7500000000000000000, 1.000000000000000000 ),
 .UNSPECIFIED. ) ;
#34776 = FACE_OUTER_BOUND ( 'NONE', #21737, .T. ) ;
#34777 = ORIENTED_EDGE ( 'NONE', *, *, #36642, .F. ) ;
#34778 = CARTESIAN_POINT ( 'NONE',  ( -11.36856035537877396, -11.29517376149446761, 64.37711966785748530 ) ) ;
#34779 = EDGE_LOOP ( 'NONE', ( #24583, #36493, #9461, #47890 ) ) ;
#34780 = EDGE_CURVE ( 'NONE', #1356, #3049, #26720, .T. ) ;
#34781 = EDGE_CURVE ( 'NONE', #24975, #44310, #11912, .T. ) ;
#34782 = CARTESIAN_POINT ( 'NONE',  ( -11.13656563017467782, -10.81292993477855902, 57.40241537293904628 ) ) ;
#34783 = CARTESIAN_POINT ( 'NONE',  ( -22.23704373183037575, -20.49607752381679759, 58.90296374359631670 ) ) ;
#34784 = CARTESIAN_POINT ( 'NONE',  ( -23.36965734407794670, -18.59798837310562902, 69.58812159897662752 ) ) ;
#34785 = EDGE_LOOP ( 'NONE', ( #4952, #29833, #22080, #11163, #12789 ) ) ;
#34786 = CARTESIAN_POINT ( 'NONE',  ( -11.04141120970326462, -11.93494789359697883, 74.55840195308121565 ) ) ;
#34787 = CARTESIAN_POINT ( 'NONE',  ( -24.08597852354971280, -11.47399750213189407, 63.07405535103134753 ) ) ;
#34788 = CARTESIAN_POINT ( 'NONE',  ( -16.15548939330727407, -7.924675066161051440, 63.95394534455144253 ) ) ;
#34789 = CARTESIAN_POINT ( 'NONE',  ( -24.72409385541305582, -14.90920654474419038, 65.94705882352940307 ) ) ;
#34790 = DIRECTION ( 'NONE',  ( -3.361323641615342917E-32, -0.9999954153791273948, -0.003028072113822189229 ) ) ;
#34791 = CARTESIAN_POINT ( 'NONE',  ( -22.76771927571487453, -10.21026527410489138, 66.83622464935415053 ) ) ;
#34792 = CARTESIAN_POINT ( 'NONE',  ( -17.59331747086620368, -7.761237804118464645, 63.85057029381061966 ) ) ;
#34793 = DIRECTION ( 'NONE',  ( 0.000000000000000000, -0.007114381193220324640, 0.9999746924698832418 ) ) ;
#34794 = CARTESIAN_POINT ( 'NONE',  ( -14.70534385650551989, -8.801233750844183135, 48.81488406609782515 ) ) ;
#34795 = EDGE_CURVE ( 'NONE', #12705, #29888, #38861, .T. ) ;
#34796 = ORIENTED_EDGE ( 'NONE', *, *, #45495, .F. ) ;
#34797 = DIRECTION ( 'NONE',  ( -0.1186632576870824130, 0.9929345553837299887, 6.051931679537041823E-08 ) ) ;
#34798 = CARTESIAN_POINT ( 'NONE',  ( -10.44881481234349252, -17.42631575494719698, 64.74243950200344955 ) ) ;
#34799 = ORIENTED_EDGE ( 'NONE', *, *, #5156, .F. ) ;
#34800 = FACE_OUTER_BOUND ( 'NONE', #35646, .T. ) ;
#34801 = DIRECTION ( 'NONE',  ( 4.664556981411351282E-06, -8.285185778185610086E-06, 0.9999999999547987128 ) ) ;
#34802 = CARTESIAN_POINT ( 'NONE',  ( -22.92319923916556235, -10.39759239192951235, 63.07185995337424345 ) ) ;
#34803 = CARTESIAN_POINT ( 'NONE',  ( -14.62324711167149260, -21.22583875644025753, 58.39447665211296368 ) ) ;
#34804 = EDGE_LOOP ( 'NONE', ( #40210, #32379, #24889, #36475, #35803 ) ) ;
#34805 = CARTESIAN_POINT ( 'NONE',  ( -24.40666182452685362, -14.31463369505075001, 66.40966133397022020 ) ) ;
#34806 = FACE_OUTER_BOUND ( 'NONE', #21549, .T. ) ;
#34807 = CARTESIAN_POINT ( 'NONE',  ( -12.41791333049023116, -9.841008508234809327, 60.97406688302051947 ) ) ;
#34808 = EDGE_LOOP ( 'NONE', ( #21782, #45755, #23053, #2837, #28969 ) ) ;
#34809 = CARTESIAN_POINT ( 'NONE',  ( -11.43942668935558515, -18.54264994400395850, 57.80714389716341373 ) ) ;
#34810 = FACE_OUTER_BOUND ( 'NONE', #37439, .T. ) ;
#34811 = CARTESIAN_POINT ( 'NONE',  ( -10.01424894596331505, -14.03598936870067782, 61.17467227907766869 ) ) ;
#34812 = CARTESIAN_POINT ( 'NONE',  ( -21.73797167162284438, -8.735188488120728678, 70.23794211215633254 ) ) ;
#34813 = DIRECTION ( 'NONE',  ( 0.9796876409582463419, -0.2005296141562635803, -7.890952368640937478E-08 ) ) ;
#34814 = EDGE_LOOP ( 'NONE', ( #47510, #19979, #27381, #13706, #44897 ) ) ;
#34815 = ORIENTED_EDGE ( 'NONE', *, *, #29887, .T. ) ;
#34816 = CARTESIAN_POINT ( 'NONE',  ( -20.66784385541303948, -9.357632978295830739, 49.97845033065684106 ) ) ;
#34817 = CARTESIAN_POINT ( 'NONE',  ( -13.87406498055279158, -8.713951040527767589, 74.19954688782125629 ) ) ;
#34818 = CARTESIAN_POINT ( 'NONE',  ( -23.41977742916776251, -11.19648202114625235, 73.66193302070908544 ) ) ;
#34819 = CARTESIAN_POINT ( 'NONE',  ( -17.77920954038207668, -22.25082405446125122, 58.59048702730397196 ) ) ;
#34820 = ADVANCED_FACE ( 'NONE', ( #30389 ), #1061, .T. ) ;
#34821 = CARTESIAN_POINT ( 'NONE',  ( -15.13017050835524913, -18.89591645955643529, 52.02966884056656482 ) ) ;
#34822 = CARTESIAN_POINT ( 'NONE',  ( -20.20088676517873694, -8.325823464045813083, 74.13585170226248522 ) ) ;
#34823 = B_SPLINE_CURVE_WITH_KNOTS ( 'NONE', 3,
 ( #30047, #18684, #47764, #48484, #32965, #14248, #37644, #10820, #7143, #36907 ),
 .UNSPECIFIED., .F., .F.,
 ( 4, 2, 2, 2, 4 ),
 ( 0.1272669073658264371, 0.2522669073439405274, 0.3772669073220545899, 0.5022669073001687634, 0.6272669072782828259 ),
 .UNSPECIFIED. ) ;
#34824 = CARTESIAN_POINT ( 'NONE',  ( -17.78516316699992217, -21.85793681952389989, 65.48965078530844153 ) ) ;
#34825 = ORIENTED_EDGE ( 'NONE', *, *, #3104, .T. ) ;
#34826 = CARTESIAN_POINT ( 'NONE',  ( -12.64995474452274138, -19.99670071527213366, 68.63657438322856308 ) ) ;
#34827 = CARTESIAN_POINT ( 'NONE',  ( -10.47654091737289050, -16.00694475801543248, 67.97767859625193410 ) ) ;
#34828 = ORIENTED_EDGE ( 'NONE', *, *, #24945, .F. ) ;
#34829 = EDGE_CURVE ( 'NONE', #35725, #21025, #23567, .T. ) ;
#34830 = EDGE_CURVE ( 'NONE', #3552, #21656, #37335, .T. ) ;
#34831 = DIRECTION ( 'NONE',  ( -0.000000000000000000, -1.000000000000000000, 0.000000000000000000 ) ) ;
#34832 = CARTESIAN_POINT ( 'NONE',  ( -13.88631413956031579, -11.73554473314222157, 49.52966884056655772 ) ) ;
#34833 = VERTEX_POINT ( 'NONE', #34537 ) ;
#34834 = CARTESIAN_POINT ( 'NONE',  ( -8.912481985338086332, -18.08067441140542186, 54.49999999999995026 ) ) ;
#34835 = EDGE_CURVE ( 'NONE', #45882, #2071, #31826, .T. ) ;
#34836 = CARTESIAN_POINT ( 'NONE',  ( -11.97490362423377164, -10.33561459433851404, 67.78424783647008667 ) ) ;
#34837 = SHAPE_REPRESENTATION ( 'Governing Air Vane Flywheel Fan', ( #29031 ), #4656 ) ;
#34838 = EDGE_CURVE ( 'NONE', #23394, #27273, #7410, .T. ) ;
#34839 = CARTESIAN_POINT ( 'NONE',  ( -21.57995947450667984, -9.113990939708571659, 70.14604673427196246 ) ) ;
#34840 = CARTESIAN_POINT ( 'NONE',  ( -24.47213906732331878, -17.22327966652203202, 72.98361780307556046 ) ) ;
#34841 = ORIENTED_EDGE ( 'NONE', *, *, #46041, .T. ) ;
#34842 = LINE ( 'NONE', #31649, #31498 ) ;
#34843 = CARTESIAN_POINT ( 'NONE',  ( -17.79333148728606417, -22.25021806323848494, 58.54406892197518886 ) ) ;
#34844 = DIRECTION ( 'NONE',  ( -2.160207931474222106E-15, -0.8949343913984794119, 0.4461977533473619473 ) ) ;
#34845 = FACE_BOUND ( 'NONE', #6567, .T. ) ;
#34846 = B_SPLINE_CURVE_WITH_KNOTS ( 'NONE', 1,
 ( #22789, #34322 ),
 .UNSPECIFIED., .F., .F.,
 ( 2, 2 ),
 ( 0.000000000000000000, 1.000000000000000000 ),
 .UNSPECIFIED. ) ;
#34847 = LINE ( 'NONE', #42739, #39195 ) ;
#34848 = CARTESIAN_POINT ( 'NONE',  ( -23.34611474887041282, -10.97735184451543589, 73.57013074316820678 ) ) ;
#34849 = ADVANCED_FACE ( 'NONE', ( #9429 ), #46847, .T. ) ;
#34850 = VECTOR ( 'NONE', #33599, 1000.000000000000227 ) ;
#34851 = CARTESIAN_POINT ( 'NONE',  ( -14.51923423662272938, -21.23689935983381716, 58.25797845284014187 ) ) ;
#34852 = VERTEX_POINT ( 'NONE', #2267 ) ;
#34853 = DIRECTION ( 'NONE',  ( -3.071710424422018668E-17, 6.404604876783312462E-16, 1.000000000000000000 ) ) ;
#34854 = ORIENTED_EDGE ( 'NONE', *, *, #19032, .T. ) ;
#34855 = CARTESIAN_POINT ( 'NONE',  ( -12.18170072908086965, -10.17053062278287889, 64.32914326641392222 ) ) ;
#34856 = CARTESIAN_POINT ( 'NONE',  ( -16.79771060966972129, -22.23299631151009237, 68.85594001288120580 ) ) ;
#34857 = ORIENTED_EDGE ( 'NONE', *, *, #4934, .F. ) ;
#34858 = DIRECTION ( 'NONE',  ( -3.071710424422018668E-17, 6.404604876783312462E-16, 1.000000000000000000 ) ) ;
#34859 = FACE_BOUND ( 'NONE', #24574, .T. ) ;
#34860 = ORIENTED_EDGE ( 'NONE', *, *, #36793, .F. ) ;
#34861 = ORIENTED_EDGE ( 'NONE', *, *, #47788, .T. ) ;
#34862 = ORIENTED_EDGE ( 'NONE', *, *, #33432, .F. ) ;
#34863 = DIRECTION ( 'NONE',  ( -0.1240347345892086062, 1.145860353393066553E-16, -0.9922778767136676281 ) ) ;
#34864 = CARTESIAN_POINT ( 'NONE',  ( -15.97409385759799072, -6.859212275519751323, 50.50378509014259265 ) ) ;
#34865 = CARTESIAN_POINT ( 'NONE',  ( -14.56922802208840828, -8.416425255985021892, 67.48804881135004052 ) ) ;
#34866 = CARTESIAN_POINT ( 'NONE',  ( -11.86332896968958650, -9.851264934370021820, 64.13640162903247699 ) ) ;
#34867 = CARTESIAN_POINT ( 'NONE',  ( -11.12358174778395714, -11.75903488045733347, 71.38860871064898106 ) ) ;
#34868 = ORIENTED_EDGE ( 'NONE', *, *, #42768, .T. ) ;
#34869 = EDGE_LOOP ( 'NONE', ( #27762, #28226, #37942, #6160 ) ) ;
#34870 = CARTESIAN_POINT ( 'NONE',  ( -21.31784385650551883, -9.790100578890868377, 49.79778022625163203 ) ) ;
#34871 = FACE_OUTER_BOUND ( 'NONE', #48633, .T. ) ;
#34872 = CARTESIAN_POINT ( 'NONE',  ( -21.81933826130772047, -16.43558560955401404, 49.52966884056655772 ) ) ;
#34873 = DIRECTION ( 'NONE',  ( 5.854827030937197869E-31, 1.020425574103664912E-16, 1.000000000000000000 ) ) ;
#34874 = ORIENTED_EDGE ( 'NONE', *, *, #7641, .T. ) ;
#34875 = EDGE_CURVE ( 'NONE', #40518, #22263, #33582, .T. ) ;
#34876 = CARTESIAN_POINT ( 'NONE',  ( -12.97364361214796347, -9.395187332399693503, 49.41428126932424192 ) ) ;
#34877 = ORIENTED_EDGE ( 'NONE', *, *, #5491, .T. ) ;
#34878 = CARTESIAN_POINT ( 'NONE',  ( -45.92409385541306222, -14.38986189584960051, 70.50000000000000000 ) ) ;
#34879 = EDGE_CURVE ( 'NONE', #13129, #33825, #33308, .T. ) ;
#34880 = CARTESIAN_POINT ( 'NONE',  ( -19.11145557798581152, -7.964112677450091660, 63.73089235102099792 ) ) ;
#34881 = CIRCLE ( 'NONE', #6561, 5.249999999999998224 ) ;
#34882 = DIRECTION ( 'NONE',  ( 0.000000000000000000, 0.000000000000000000, 1.000000000000000000 ) ) ;
#34883 =( BOUNDED_CURVE ( )  B_SPLINE_CURVE ( 3, ( #18966, #34455, #15487, #30552 ),
 .UNSPECIFIED., .F., .F. ) 
 B_SPLINE_CURVE_WITH_KNOTS ( ( 4, 4 ),
 ( 0.5000000000000000000, 0.9074455897393663983 ),
 .UNSPECIFIED. ) 
 CURVE ( )  GEOMETRIC_REPRESENTATION_ITEM ( )  RATIONAL_B_SPLINE_CURVE ( ( 1.000000000000010658, 0.4567392136813307468, 0.3561768502900223843, 0.6983129098260969503 ) ) 
 REPRESENTATION_ITEM ( '' )  );
#34884 = ORIENTED_EDGE ( 'NONE', *, *, #36789, .F. ) ;
#34885 = CARTESIAN_POINT ( 'NONE',  ( -16.52316554273587101, -21.80170452179945073, 65.24036514508233608 ) ) ;
#34886 = CARTESIAN_POINT ( 'NONE',  ( -21.61813339613238227, -8.651787399021619862, 73.71633365192373333 ) ) ;
#34887 = CARTESIAN_POINT ( 'NONE',  ( -10.42892955798469323, -14.54578234806194992, 67.85800118616361942 ) ) ;
#34888 = DIRECTION ( 'NONE',  ( -9.637352644315596475E-17, 0.000000000000000000, -1.000000000000000000 ) ) ;
#34889 = EDGE_CURVE ( 'NONE', #29740, #27105, #31748, .T. ) ;
#34890 = ORIENTED_EDGE ( 'NONE', *, *, #37765, .T. ) ;
#34891 = CARTESIAN_POINT ( 'NONE',  ( -10.45256745270239307, -15.43993597667916795, 57.86792809192976961 ) ) ;
#34892 = ADVANCED_FACE ( 'NONE', ( #24455 ), #35514, .T. ) ;
#34893 = CARTESIAN_POINT ( 'NONE',  ( -21.34581862946232889, -20.66775363590295456, 72.52446429492310642 ) ) ;
#34894 = CARTESIAN_POINT ( 'NONE',  ( -12.35838514372898800, -20.27197932131825198, 68.44383270345304027 ) ) ;
#34895 = ORIENTED_EDGE ( 'NONE', *, *, #16754, .T. ) ;
#34896 = CARTESIAN_POINT ( 'NONE',  ( -10.02134419679888211, -13.96483583313674615, 61.10476640098193002 ) ) ;
#34897 =( BOUNDED_CURVE ( )  B_SPLINE_CURVE ( 3, ( #12821, #34980, #12583, #20211 ),
 .UNSPECIFIED., .F., .F. ) 
 B_SPLINE_CURVE_WITH_KNOTS ( ( 4, 4 ),
 ( 0.5000000000000000000, 0.9074455897393671755 ),
 .UNSPECIFIED. ) 
 CURVE ( )  GEOMETRIC_REPRESENTATION_ITEM ( )  RATIONAL_B_SPLINE_CURVE ( ( 0.9999999999999841238, 0.4567392136813330783, 0.3561768502900416467, 0.6983129098260927314 ) ) 
 REPRESENTATION_ITEM ( '' )  );
#34898 = VERTEX_POINT ( 'NONE', #28129 ) ;
#34899 = LINE ( 'NONE', #16666, #24245 ) ;
#34900 = CARTESIAN_POINT ( 'NONE',  ( -14.86477050248655551, -7.812526586475418533, 57.10645908473438226 ) ) ;
#34901 = EDGE_CURVE ( 'NONE', #43456, #15655, #45985, .T. ) ;
#34902 = ORIENTED_EDGE ( 'NONE', *, *, #36858, .T. ) ;
#34903 = CARTESIAN_POINT ( 'NONE',  ( -13.07136655094769750, -8.762923122256669473, 64.02451139116674028 ) ) ;
#34904 = CARTESIAN_POINT ( 'NONE',  ( -18.32857646159318676, -22.20418385865972155, 68.93019298464047040 ) ) ;
#34905 = LINE ( 'NONE', #8578, #17883 ) ;
#34906 = DIRECTION ( 'NONE',  ( 2.210955087992717862E-06, -1.097707075699772489E-06, 0.9999999999969533260 ) ) ;
#34907 = ORIENTED_EDGE ( 'NONE', *, *, #25702, .F. ) ;
#34908 = CARTESIAN_POINT ( 'NONE',  ( -9.996284180359110039, -14.23299000612383303, 64.51086969714638997 ) ) ;
#34909 = EDGE_CURVE ( 'NONE', #12927, #45073, #20984, .T. ) ;
#34910 = CARTESIAN_POINT ( 'NONE',  ( -22.36602013069261119, -13.03724021049843351, 49.52966884056655772 ) ) ;
#34911 = FACE_OUTER_BOUND ( 'NONE', #27703, .T. ) ;
#34912 = CARTESIAN_POINT ( 'NONE',  ( -10.49189908542464700, -16.09426454567519116, 68.26295692486267797 ) ) ;
#34913 = EDGE_LOOP ( 'NONE', ( #47161, #4626, #2907, #22362, #43325 ) ) ;
#34914 = DIRECTION ( 'NONE',  ( 0.9271861211590526342, 0.3746009833543293421, -1.005599061620490611E-08 ) ) ;
#34915 = AXIS2_PLACEMENT_3D ( 'NONE', #48483, #15468, #44564 ) ;
#34916 = CARTESIAN_POINT ( 'NONE',  ( -21.79997194174348607, -9.271457673084677609, 70.27565669584988939 ) ) ;
#34917 = AXIS2_PLACEMENT_3D ( 'NONE', #29642, #37011, #18296 ) ;
#34918 = EDGE_LOOP ( 'NONE', ( #12930, #30279, #45234, #32269 ) ) ;
#34919 = ORIENTED_EDGE ( 'NONE', *, *, #40667, .F. ) ;
#34920 = CARTESIAN_POINT ( 'NONE',  ( -22.80992383800762724, -10.33718617846504273, 66.82565708633600821 ) ) ;
#34921 = CARTESIAN_POINT ( 'NONE',  ( -24.09792889798371007, -17.08130376423426000, 73.18336032035891492 ) ) ;
#34922 = CARTESIAN_POINT ( 'NONE',  ( -11.22150886908280931, -18.16670198096008093, 58.22203402163793839 ) ) ;
#34923 = CARTESIAN_POINT ( 'NONE',  ( -20.78034385650551386, -6.424090610841174609, 49.80797279389977916 ) ) ;
#34924 = CARTESIAN_POINT ( 'NONE',  ( -24.17899278864585355, -11.66673636667039027, 59.66731167108189737 ) ) ;
#34925 = DIRECTION ( 'NONE',  ( -2.866981220435666553E-17, 1.000000000000000000, 1.190614954331866791E-16 ) ) ;
#34926 = CARTESIAN_POINT ( 'NONE',  ( -19.70639647806698136, -21.90109437720271757, 65.57990800639531415 ) ) ;
#34927 = CARTESIAN_POINT ( 'NONE',  ( -23.75797280549784318, -17.78947120508452429, 59.30378417803890301 ) ) ;
#34928 = ORIENTED_EDGE ( 'NONE', *, *, #23324, .T. ) ;
#34929 = ORIENTED_EDGE ( 'NONE', *, *, #25506, .F. ) ;
#34930 = CARTESIAN_POINT ( 'NONE',  ( -11.25339550917664333, -11.39346175823023088, 60.56396915994215391 ) ) ;
#34931 =( NAMED_UNIT ( * ) PLANE_ANGLE_UNIT ( ) SI_UNIT ( $, .RADIAN. ) );
#34932 = CARTESIAN_POINT ( 'NONE',  ( -14.90085577400961014, -10.20532018813695707, 52.02966884056656482 ) ) ;
#34933 = CARTESIAN_POINT ( 'NONE',  ( -13.54792730259346456, -8.920061342218058797, 57.25495614889487683 ) ) ;
#34934 = CARTESIAN_POINT ( 'NONE',  ( -40.92409385541305511, -14.80920654474410725, 74.99999999999998579 ) ) ;
#34935 = ADVANCED_FACE ( 'NONE', ( #35742 ), #5740, .F. ) ;
#34936 = ORIENTED_EDGE ( 'NONE', *, *, #40027, .T. ) ;
#34937 = CYLINDRICAL_SURFACE ( 'NONE', #2085, 1.999999999999999556 ) ;
#34938 = CARTESIAN_POINT ( 'NONE',  ( -24.86242989439883289, -14.39095395922188558, 66.36788051138485400 ) ) ;
#34939 = DIRECTION ( 'NONE',  ( 0.000000000000000000, -0.9999954153791273948, -0.003028072113819838245 ) ) ;
#34940 = CARTESIAN_POINT ( 'NONE',  ( -15.83004105235379022, -7.531612319186171689, 67.26290417877635264 ) ) ;
#34941 = EDGE_LOOP ( 'NONE', ( #11752, #40022, #43926, #6667, #6776 ) ) ;
#34942 = CARTESIAN_POINT ( 'NONE',  ( -21.94242186726961208, -9.397052521110282441, 60.00699132926281010 ) ) ;
#34943 = CARTESIAN_POINT ( 'NONE',  ( -19.30271816048872324, -8.014114901043837946, 60.26092997144683494 ) ) ;
#34944 = VECTOR ( 'NONE', #17534, 1000.000000000000000 ) ;
#34945 = ORIENTED_EDGE ( 'NONE', *, *, #1089, .F. ) ;
#34946 = EDGE_CURVE ( 'NONE', #1752, #29174, #25468, .T. ) ;
#34947 = CARTESIAN_POINT ( 'NONE',  ( -14.63779949229408750, -10.05162950738736072, 53.69233794759168887 ) ) ;
#34948 = CARTESIAN_POINT ( 'NONE',  ( -22.17450858901738897, -19.95071429852638545, 66.00421734751543568 ) ) ;
#34949 = VERTEX_POINT ( 'NONE', #24921 ) ;
#34950 = CARTESIAN_POINT ( 'NONE',  ( -13.11945872550529657, -9.225962324091906197, 67.67942785705487552 ) ) ;
#34951 = ORIENTED_EDGE ( 'NONE', *, *, #42956, .F. ) ;
#34952 = DIRECTION ( 'NONE',  ( 0.1571515419521612722, -0.9875744999047174622, 7.433889655140131751E-08 ) ) ;
#34953 = EDGE_CURVE ( 'NONE', #29256, #23803, #45933, .T. ) ;
#34954 = CARTESIAN_POINT ( 'NONE',  ( -45.92409385541306222, 12.69079345525585545, 70.50000000000000000 ) ) ;
#34955 = ORIENTED_EDGE ( 'NONE', *, *, #20168, .T. ) ;
#34956 = CARTESIAN_POINT ( 'NONE',  ( -23.80175822008580866, -17.82088921309938812, 62.88849600917846061 ) ) ;
#34957 = DIRECTION ( 'NONE',  ( 0.6607190350373965959, 0.7506333037770516192, 0.000000000000000000 ) ) ;
#34958 = CARTESIAN_POINT ( 'NONE',  ( -17.94284385650551528, -8.811426318492348031, 52.18089403414751359 ) ) ;
#34959 = CARTESIAN_POINT ( 'NONE',  ( -15.06075745000970834, -21.87520294740874149, 68.76248218113177302 ) ) ;
#34960 = ADVANCED_FACE ( 'NONE', ( #31588 ), #3449, .T. ) ;
#34961 = B_SPLINE_CURVE_WITH_KNOTS ( 'NONE', 3,
 ( #47568, #13566, #13326, #39453 ),
 .UNSPECIFIED., .F., .F.,
 ( 4, 4 ),
 ( 0.001041996463599131851, 0.002493317452641904963 ),
 .UNSPECIFIED. ) ;
#34962 = CARTESIAN_POINT ( 'NONE',  ( -19.80886856394220175, -10.13209743873032309, 49.52966884056655772 ) ) ;
#34963 = DIRECTION ( 'NONE',  ( 0.000000000000000000, 0.000000000000000000, 1.000000000000000000 ) ) ;
#34964 = VERTEX_POINT ( 'NONE', #42681 ) ;
#34965 = LINE ( 'NONE', #2206, #6628 ) ;
#34966 = CARTESIAN_POINT ( 'NONE',  ( -18.69178539469224987, -19.32099559247695097, 52.02966884056656482 ) ) ;
#34967 = CARTESIAN_POINT ( 'NONE',  ( -14.60479643987598841, -7.913168514039711887, 60.50491717424539218 ) ) ;
#34968 = CARTESIAN_POINT ( 'NONE',  ( -24.59325023630216833, -12.78233532962698682, 66.46280073947134781 ) ) ;
#34969 = CARTESIAN_POINT ( 'NONE',  ( -12.55411140858086760, -19.90724249994213935, 65.15202838036978505 ) ) ;
#34970 = VERTEX_POINT ( 'NONE', #24202 ) ;
#34971 = VERTEX_POINT ( 'NONE', #28850 ) ;
#34972 = CARTESIAN_POINT ( 'NONE',  ( -21.31800492490012999, -20.62620369199774117, 72.52446429884872714 ) ) ;
#34973 = ORIENTED_EDGE ( 'NONE', *, *, #38886, .F. ) ;
#34974 = CARTESIAN_POINT ( 'NONE',  ( -24.12651600458584511, -12.62191667979047338, 73.25697658996379857 ) ) ;
#34975 = CARTESIAN_POINT ( 'NONE',  ( -15.19396558280303822, -21.91766586989539434, 68.61946996636811491 ) ) ;
#34976 = CARTESIAN_POINT ( 'NONE',  ( -10.27127829932231862, -12.72555322402984146, 64.44552998452087422 ) ) ;
#34977 = DIRECTION ( 'NONE',  ( -0.1240347345892086062, 1.145860353393066553E-16, -0.9922778767136676281 ) ) ;
#34978 = EDGE_CURVE ( 'NONE', #40830, #5810, #38644, .T. ) ;
#34979 = CARTESIAN_POINT ( 'NONE',  ( -11.06939607882469190, -17.86905163984256006, 71.45229597776977926 ) ) ;
#34980 = CARTESIAN_POINT ( 'NONE',  ( -10.89363166428750773, -17.47500997361330022, 71.65898155907456157 ) ) ;
#34981 = DIRECTION ( 'NONE',  ( 0.9986807914369958405, -0.05134858142905002198, 1.286972170232540014E-09 ) ) ;
#34982 = EDGE_CURVE ( 'NONE', #748, #36010, #41825, .T. ) ;
#34983 = VECTOR ( 'NONE', #20410, 1000.000000000000114 ) ;
#34984 = ORIENTED_EDGE ( 'NONE', *, *, #24493, .F. ) ;
#34985 = CARTESIAN_POINT ( 'NONE',  ( -22.68646401470678953, -20.08284273627726435, 69.35913316877790180 ) ) ;
#34986 = EDGE_CURVE ( 'NONE', #26512, #29684, #23665, .T. ) ;
#34987 = AXIS2_PLACEMENT_3D ( 'NONE', #15149, #3859, #11240 ) ;
#34988 = CARTESIAN_POINT ( 'NONE',  ( -17.42409385541299471, -14.80920654474434883, 62.02966884056656482 ) ) ;
#34989 = CARTESIAN_POINT ( 'NONE',  ( -22.51638425468451743, -9.928425624739869448, 70.21998462585445111 ) ) ;
#34990 = CARTESIAN_POINT ( 'NONE',  ( -17.72591277652480812, -7.814435863317398479, 63.77886828924947338 ) ) ;
#34991 = CARTESIAN_POINT ( 'NONE',  ( -17.39742496553465401, -7.759256980052345654, 67.02039592192090822 ) ) ;
#34992 = B_SPLINE_CURVE_WITH_KNOTS ( 'NONE', 3,
 ( #17291, #24707, #32336, #9921, #42695, #2040, #6225, #1556, #32086, #12876 ),
 .UNSPECIFIED., .F., .F.,
 ( 4, 2, 2, 2, 4 ),
 ( 0.6272669072878003238, 0.7522669073073093848, 0.8772669073268185569, 1.002266907346327729, 1.127266907365836790 ),
 .UNSPECIFIED. ) ;
#34993 = ORIENTED_EDGE ( 'NONE', *, *, #7623, .T. ) ;
#34994 = ORIENTED_EDGE ( 'NONE', *, *, #3386, .F. ) ;
#34995 = CARTESIAN_POINT ( 'NONE',  ( -21.68034385650551599, -6.424090610841174609, 49.80797279389977916 ) ) ;
#34996 = ORIENTED_EDGE ( 'NONE', *, *, #45905, .T. ) ;
#34997 = B_SPLINE_CURVE_WITH_KNOTS ( 'NONE', 3,
 ( #24626, #31758, #20440, #42847, #36158, #47013, #28054, #2678, #39136, #5419 ),
 .UNSPECIFIED., .F., .F.,
 ( 4, 2, 2, 2, 4 ),
 ( 0.1272669073658367345, 0.2522669073463192357, 0.3772669073268017925, 0.5022669073072842938, 0.6272669072877667951 ),
 .UNSPECIFIED. ) ;
#34998 = CARTESIAN_POINT ( 'NONE',  ( -11.17943887680513981, -18.87220427245064513, 65.00353025264104190 ) ) ;
#34999 = CARTESIAN_POINT ( 'NONE',  ( -11.00006132919183521, -18.58228645891882280, 57.92901817424456112 ) ) ;
#35000 = ORIENTED_EDGE ( 'NONE', *, *, #41291, .F. ) ;
#35001 = DIRECTION ( 'NONE',  ( 1.224646799147353207E-16, 1.000000000000000000, -1.912410701131276611E-32 ) ) ;
#35002 = CARTESIAN_POINT ( 'NONE',  ( -15.56465948913147557, -7.543361525925788236, 54.27966884056655061 ) ) ;
#35003 = VERTEX_POINT ( 'NONE', #33485 ) ;
#35004 = CARTESIAN_POINT ( 'NONE',  ( -14.11063322135152909, -21.03236308526469855, 72.21135587486895702 ) ) ;
#35005 = DIRECTION ( 'NONE',  ( -0.9956360040033419567, 0.09332174201255245827, 0.000000000000000000 ) ) ;
#35006 = ORIENTED_EDGE ( 'NONE', *, *, #36287, .F. ) ;
#35007 = CARTESIAN_POINT ( 'NONE',  ( -10.83683315258895519, -12.44108567723101899, 57.32857332099802505 ) ) ;
#35008 = CARTESIAN_POINT ( 'NONE',  ( -13.54546414475118610, -21.17012168889900181, 65.14662202029667526 ) ) ;
#35009 = B_SPLINE_CURVE_WITH_KNOTS ( 'NONE', 1,
 ( #21246, #18494 ),
 .UNSPECIFIED., .F., .F.,
 ( 2, 2 ),
 ( 0.000000000000000000, 1.000000000000000000 ),
 .UNSPECIFIED. ) ;
#35010 = ORIENTED_EDGE ( 'NONE', *, *, #4048, .T. ) ;
#35011 = CARTESIAN_POINT ( 'NONE',  ( -23.08487763607990928, -19.01185175973044039, 62.36879011380454330 ) ) ;
#35012 = CARTESIAN_POINT ( 'NONE',  ( -16.71957921250844592, -21.82421608262117729, 68.71032757591046902 ) ) ;
#35013 = EDGE_CURVE ( 'NONE', #33357, #39181, #46846, .T. ) ;
#35014 = CARTESIAN_POINT ( 'NONE',  ( -19.56272746357835501, -21.53536514712069305, 58.68074270823246508 ) ) ;
#35015 = ORIENTED_EDGE ( 'NONE', *, *, #41247, .T. ) ;
#35016 = DIRECTION ( 'NONE',  ( 2.081668171172170091E-15, 0.000000000000000000, -1.000000000000000000 ) ) ;
#35017 = AXIS2_PLACEMENT_3D ( 'NONE', #16860, #27476, #8783 ) ;
#35018 = CARTESIAN_POINT ( 'NONE',  ( -21.99213670719075253, -20.17946569659695655, 59.04970794435396897 ) ) ;
#35019 =( BOUNDED_SURFACE ( )  B_SPLINE_SURFACE ( 3, 1, ( 
 ( #24333, #9566 ),
 ( #38355, #46506 ),
 ( #12984, #46970 ),
 ( #955, #16918 ),
 ( #5137, #20145 ),
 ( #46015, #13215 ),
 ( #27293, #4899 ) ),
 .UNSPECIFIED., .T., .F., .F. ) 
 B_SPLINE_SURFACE_WITH_KNOTS ( ( 4, 3, 4 ),
 ( 2, 2 ),
 ( 0.000000000000000000, 0.5000000000000000000, 1.000000000000000000 ),
 ( 0.000000000000000000, 1.000000000000000000 ),
 .UNSPECIFIED. ) 
 GEOMETRIC_REPRESENTATION_ITEM ( )  RATIONAL_B_SPLINE_SURFACE ( (
 ( 1.000000000000000000, 1.000000000000000000),
 ( 0.3333333333333335369, 0.3333333333333330373),
 ( 0.3333333333333335369, 0.3333333333333330373),
 ( 1.000000000000000000, 1.000000000000000000),
 ( 0.3333333333333333703, 0.3333333333333333703),
 ( 0.3333333333333333703, 0.3333333333333333703),
 ( 1.000000000000000000, 1.000000000000000000) ) ) 
 REPRESENTATION_ITEM ( '' )  SURFACE ( )  );
#35020 = FACE_OUTER_BOUND ( 'NONE', #47984, .T. ) ;
#35021 = CARTESIAN_POINT ( 'NONE',  ( -24.08517543038346531, -12.49907855475201579, 73.52753481283211556 ) ) ;
#35022 = CARTESIAN_POINT ( 'NONE',  ( -14.94170459844064780, -18.78425696289860269, 49.52966884056656482 ) ) ;
#35023 = DIRECTION ( 'NONE',  ( -1.616182858256118783E-16, -0.003028072113822189229, 0.9999954153791275058 ) ) ;
#35024 = CARTESIAN_POINT ( 'NONE',  ( -11.01197672498281044, -17.74032467813711733, 71.85246142747087106 ) ) ;
#35025 = CARTESIAN_POINT ( 'NONE',  ( -12.07742570852865427, -19.41007429933622319, 58.22682412763990811 ) ) ;
#35026 = DIRECTION ( 'NONE',  ( 0.5097212845717493668, -0.8603395911234852367, 0.000000000000000000 ) ) ;
#35027 = CARTESIAN_POINT ( 'NONE',  ( -16.73034385650551670, -9.794322478646142471, 51.19202720610083190 ) ) ;
#35028 = EDGE_LOOP ( 'NONE', ( #5462, #3834, #43764, #33648, #29647 ) ) ;
#35029 = LINE ( 'NONE', #42445, #43230 ) ;
#35030 = CARTESIAN_POINT ( 'NONE',  ( -11.81042834955647258, -10.54382735031610174, 74.45357240259568243 ) ) ;
#35031 = ORIENTED_EDGE ( 'NONE', *, *, #11322, .T. ) ;
#35032 = CARTESIAN_POINT ( 'NONE',  ( -23.27284462870851911, -18.74605969774991010, 66.10917289053097079 ) ) ;
#35033 = CARTESIAN_POINT ( 'NONE',  ( -15.01062035279700346, -21.85762174227016885, 65.26630065318278184 ) ) ;
#35034 = CARTESIAN_POINT ( 'NONE',  ( -21.39967327233876659, -20.63170314183283693, 72.80974286114339122 ) ) ;
#35035 = CARTESIAN_POINT ( 'NONE',  ( -23.25220530991251167, -10.16847870644612328, 63.26524311255320043 ) ) ;
#35036 = DIRECTION ( 'NONE',  ( 3.549360974554993999E-17, -6.371834667797928663E-18, -1.000000000000000000 ) ) ;
#35037 =( BOUNDED_CURVE ( )  B_SPLINE_CURVE ( 3, ( #5197, #24152, #43359, #27836 ),
 .UNSPECIFIED., .F., .F. ) 
 B_SPLINE_CURVE_WITH_KNOTS ( ( 4, 4 ),
 ( 4.712388980384690562, 4.921828490624008623 ),
 .UNSPECIFIED. ) 
 CURVE ( )  GEOMETRIC_REPRESENTATION_ITEM ( )  RATIONAL_B_SPLINE_CURVE ( ( 1.000000000000000000, 0.9963479302455156006, 0.9963479302455156006, 1.000000000000000000 ) ) 
 REPRESENTATION_ITEM ( '' )  );
#35038 = ORIENTED_EDGE ( 'NONE', *, *, #22508, .F. ) ;
#35039 =( BOUNDED_CURVE ( )  B_SPLINE_CURVE ( 3, ( #18407, #11521, #7361, #34159 ),
 .UNSPECIFIED., .F., .F. ) 
 B_SPLINE_CURVE_WITH_KNOTS ( ( 4, 4 ),
 ( 0.4074455897393624015, 0.5000000000000000000 ),
 .UNSPECIFIED. ) 
 CURVE ( )  GEOMETRIC_REPRESENTATION_ITEM ( )  RATIONAL_B_SPLINE_CURVE ( ( 0.6983129098260958401, 0.7760317562606984243, 0.8765941196519991818, 0.9999999999999965583 ) ) 
 REPRESENTATION_ITEM ( '' )  );
#35040 = CARTESIAN_POINT ( 'NONE',  ( -23.71873315273824545, -11.74668173045760433, 63.25218284853021089 ) ) ;
#35041 = EDGE_CURVE ( 'NONE', #45990, #46544, #7190, .T. ) ;
#35042 = CARTESIAN_POINT ( 'NONE',  ( -20.70466284777608124, -8.568939270112290174, 60.14125232065403992 ) ) ;
#35043 = CARTESIAN_POINT ( 'NONE',  ( -10.08184786930872789, -16.07202671437600117, 68.08493695327037187 ) ) ;
#35044 = EDGE_CURVE ( 'NONE', #47460, #20025, #47804, .T. ) ;
#35045 = EDGE_CURVE ( 'NONE', #22219, #13885, #8181, .T. ) ;
#35046 = ORIENTED_EDGE ( 'NONE', *, *, #3935, .T. ) ;
#35047 = CARTESIAN_POINT ( 'NONE',  ( -23.96075626263749569, -17.45014286185010732, 66.24357239682277054 ) ) ;
#35048 = CYLINDRICAL_SURFACE ( 'NONE', #40528, 4.686499999999997002 ) ;
#35049 = CARTESIAN_POINT ( 'NONE',  ( -18.34560609025200861, -9.386954687716537293, 53.49999999999995026 ) ) ;
#35050 = CARTESIAN_POINT ( 'NONE',  ( -10.13258936719380898, -16.33817337277914561, 71.63245765104117879 ) ) ;
#35051 = CARTESIAN_POINT ( 'NONE',  ( -46.29409385541305255, -12.76354662275040219, 69.95698270748289360 ) ) ;
#35052 =( BOUNDED_CURVE ( )  B_SPLINE_CURVE ( 3, ( #3244, #7443, #7202, #3482 ),
 .UNSPECIFIED., .F., .F. ) 
 B_SPLINE_CURVE_WITH_KNOTS ( ( 4, 4 ),
 ( 0.4074455897279072869, 0.5000000000000000000 ),
 .UNSPECIFIED. ) 
 CURVE ( )  GEOMETRIC_REPRESENTATION_ITEM ( )  RATIONAL_B_SPLINE_CURVE ( ( 0.6983129097972519128, 0.7760317562358295396, 0.8765941196367486032, 1.000000000000016209 ) ) 
 REPRESENTATION_ITEM ( '' )  );
#35053 = ORIENTED_EDGE ( 'NONE', *, *, #43086, .F. ) ;
#35054 = ORIENTED_EDGE ( 'NONE', *, *, #46589, .F. ) ;
#35055 = CARTESIAN_POINT ( 'NONE',  ( -21.90534385541304374, -7.595227055684746986, 51.75156210489594599 ) ) ;
#35056 = CARTESIAN_POINT ( 'NONE',  ( -19.85909577874797449, -21.37257635846961890, 72.46322212860958700 ) ) ;
#35057 = DIRECTION ( 'NONE',  ( -0.6323592902076723421, -0.7746752403995151859, 4.984538757074985308E-08 ) ) ;
#35058 = PRODUCT_DEFINITION_SHAPE ( 'NONE', 'NONE',  #29471 ) ;
#35059 = CARTESIAN_POINT ( 'NONE',  ( -45.92409385541306932, -16.70920654474410938, 70.50000000000000000 ) ) ;
#35060 = EDGE_CURVE ( 'NONE', #47966, #32808, #47431, .T. ) ;
#35061 = CARTESIAN_POINT ( 'NONE',  ( -10.59656512619885227, -13.05092609425065220, 68.02360230423869325 ) ) ;
#35062 = CARTESIAN_POINT ( 'NONE',  ( -13.91686182480500200, -8.236299899141551251, 74.31459327626868117 ) ) ;
#35063 = CARTESIAN_POINT ( 'NONE',  ( -23.95986381193147707, -17.46034710541827906, 69.82828398331871256 ) ) ;
#35064 = EDGE_LOOP ( 'NONE', ( #14328, #41265, #6880, #29855, #35828 ) ) ;
#35065 = CARTESIAN_POINT ( 'NONE',  ( -24.12016595861979695, -18.07666464397348349, 59.19033703419022885 ) ) ;
#35066 = CARTESIAN_POINT ( 'NONE',  ( -17.15681831196262408, -7.812702829301893637, 74.14945326254591862 ) ) ;
#35067 = VERTEX_POINT ( 'NONE', #17517 ) ;
#35068 = DIRECTION ( 'NONE',  ( -5.224165706511165539E-06, 4.853367013834837651E-07, 0.9999999999862362321 ) ) ;
#35069 = DIRECTION ( 'NONE',  ( 1.000000000000000000, 2.866981220435666553E-17, 0.000000000000000000 ) ) ;
#35070 = ORIENTED_EDGE ( 'NONE', *, *, #19799, .F. ) ;
#35071 = CARTESIAN_POINT ( 'NONE',  ( -16.75933984047804515, -20.01695097968237036, 52.02966884056656482 ) ) ;
#35072 = CARTESIAN_POINT ( 'NONE',  ( -10.00186344861280396, -15.45246920467748275, 57.67518653529428718 ) ) ;
#35073 = ADVANCED_FACE ( 'NONE', ( #6457 ), #25405, .T. ) ;
#35074 = CARTESIAN_POINT ( 'NONE',  ( -21.69457540385530336, -9.196023516753362159, 70.54621400560100142 ) ) ;
#35075 = CARTESIAN_POINT ( 'NONE',  ( -19.52323420048857372, -8.075080386471409355, 60.26093179093862062 ) ) ;
#35076 = ORIENTED_EDGE ( 'NONE', *, *, #29806, .T. ) ;
#35077 = CARTESIAN_POINT ( 'NONE',  ( -18.60622096112062707, -22.16490860957766529, 72.47006221837980888 ) ) ;
#35078 = FACE_OUTER_BOUND ( 'NONE', #32416, .T. ) ;
#35079 = DIRECTION ( 'NONE',  ( -0.9271861211590526342, -0.3746009833543293421, 1.005599061620507320E-08 ) ) ;
#35080 = VECTOR ( 'NONE', #9549, 1000.000000000000000 ) ;
#35081 = AXIS2_PLACEMENT_3D ( 'NONE', #8250, #4535, #27681 ) ;
#35082 = DIRECTION ( 'NONE',  ( -3.071710424422018668E-17, 6.404604876783312462E-16, 1.000000000000000000 ) ) ;
#35083 = CARTESIAN_POINT ( 'NONE',  ( 0.000000000000000000, 0.000000000000000000, 0.000000000000000000 ) ) ;
#35084 = PLANE ( 'NONE',  #32108 ) ;
#35085 = CARTESIAN_POINT ( 'NONE',  ( -17.33262245845742910, -7.759502110702281463, 67.30567542699309058 ) ) ;
#35086 = CARTESIAN_POINT ( 'NONE',  ( -45.55409385541306477, -12.70920654474410760, 71.79999999999999716 ) ) ;
#35087 = ORIENTED_EDGE ( 'NONE', *, *, #43826, .T. ) ;
#35088 = CARTESIAN_POINT ( 'NONE',  ( -10.69329545470549547, -12.88639875208188634, 64.28338539888954983 ) ) ;
#35089 = EDGE_LOOP ( 'NONE', ( #1078, #25116, #15230, #17457, #40334 ) ) ;
#35090 = CARTESIAN_POINT ( 'NONE',  ( -7.924093855413070209, -6.359206544744109735, 52.99999999999997868 ) ) ;
#35091 = CARTESIAN_POINT ( 'NONE',  ( -13.18109041692693140, -9.241580129719441317, 67.37942828297590836 ) ) ;
#35092 = ORIENTED_EDGE ( 'NONE', *, *, #2789, .T. ) ;
#35093 = CARTESIAN_POINT ( 'NONE',  ( -22.88419851978063591, -10.42888047092867865, 63.07185995612697837 ) ) ;
#35094 = FACE_BOUND ( 'NONE', #29243, .T. ) ;
#35095 = ORIENTED_EDGE ( 'NONE', *, *, #15766, .T. ) ;
#35096 = EDGE_CURVE ( 'NONE', #41338, #2641, #21311, .T. ) ;
#35097 = EDGE_CURVE ( 'NONE', #27032, #47884, #27745, .T. ) ;
#35098 = EDGE_LOOP ( 'NONE', ( #3061, #13875 ) ) ;
#35099 = ORIENTED_EDGE ( 'NONE', *, *, #2776, .F. ) ;
#35100 = CARTESIAN_POINT ( 'NONE',  ( -10.03860189133040315, -15.79316336790978603, 61.15133701675058120 ) ) ;
#35101 = DIRECTION ( 'NONE',  ( -0.4332512900281776380, 0.1108752438054599471, 0.8944271909999157444 ) ) ;
#35102 = CARTESIAN_POINT ( 'NONE',  ( -22.82021534226488413, -10.26644114900146576, 70.31178585817200144 ) ) ;
#35103 = CARTESIAN_POINT ( 'NONE',  ( -10.57136597998982985, -13.11950654315977793, 64.42403173677416817 ) ) ;
#35104 = CARTESIAN_POINT ( 'NONE',  ( -13.34436364135905606, -9.120990523779875403, 60.63053345639304581 ) ) ;
#35105 = ORIENTED_EDGE ( 'NONE', *, *, #2535, .T. ) ;
#35106 = ORIENTED_EDGE ( 'NONE', *, *, #3104, .F. ) ;
#35107 = EDGE_CURVE ( 'NONE', #43552, #2873, #42507, .T. ) ;
#35108 = EDGE_CURVE ( 'NONE', #39476, #10157, #37687, .T. ) ;
#35109 = DIRECTION ( 'NONE',  ( 0.9687793358424819923, -0.2479245821708678243, 0.000000000000000000 ) ) ;
#35110 = EDGE_CURVE ( 'NONE', #8273, #33946, #22688, .T. ) ;
#35111 = CARTESIAN_POINT ( 'NONE',  ( -22.61838138049972358, -19.58773617554900071, 69.32985287095068827 ) ) ;
#35112 = CARTESIAN_POINT ( 'NONE',  ( -23.12302852889637705, -18.95946475466559633, 62.65406880579606508 ) ) ;
#35113 = CYLINDRICAL_SURFACE ( 'NONE', #15097, 0.1499999999999991063 ) ;
#35114 = EDGE_CURVE ( 'NONE', #13421, #23075, #2825, .T. ) ;
#35115 = ORIENTED_EDGE ( 'NONE', *, *, #44212, .F. ) ;
#35116 = CARTESIAN_POINT ( 'NONE',  ( -22.33034385650551812, -9.794322478646142471, 51.19202720610083901 ) ) ;
#35117 = AXIS2_PLACEMENT_3D ( 'NONE', #32045, #47066, #1269 ) ;
#35118 = AXIS2_PLACEMENT_3D ( 'NONE', #31799, #46818, #9876 ) ;
#35119 = ORIENTED_EDGE ( 'NONE', *, *, #35910, .F. ) ;
#35120 = CARTESIAN_POINT ( 'NONE',  ( -23.08463366406817840, -10.68898790873936555, 59.83033381731064537 ) ) ;
#35121 = EDGE_CURVE ( 'NONE', #29632, #188, #1314, .T. ) ;
#35122 = CARTESIAN_POINT ( 'NONE',  ( -16.71957921250844592, -21.82421608262117729, 68.71032757591046902 ) ) ;
#35123 = CARTESIAN_POINT ( 'NONE',  ( -48.42409385541304800, -25.10920654474410441, 79.99999999999998579 ) ) ;
#35124 =( BOUNDED_CURVE ( )  B_SPLINE_CURVE ( 3, ( #48168, #37307, #45230, #48408 ),
 .UNSPECIFIED., .F., .F. ) 
 B_SPLINE_CURVE_WITH_KNOTS ( ( 4, 4 ),
 ( 6.081827386389253576, 6.484543227969918888 ),
 .UNSPECIFIED. ) 
 CURVE ( )  GEOMETRIC_REPRESENTATION_ITEM ( )  RATIONAL_B_SPLINE_CURVE ( ( 1.000000000000000000, 0.9865305980755139093, 0.9865305980755139093, 1.000000000000000000 ) ) 
 REPRESENTATION_ITEM ( '' )  );
#35125 = AXIS2_PLACEMENT_3D ( 'NONE', #28236, #43266, #15925 ) ;
#35126 = ORIENTED_EDGE ( 'NONE', *, *, #24414, .T. ) ;
#35127 = CARTESIAN_POINT ( 'NONE',  ( -11.60677555321244547, -18.70493759839273906, 68.44519605431926834 ) ) ;
#35128 = CARTESIAN_POINT ( 'NONE',  ( -22.76532612177806314, -10.19550891705927498, 73.62593845350987465 ) ) ;
#35129 = CARTESIAN_POINT ( 'NONE',  ( -22.11926001268504294, -9.024814352312150234, 63.30658345311071855 ) ) ;
#35130 = CARTESIAN_POINT ( 'NONE',  ( -12.05451961919647630, -9.643808529799599683, 57.20280282899455671 ) ) ;
#35131 = EDGE_LOOP ( 'NONE', ( #32640, #10097, #26040, #5234 ) ) ;
#35132 = CARTESIAN_POINT ( 'NONE',  ( -24.55871722839809834, -12.66422925090921225, 69.88747596251579353 ) ) ;
#35133 = CARTESIAN_POINT ( 'NONE',  ( -24.83179309550701319, -15.60247978309782546, 73.19577886632693264 ) ) ;
#35134 = CARTESIAN_POINT ( 'NONE',  ( -24.31823732957325745, -17.63313362019280106, 66.05861802595141796 ) ) ;
#35135 = ORIENTED_EDGE ( 'NONE', *, *, #40586, .F. ) ;
#35136 = CARTESIAN_POINT ( 'NONE',  ( -22.49805058420730219, -9.986866540729424813, 73.78161091687563555 ) ) ;
#35137 = EDGE_LOOP ( 'NONE', ( #40983, #18446, #11342, #38903 ) ) ;
#35138 = CARTESIAN_POINT ( 'NONE',  ( -19.24190894175819366, -7.584296403803404196, 63.54593838833191910 ) ) ;
#35139 = CARTESIAN_POINT ( 'NONE',  ( -12.74563483257940177, -17.19133189234193893, 49.52966884056655772 ) ) ;
#35140 = ORIENTED_EDGE ( 'NONE', *, *, #6550, .F. ) ;
#35141 = CARTESIAN_POINT ( 'NONE',  ( -16.36834346081282732, -22.18410778960565466, 61.94063409281806543 ) ) ;
#35142 = DIRECTION ( 'NONE',  ( -3.071710424422018668E-17, 6.404604876783312462E-16, 1.000000000000000000 ) ) ;
#35143 = CARTESIAN_POINT ( 'NONE',  ( -24.22177629109872399, -13.13842424187848934, 63.13264177643409880 ) ) ;
#35144 = LINE ( 'NONE', #7675, #47893 ) ;
#35145 = ORIENTED_EDGE ( 'NONE', *, *, #21868, .T. ) ;
#35146 = PRODUCT_DEFINITION_CONTEXT ( 'detailed design', #43887, 'design' ) ;
#35147 = CARTESIAN_POINT ( 'NONE',  ( -20.52762626839951210, -8.534807245883811788, 63.61121513079540080 ) ) ;
#35148 = EDGE_CURVE ( 'NONE', #31941, #45590, #16002, .T. ) ;
#35149 = CARTESIAN_POINT ( 'NONE',  ( -10.42257993575900876, -15.70014684107950842, 68.12200980565171449 ) ) ;
#35150 = ORIENTED_EDGE ( 'NONE', *, *, #22218, .T. ) ;
#35151 = CARTESIAN_POINT ( 'NONE',  ( -12.83007281553047108, -20.09077549419061626, 71.80653676829817300 ) ) ;
#35152 = AXIS2_PLACEMENT_3D ( 'NONE', #36252, #13108, #13593 ) ;
#35153 = B_SPLINE_CURVE_WITH_KNOTS ( 'NONE', 3,
 ( #7210, #33264, #14537, #41168, #18755, #10648, #44886, #3490, #21970, #45128 ),
 .UNSPECIFIED., .F., .F.,
 ( 4, 2, 2, 2, 4 ),
 ( 0.000000000000000000, 0.2500000000000000000, 0.5000000000000000000, 0.7500000000000000000, 1.000000000000000000 ),
 .UNSPECIFIED. ) ;
#35154 = CARTESIAN_POINT ( 'NONE',  ( -21.78783678618839303, -8.770877803870156697, 70.38778484029896276 ) ) ;
#35155 = ADVANCED_FACE ( 'NONE', ( #23176 ), #46062, .T. ) ;
#35156 = ORIENTED_EDGE ( 'NONE', *, *, #14927, .T. ) ;
#35157 = EDGE_LOOP ( 'NONE', ( #3518, #18207, #290, #17154, #10766 ) ) ;
#35158 = CARTESIAN_POINT ( 'NONE',  ( -14.87246701381353198, -21.32764640494525210, 58.39291311840838006 ) ) ;
#35159 = CARTESIAN_POINT ( 'NONE',  ( -20.04168780904239355, -21.30143565362524072, 72.41981212996954298 ) ) ;
#35160 = DIRECTION ( 'NONE',  ( 3.549360974551883545E-17, -6.371834667872732552E-18, -1.000000000000000000 ) ) ;
#35161 = AXIS2_PLACEMENT_3D ( 'NONE', #48641, #41757, #22304 ) ;
#35162 = CARTESIAN_POINT ( 'NONE',  ( -18.19284385650551883, -7.406986770994973490, 48.81910596585309747 ) ) ;
#35163 = CARTESIAN_POINT ( 'NONE',  ( -12.39467452642779044, -9.940348555453047297, 57.10438015346839791 ) ) ;
#35164 = LINE ( 'NONE', #20649, #44044 ) ;
#35165 = CARTESIAN_POINT ( 'NONE',  ( -17.28496127917699710, -14.43418371046636217, 56.49999999999994316 ) ) ;
#35166 = CYLINDRICAL_SURFACE ( 'NONE', #19023, 1.250000000000001110 ) ;
#35167 = VERTEX_POINT ( 'NONE', #38168 ) ;
#35168 = EDGE_LOOP ( 'NONE', ( #3062, #33135, #16208, #36568, #45241 ) ) ;
#35169 = CARTESIAN_POINT ( 'NONE',  ( -11.52915434062558120, -10.92788463621912420, 60.82318916367986361 ) ) ;
#35170 = DIRECTION ( 'NONE',  ( 0.000000000000000000, 0.000000000000000000, 1.000000000000000000 ) ) ;
#35171 = EDGE_CURVE ( 'NONE', #43290, #39133, #20797, .T. ) ;
#35172 = CARTESIAN_POINT ( 'NONE',  ( -12.60227155074094441, -19.95281705956671559, 68.35129494334645983 ) ) ;
#35173 = CARTESIAN_POINT ( 'NONE',  ( -18.30726797983150789, -21.75326897020822514, 68.81514702557041119 ) ) ;
#35174 = EDGE_CURVE ( 'NONE', #14220, #17691, #10128, .T. ) ;
#35175 =( BOUNDED_CURVE ( )  B_SPLINE_CURVE ( 3, ( #15353, #14855, #38014, #33573 ),
 .UNSPECIFIED., .F., .F. ) 
 B_SPLINE_CURVE_WITH_KNOTS ( ( 4, 4 ),
 ( 0.5000000000000000000, 0.9074455897393662873 ),
 .UNSPECIFIED. ) 
 CURVE ( )  GEOMETRIC_REPRESENTATION_ITEM ( )  RATIONAL_B_SPLINE_CURVE ( ( 1.000000000000000666, 0.4567392136813310799, 0.3561768502900293232, 0.6983129098260962841 ) ) 
 REPRESENTATION_ITEM ( '' )  );
#35176 = VERTEX_POINT ( 'NONE', #30816 ) ;
#35177 = CARTESIAN_POINT ( 'NONE',  ( -14.99952990268716491, -21.37596734354964667, 61.92135132145442356 ) ) ;
#35178 = CARTESIAN_POINT ( 'NONE',  ( -23.75068382698706770, -10.87373689121910658, 73.47537926597675551 ) ) ;
#35179 = CARTESIAN_POINT ( 'NONE',  ( -17.39742496553465401, -7.759256980052345654, 67.02039592192090822 ) ) ;
#35180 = CARTESIAN_POINT ( 'NONE',  ( -24.20601044598569374, -16.76383555912477874, 73.03903240339252534 ) ) ;
#35181 = EDGE_CURVE ( 'NONE', #1692, #48324, #7890, .T. ) ;
#35182 = ORIENTED_EDGE ( 'NONE', *, *, #31418, .T. ) ;
#35183 =( BOUNDED_SURFACE ( )  B_SPLINE_SURFACE ( 3, 1, ( 
 ( #3388, #33649 ),
 ( #3897, #22119 ),
 ( #18906, #29994 ),
 ( #37593, #10546 ),
 ( #40568, #26055 ),
 ( #29494, #36617 ),
 ( #40817, #17904 ) ),
 .UNSPECIFIED., .T., .F., .F. ) 
 B_SPLINE_SURFACE_WITH_KNOTS ( ( 4, 3, 4 ),
 ( 2, 2 ),
 ( 0.000000000000000000, 0.5000000000000000000, 1.000000000000000000 ),
 ( 0.000000000000000000, 1.000000000000000000 ),
 .UNSPECIFIED. ) 
 GEOMETRIC_REPRESENTATION_ITEM ( )  RATIONAL_B_SPLINE_SURFACE ( (
 ( 1.000000000000000000, 1.000000000000000000),
 ( 0.3333333333333335369, 0.3333333333333330373),
 ( 0.3333333333333335369, 0.3333333333333330373),
 ( 1.000000000000000000, 1.000000000000000000),
 ( 0.3333333333333333703, 0.3333333333333333703),
 ( 0.3333333333333333703, 0.3333333333333333703),
 ( 1.000000000000000000, 1.000000000000000000) ) ) 
 REPRESENTATION_ITEM ( '' )  SURFACE ( )  );
#35184 = CARTESIAN_POINT ( 'NONE',  ( -20.13271805750754950, -8.299978134201072777, 70.53628287813307907 ) ) ;
#35185 = VECTOR ( 'NONE', #41854, 1000.000000000000114 ) ;
#35186 = CARTESIAN_POINT ( 'NONE',  ( -24.37817933763783529, -15.98629254845087466, 69.94796348494512017 ) ) ;
#35187 = PRODUCT_DEFINITION ( 'UNKNOWN', '', #21171, #39578 ) ;
#35188 = EDGE_LOOP ( 'NONE', ( #2147, #40449, #32281, #33819, #20212 ) ) ;
#35189 = VECTOR ( 'NONE', #45393, 1000.000000000000000 ) ;
#35190 = DIRECTION ( 'NONE',  ( -0.1261685609230672744, -0.9920088176193796459, -5.058037263227848996E-08 ) ) ;
#35191 = CARTESIAN_POINT ( 'NONE',  ( -24.21863471429747250, -16.49938873345172397, 59.31259601734559794 ) ) ;
#35192 = ORIENTED_EDGE ( 'NONE', *, *, #5333, .T. ) ;
#35193 = CARTESIAN_POINT ( 'NONE',  ( -14.09463846823036981, -8.088735815341543400, 53.49999999999994316 ) ) ;
#35194 = CIRCLE ( 'NONE', #42318, 0.09999999999999939493 ) ;
#35195 = EDGE_LOOP ( 'NONE', ( #37451, #11506, #45236, #2524, #41068 ) ) ;
#35196 = DIRECTION ( 'NONE',  ( -0.9687793358424819923, 0.2479245821708680464, 0.000000000000000000 ) ) ;
#35197 = CARTESIAN_POINT ( 'NONE',  ( -18.84068548446033731, -21.72355622379298978, 72.44077832767429470 ) ) ;
#35198 = EDGE_LOOP ( 'NONE', ( #19630, #27447, #13634, #15367 ) ) ;
#35199 = CARTESIAN_POINT ( 'NONE',  ( -15.18349748943555966, -8.120920323119461770, 56.94179993390997652 ) ) ;
#35200 = CARTESIAN_POINT ( 'NONE',  ( -18.33016535318852291, -22.20398178282153623, 69.07160637178317586 ) ) ;
#35201 = CARTESIAN_POINT ( 'NONE',  ( -18.84284385650551741, -8.811426318492348031, 52.18089403414751359 ) ) ;
#35202 = VERTEX_POINT ( 'NONE', #7927 ) ;
#35203 = DIRECTION ( 'NONE',  ( 0.000000000000000000, 1.000000000000000000, -0.000000000000000000 ) ) ;
#35204 = EDGE_CURVE ( 'NONE', #35946, #15919, #22947, .T. ) ;
#35205 = CARTESIAN_POINT ( 'NONE',  ( -10.61954745215241935, -11.77581898585687092, 74.75114390221474991 ) ) ;
#35206 = CARTESIAN_POINT ( 'NONE',  ( -14.84927081153347039, -21.37251255130113137, 61.65072491673618771 ) ) ;
#35207 = ORIENTED_EDGE ( 'NONE', *, *, #6395, .T. ) ;
#35208 = CARTESIAN_POINT ( 'NONE',  ( -16.22920462672756159, -7.911818831816758824, 60.50028431019059383 ) ) ;
#35209 = CARTESIAN_POINT ( 'NONE',  ( -11.81042834955647258, -10.54382735031610174, 74.45357240259568243 ) ) ;
#35210 = CARTESIAN_POINT ( 'NONE',  ( -17.42409385541299471, -14.80920654474434883, 62.02966884056656482 ) ) ;
#35211 = CARTESIAN_POINT ( 'NONE',  ( -20.51563283865871057, -8.030886342657675314, 66.88765784730034625 ) ) ;
#35212 = CARTESIAN_POINT ( 'NONE',  ( -12.65513433691805290, -20.00553804586020590, 64.75186297256590251 ) ) ;
#35213 = ORIENTED_EDGE ( 'NONE', *, *, #35717, .T. ) ;
#35214 = VERTEX_POINT ( 'NONE', #37936 ) ;
#35215 = CARTESIAN_POINT ( 'NONE',  ( -18.32882331211134286, -7.814473174497912566, 73.72575526123169709 ) ) ;
#35216 = CARTESIAN_POINT ( 'NONE',  ( -11.00421863625541974, -17.72293202094342490, 71.86158434966563391 ) ) ;
#35217 = ORIENTED_EDGE ( 'NONE', *, *, #17731, .T. ) ;
#35218 = CARTESIAN_POINT ( 'NONE',  ( -15.82259747647940173, -7.533288219471245384, 67.25511999279136433 ) ) ;
#35219 = FACE_OUTER_BOUND ( 'NONE', #6392, .T. ) ;
#35220 = CARTESIAN_POINT ( 'NONE',  ( -21.54284385759798681, -7.587656875400192291, 49.25157356644813689 ) ) ;
#35221 = CARTESIAN_POINT ( 'NONE',  ( -23.82760511577973617, -11.00139541567114421, 73.48476430283872673 ) ) ;
#35222 = CARTESIAN_POINT ( 'NONE',  ( -10.84896266223257122, -17.37486770053218521, 71.71150890757306229 ) ) ;
#35223 = DIRECTION ( 'NONE',  ( 0.9687793358424821033, -0.2479245821708677133, 0.000000000000000000 ) ) ;
#35224 = VECTOR ( 'NONE', #2447, 1000.000000000000000 ) ;
#35225 = EDGE_LOOP ( 'NONE', ( #22461, #46520 ) ) ;
#35226 = DIRECTION ( 'NONE',  ( 0.8949343913984055821, -0.4461977533475101620, -3.119193279067933041E-16 ) ) ;
#35227 = ADVANCED_FACE ( 'NONE', ( #27101, #42127 ), #24390, .T. ) ;
#35228 = CARTESIAN_POINT ( 'NONE',  ( -10.45582064790140464, -15.88054293009791706, 64.80211778324330396 ) ) ;
#35229 = CARTESIAN_POINT ( 'NONE',  ( -19.83745867003831975, -21.38006599400703678, 68.94187494913028047 ) ) ;
#35230 = DIRECTION ( 'NONE',  ( -0.6323592902076722311, -0.7746752403995150749, 4.984538757074984646E-08 ) ) ;
#35231 = EDGE_CURVE ( 'NONE', #21060, #23374, #34965, .T. ) ;
#35232 = CIRCLE ( 'NONE', #45376, 4.686500000000000554 ) ;
#35233 = EDGE_LOOP ( 'NONE', ( #39447, #37182, #7849, #12837 ) ) ;
#35234 = VERTEX_POINT ( 'NONE', #35451 ) ;
#35235 = EDGE_CURVE ( 'NONE', #3060, #46704, #45377, .T. ) ;
#35236 = ORIENTED_EDGE ( 'NONE', *, *, #20956, .F. ) ;
#35237 = CARTESIAN_POINT ( 'NONE',  ( -24.47697530877170990, -14.85041752174647733, 63.12785080464042409 ) ) ;
#35238 = CARTESIAN_POINT ( 'NONE',  ( -24.11793993921729395, -12.76166543249827434, 70.07243002473258286 ) ) ;
#35239 = EDGE_CURVE ( 'NONE', #16707, #18836, #43091, .T. ) ;
#35240 = EDGE_LOOP ( 'NONE', ( #47389, #19967, #34825, #30323 ) ) ;
#35241 = CARTESIAN_POINT ( 'NONE',  ( -10.82867520472564848, -11.34449427682889677, 67.73369198428547122 ) ) ;
#35242 = CARTESIAN_POINT ( 'NONE',  ( -11.13733870171179596, -11.61806121328041996, 67.90392505421056057 ) ) ;
#35243 = VERTEX_POINT ( 'NONE', #46563 ) ;
#35244 = CARTESIAN_POINT ( 'NONE',  ( -20.95139844211411884, -8.247003834134126521, 59.96408367069768275 ) ) ;
#35245 = CARTESIAN_POINT ( 'NONE',  ( -10.47144901298989694, -13.99582629904338127, 57.73359634450734745 ) ) ;
#35246 = AXIS2_PLACEMENT_3D ( 'NONE', #837, #46133, #26447 ) ;
#35247 = ORIENTED_EDGE ( 'NONE', *, *, #46154, .F. ) ;
#35248 = CARTESIAN_POINT ( 'NONE',  ( -19.86401518824997225, -21.42384811948916834, 69.22010401872219632 ) ) ;
#35249 = CARTESIAN_POINT ( 'NONE',  ( -10.13336409668949400, -13.27690444941326042, 74.77843402251788518 ) ) ;
#35250 = AXIS2_PLACEMENT_3D ( 'NONE', #7813, #18871, #413 ) ;
#35251 = VECTOR ( 'NONE', #27764, 1000.000000000000227 ) ;
#35252 = EDGE_CURVE ( 'NONE', #34423, #25804, #27857, .T. ) ;
#35253 = EDGE_LOOP ( 'NONE', ( #7987, #40459, #48125, #40785 ) ) ;
#35254 = CARTESIAN_POINT ( 'NONE',  ( -24.47243858273885664, -15.17772250287404567, 59.38732937676161328 ) ) ;
#35255 = CARTESIAN_POINT ( 'NONE',  ( -24.14679772577363437, -12.68507108172156705, 70.05770892828130059 ) ) ;
#35256 = PLANE ( 'NONE',  #41516 ) ;
#35257 = VERTEX_POINT ( 'NONE', #13036 ) ;
#35258 = PLANE ( 'NONE',  #11309 ) ;
#35259 = DIRECTION ( 'NONE',  ( 6.695352868347749370E-17, -2.732354947069688554E-32, -1.000000000000000000 ) ) ;
#35260 = CARTESIAN_POINT ( 'NONE',  ( -24.08907074505709645, -11.48026357735065872, 63.13713704106291402 ) ) ;
#35261 = AXIS2_PLACEMENT_3D ( 'NONE', #38326, #12012, #8318 ) ;
#35262 = EDGE_CURVE ( 'NONE', #2300, #20349, #1966, .T. ) ;
#35263 = CARTESIAN_POINT ( 'NONE',  ( -13.69528579949288982, -8.884502191640171631, 56.98584450146461222 ) ) ;
#35264 = CARTESIAN_POINT ( 'NONE',  ( -22.79960237261627398, -9.650942640399760464, 73.66656521964461035 ) ) ;
#35265 = CARTESIAN_POINT ( 'NONE',  ( -19.15893590421327985, -8.027528287274607877, 60.03381006258986474 ) ) ;
#35266 = ORIENTED_EDGE ( 'NONE', *, *, #2116, .F. ) ;
#35267 = DIRECTION ( 'NONE',  ( 1.000000000000000000, 2.866981220435666553E-17, 0.000000000000000000 ) ) ;
#35268 = CARTESIAN_POINT ( 'NONE',  ( -22.79734292848665334, -10.24514101169484448, 66.84182257473258915 ) ) ;
#35269 = CARTESIAN_POINT ( 'NONE',  ( -24.86682742714664229, -14.47648176530652719, 66.34439218741853495 ) ) ;
#35270 = CYLINDRICAL_SURFACE ( 'NONE', #48589, 0.1500000000000047407 ) ;
#35271 = CARTESIAN_POINT ( 'NONE',  ( -24.86610167639389246, -14.46236660854407674, 66.29797298380238146 ) ) ;
#35272 = CARTESIAN_POINT ( 'NONE',  ( -16.22409385650551883, -6.426201560718813433, 50.50509628382439331 ) ) ;
#35273 = ORIENTED_EDGE ( 'NONE', *, *, #21809, .T. ) ;
#35274 = CARTESIAN_POINT ( 'NONE',  ( -15.40811923343077083, -21.56513327689926030, 72.06047564147742435 ) ) ;
#35275 = DIRECTION ( 'NONE',  ( 0.9687793358424819923, -0.2479245821708680464, 0.000000000000000000 ) ) ;
#35276 = ORIENTED_EDGE ( 'NONE', *, *, #30783, .F. ) ;
#35277 = DIRECTION ( 'NONE',  ( -3.071710424422018668E-17, 6.404604876783312462E-16, 1.000000000000000000 ) ) ;
#35278 = CARTESIAN_POINT ( 'NONE',  ( -35.32409385541306079, -6.359206544744109735, 52.29999999999998295 ) ) ;
#35279 = CARTESIAN_POINT ( 'NONE',  ( -17.96161316005734676, -22.23979900576015822, 62.07524705671683307 ) ) ;
#35280 = CARTESIAN_POINT ( 'NONE',  ( -23.26642198590026211, -10.18619985444824572, 63.23332526816662380 ) ) ;
#35281 = CARTESIAN_POINT ( 'NONE',  ( -16.26195973558533581, -21.76306465430365122, 58.57113428431811997 ) ) ;
#35282 = VERTEX_POINT ( 'NONE', #39148 ) ;
#35283 = ADVANCED_FACE ( 'NONE', ( #31279 ), #46312, .T. ) ;
#35284 = CARTESIAN_POINT ( 'NONE',  ( -41.67850562011894766, -14.80920654474422271, 68.96470588235293064 ) ) ;
#35285 = CARTESIAN_POINT ( 'NONE',  ( -10.85164377074246289, -17.36018552090334310, 64.92179613810992578 ) ) ;
#35286 = CARTESIAN_POINT ( 'NONE',  ( -12.13668540368383653, -10.14142895936130628, 60.44429485117178302 ) ) ;
#35287 = EDGE_LOOP ( 'NONE', ( #22952, #26334 ) ) ;
#35288 = CIRCLE ( 'NONE', #22730, 2.000000000000001332 ) ;
#35289 = B_SPLINE_CURVE_WITH_KNOTS ( 'NONE', 3,
 ( #46795, #31050, #8893, #19469, #770, #28069, #13039, #27593, #1484, #42132 ),
 .UNSPECIFIED., .F., .F.,
 ( 4, 2, 2, 2, 4 ),
 ( 0.1272669073657891059, 0.2522669073462849854, 0.3772669073267808093, 0.5022669073072767443, 0.6272669072877725682 ),
 .UNSPECIFIED. ) ;
#35290 = CARTESIAN_POINT ( 'NONE',  ( -18.29367245688808552, -17.15309925898211318, 77.49999999999994316 ) ) ;
#35291 = AXIS2_PLACEMENT_3D ( 'NONE', #19253, #45363, #19011 ) ;
#35292 = FACE_OUTER_BOUND ( 'NONE', #3041, .T. ) ;
#35293 = CARTESIAN_POINT ( 'NONE',  ( -13.80550519567689172, -20.80142258237229669, 65.00131257522635053 ) ) ;
#35294 = CARTESIAN_POINT ( 'NONE',  ( -20.99070387547166661, -20.89051904145194527, 65.58453967743210455 ) ) ;
#35295 = CIRCLE ( 'NONE', #21930, 5.249999999999998224 ) ;
#35296 = AXIS2_PLACEMENT_3D ( 'NONE', #38226, #30876, #34539 ) ;
#35297 = ORIENTED_EDGE ( 'NONE', *, *, #47404, .T. ) ;
#35298 = ORIENTED_EDGE ( 'NONE', *, *, #32095, .F. ) ;
#35299 = CARTESIAN_POINT ( 'NONE',  ( -19.93659385541304019, -8.995762431863214559, 51.38120296130585274 ) ) ;
#35300 = EDGE_CURVE ( 'NONE', #38102, #21018, #4303, .T. ) ;
#35301 = CARTESIAN_POINT ( 'NONE',  ( -18.68070144837527735, -7.415226739706412218, 47.99999999999994316 ) ) ;
#35302 = ADVANCED_FACE ( 'NONE', ( #13270 ), #12568, .T. ) ;
#35303 = DIRECTION ( 'NONE',  ( 6.385196549736874992E-06, -5.147825522337142951E-06, 0.9999999999663644612 ) ) ;
#35304 = VECTOR ( 'NONE', #39575, 1000.000000000000000 ) ;
#35305 = CARTESIAN_POINT ( 'NONE',  ( -22.97880759471717838, -10.54929209374549082, 59.60203382397228467 ) ) ;
#35306 = LINE ( 'NONE', #28657, #1043 ) ;
#35307 = FACE_OUTER_BOUND ( 'NONE', #44887, .T. ) ;
#35308 = CARTESIAN_POINT ( 'NONE',  ( -18.45262242793555885, -21.79183460504582470, 65.50099240037707204 ) ) ;
#35309 =( BOUNDED_SURFACE ( )  B_SPLINE_SURFACE ( 1, 2, ( 
 ( #26889, #45612, #46575, #27112, #27356, #27601, #34493, #8658, #1019, #16014, #19975, #19478, #11863, #23921, #41899, #7940, #38922, #23684, #38682, #5201, #20208, #35220, #8177, #23190, #38180, #37948, #4234, #19243, #34245, #4462, #4965, #779, #15775, #30831, #45844, #12100, #42141, #8406, #40142, #24156, #9634, #10100, #1979, #24877, #47295, #6162, #28079, #32736, #25123, #13766, #16976, #16740, #32275, #21436, #6407, #2218, #24650, #13530, #28576, #24402, #28810, #43103, #39650, #43847, #20704, #27840, #43604, #32505, #13047, #9862, #5921, #2467, #17230, #5449, #39413, #5695, #42869, #20466, #9140, #21188, #12818, #1748, #36420, #36182, #35462, #39891, #2700, #17707, #39161, #31782, #46802, #35694, #9382, #20942, #32022, #47040, #13283, #28337, #17476, #47531, #43363, #35942, #33202, #44817, #7390, #44330, #25363, #13996, #33441, #44560, #2933, #29293, #29050, #40376, #37383, #25591, #29785, #3675, #36902, #18680, #3427, #48237, #37140, #14474, #10582, #11071, #18940, #48480, #25837, #26329, #17943, #26093, #40601, #41105, #22390, #29532, #6885, #40857, #10816, #30042, #6644, #44097, #21661, #7139, #18432, #10350, #14244, #3184, #21899, #22156, #18194, #33686, #14712, #36082, #14977, #47760, #45068, #36651, #11315, #41342, #7635, #22640, #37638, #32961, #3933, #48007, #30529, #5143, #23136, #15958, #38362, #46261, #27058, #962, #45305, #12518, #12042, #4906, #8847 ),
 ( #480, #19918, #19678, #33953, #38127, #15465, #4655, #247, #30772, #7879, #8595, #37894, #45793, #15225, #42082, #27543, #720, #15715, #22900, #30284, #42585, #34684, #11552, #19184, #23863, #26576, #41597, #23625, #38867, #45547, #4182, #31000, #34189, #38622, #8351, #23368, #11806, #26828, #4403, #34923, #41847, #8121, #19422, #34428, #46022, #12277, #42327, #27301, #1188, #16194, #31238, #42810, #24594, #36125, #44450, #16445, #21127, #5386, #28018, #40734, #46977, #24341, #10703, #9574, #35408, #24096, #25719, #20405, #47228, #2408, #1685, #43045, #16924, #20647, #17418, #31960, #35877, #16685, #39589, #20151, #13221, #12990, #31726, #35641, #1431, #35162, #1923, #28271, #9084, #39102, #39831, #43300, #29418, #6099, #2159, #46747, #9322, #31479, #5866, #20883, #32450, #39352, #17159, #32212, #13473, #28520, #5639, #43544, #9808, #24820, #46514, #47475, #14364, #12767, #27781, #26703, #41722, #29661, #40989, #44695, #19307, #15593, #37027, #34310, #18561, #3807, #33568, #18314, #7762, #18823, #10952, #25970, #33829, #597, #33325, #126, #4298, #44947, #19065, #41470, #365, #22274, #26949, #30657, #8012, #11202, #7272, #26455, #45676, #11932, #45189, #15110, #22778, #37771, #48613, #23025, #37265, #30168, #38010, #14850, #22033, #4067, #7015, #3555, #34074, #11428, #45425, #15348, #48364, #3314, #30410, #14599, #29914, #26214, #11678, #41226, #7512, #22518, #37512 ) ),
 .UNSPECIFIED., .F., .F., .F. ) 
 B_SPLINE_SURFACE_WITH_KNOTS ( ( 2, 2 ),
 ( 3, 2, 2, 2, 2, 2, 2, 2, 2, 2, 2, 2, 2, 2, 2, 2, 2, 2, 2, 2, 2, 2, 2, 2, 2, 2, 2, 2, 2, 2, 2, 2, 2, 2, 2, 2, 2, 2, 2, 2, 2, 2, 2, 2, 2, 2, 2, 2, 2, 2, 2, 2, 2, 2, 2, 2, 2, 2, 2, 2, 2, 2, 2, 2, 2, 2, 2, 2, 2, 2, 2, 2, 2, 2, 2, 2, 2, 2, 2, 2, 2, 2, 2, 2, 2, 2, 2, 2, 2, 3 ),
 ( 0.000000000000000000, 1.000000000000000000 ),
 ( 0.000000000000000000, 0.01041666666666666609, 0.02083333333333333218, 0.03125000000000000000, 0.04166666666666666435, 0.05208333333333333565, 0.06250000000000000000, 0.07291666666666667129, 0.08333333333333332871, 0.09375000000000000000, 0.1041666666666666713, 0.1145833333333333287, 0.1250000000000000000, 0.1354166666666666574, 0.1458333333333333426, 0.1562500000000000000, 0.1666666666666666574, 0.1770833333333333426, 0.1875000000000000000, 0.1979166666666666574, 0.2083333333333333426, 0.2187500000000000000, 0.2291666666666666574, 0.2395833333333333426, 0.2500000000000000000, 0.2604166666666666852, 0.2708333333333333148, 0.2812500000000000000, 0.2916666666666666852, 0.3020833333333333148, 0.3125000000000000000, 0.3229166666666666852, 0.3333333333333333148, 0.3437500000000000000, 0.3541666666666666852, 0.3645833333333333148, 0.3750000000000000000, 0.3854166666666666852, 0.3958333333333333148, 0.4062500000000000000, 0.4166666666666666852, 0.4270833333333333148, 0.4375000000000000000, 0.4479166666666666852, 0.4583333333333333148, 0.4687500000000000000, 0.4791666666666666852, 0.4895833333333333148, 0.5000000000000000000, 0.5104166666666666297, 0.5208333333333333703, 0.5312500000000000000, 0.5416666666666666297, 0.5520833333333333703, 0.5625000000000000000, 0.5729166666666666297, 0.5833333333333333703, 0.5937500000000000000, 0.6041666666666666297, 0.6145833333333333703, 0.6250000000000000000, 0.6354166666666666297, 0.6458333333333333703, 0.6562500000000000000, 0.6666666666666666297, 0.6770833333333333703, 0.6875000000000000000, 0.6979166666666666297, 0.7083333333333333703, 0.7187500000000000000, 0.7291666666666666297, 0.7395833333333333703, 0.7500000000000000000, 0.7604166666666666297, 0.7708333333333333703, 0.7812500000000000000, 0.7916666666666666297, 0.8020833333333333703, 0.8125000000000000000, 0.8229166666666666297, 0.8333333333333333703, 0.8437500000000000000, 0.8541666666666666297, 0.8645833333333333703, 0.8750000000000000000, 0.8854166666666666297, 0.8958333333333333703, 0.9062500000000000000, 0.9166666666666666297, 0.9259047100830449795 ),
 .UNSPECIFIED. ) 
 GEOMETRIC_REPRESENTATION_ITEM ( )  RATIONAL_B_SPLINE_SURFACE ( (
 ( 1.000000000000000000, 0.9238795325112867385, 1.000000000000000000, 0.9238795325112867385, 1.000000000000000000, 0.9238795325112867385, 1.000000000000000000, 0.9238795325112867385, 1.000000000000000000, 0.9238795325112867385, 1.000000000000000000, 0.9238795325112867385, 1.000000000000000000, 0.9238795325112867385, 1.000000000000000000, 0.9238795325112867385, 1.000000000000000000, 0.9238795325112867385, 1.000000000000000000, 0.9238795325112867385, 1.000000000000000000, 0.9238795325112867385, 1.000000000000000000, 0.9238795325112867385, 1.000000000000000000, 0.9238795325112867385, 1.000000000000000000, 0.9238795325112867385, 1.000000000000000000, 0.9238795325112867385, 1.000000000000000000, 0.9238795325112867385, 1.000000000000000000, 0.9238795325112867385, 1.000000000000000000, 0.9238795325112867385, 1.000000000000000000, 0.9238795325112867385, 1.000000000000000000, 0.9238795325112867385, 1.000000000000000000, 0.9238795325112867385, 1.000000000000000000, 0.9238795325112867385, 1.000000000000000000, 0.9238795325112867385, 1.000000000000000000, 0.9238795325112867385, 1.000000000000000000, 0.9238795325112867385, 1.000000000000000000, 0.9238795325112867385, 1.000000000000000000, 0.9238795325112867385, 1.000000000000000000, 0.9238795325112867385, 1.000000000000000000, 0.9238795325112867385, 1.000000000000000000, 0.9238795325112867385, 1.000000000000000000, 0.9238795325112867385, 1.000000000000000000, 0.9238795325112867385, 1.000000000000000000, 0.9238795325112867385, 1.000000000000000000, 0.9238795325112867385, 1.000000000000000000, 0.9238795325112867385, 1.000000000000000000, 0.9238795325112867385, 1.000000000000000000, 0.9238795325112867385, 1.000000000000000000, 0.9238795325112867385, 1.000000000000000000, 0.9238795325112867385, 1.000000000000000000, 0.9238795325112867385, 1.000000000000000000, 0.9238795325112867385, 1.000000000000000000, 0.9238795325112867385, 1.000000000000000000, 0.9238795325112867385, 1.000000000000000000, 0.9238795325112867385, 1.000000000000000000, 0.9238795325112867385, 1.000000000000000000, 0.9238795325112867385, 1.000000000000000000, 0.9238795325112867385, 1.000000000000000000, 0.9238795325112867385, 1.000000000000000000, 0.9238795325112867385, 1.000000000000000000, 0.9238795325112867385, 1.000000000000000000, 0.9238795325112867385, 1.000000000000000000, 0.9238795325112867385, 1.000000000000000000, 0.9238795325112867385, 1.000000000000000000, 0.9238795325112867385, 1.000000000000000000, 0.9238795325112867385, 1.000000000000000000, 0.9238795325112867385, 1.000000000000000000, 0.9238795325112867385, 1.000000000000000000, 0.9238795325112867385, 1.000000000000000000, 0.9238795325112867385, 1.000000000000000000, 0.9238795325112867385, 1.000000000000000000, 0.9238795325112867385, 1.000000000000000000, 0.9238795325112867385, 1.000000000000000000, 0.9238795325112867385, 1.000000000000000000, 0.9238795325112867385, 1.000000000000000000, 0.9238795325112867385, 1.000000000000000000, 0.9238795325112867385, 1.000000000000000000, 0.9238795325112867385, 1.000000000000000000, 0.9238795325112867385, 1.000000000000000000, 0.9238795325112867385, 1.000000000000000000, 0.9238795325112867385, 1.000000000000000000, 0.9238795325112867385, 1.000000000000000000, 0.9238795325112867385, 1.000000000000000000, 0.9238795325112867385, 1.000000000000000000, 0.9238795325112867385, 1.000000000000000000, 0.9238795325112867385, 1.000000000000000000, 0.9238795325112867385, 1.000000000000000000, 0.9238795325112867385, 1.000000000000000000, 0.9238795325112867385, 1.000000000000000000, 0.9238795325112867385, 1.000000000000000000, 0.9238795325112867385, 1.000000000000000000, 0.9238795325112867385, 1.000000000000000000, 0.9238795325112867385, 1.000000000000000000, 0.9238795325112867385, 1.000000000000000000, 0.9238795325112867385, 1.000000000000000000, 0.9238795325112867385, 1.000000000000000000, 0.9238795325112867385, 1.000000000000000000, 0.9238795325112867385, 1.000000000000000000, 0.9238795325112867385, 1.000000000000000000, 0.9324923983805685213, 0.9847233224627454096),
 ( 1.000000000000000000, 0.9238795325112867385, 1.000000000000000000, 0.9238795325112867385, 1.000000000000000000, 0.9238795325112867385, 1.000000000000000000, 0.9238795325112867385, 1.000000000000000000, 0.9238795325112867385, 1.000000000000000000, 0.9238795325112867385, 1.000000000000000000, 0.9238795325112867385, 1.000000000000000000, 0.9238795325112867385, 1.000000000000000000, 0.9238795325112867385, 1.000000000000000000, 0.9238795325112867385, 1.000000000000000000, 0.9238795325112867385, 1.000000000000000000, 0.9238795325112867385, 1.000000000000000000, 0.9238795325112867385, 1.000000000000000000, 0.9238795325112867385, 1.000000000000000000, 0.9238795325112867385, 1.000000000000000000, 0.9238795325112867385, 1.000000000000000000, 0.9238795325112867385, 1.000000000000000000, 0.9238795325112867385, 1.000000000000000000, 0.9238795325112867385, 1.000000000000000000, 0.9238795325112867385, 1.000000000000000000, 0.9238795325112867385, 1.000000000000000000, 0.9238795325112867385, 1.000000000000000000, 0.9238795325112867385, 1.000000000000000000, 0.9238795325112867385, 1.000000000000000000, 0.9238795325112867385, 1.000000000000000000, 0.9238795325112867385, 1.000000000000000000, 0.9238795325112867385, 1.000000000000000000, 0.9238795325112867385, 1.000000000000000000, 0.9238795325112867385, 1.000000000000000000, 0.9238795325112867385, 1.000000000000000000, 0.9238795325112867385, 1.000000000000000000, 0.9238795325112867385, 1.000000000000000000, 0.9238795325112867385, 1.000000000000000000, 0.9238795325112867385, 1.000000000000000000, 0.9238795325112867385, 1.000000000000000000, 0.9238795325112867385, 1.000000000000000000, 0.9238795325112867385, 1.000000000000000000, 0.9238795325112867385, 1.000000000000000000, 0.9238795325112867385, 1.000000000000000000, 0.9238795325112867385, 1.000000000000000000, 0.9238795325112867385, 1.000000000000000000, 0.9238795325112867385, 1.000000000000000000, 0.9238795325112867385, 1.000000000000000000, 0.9238795325112867385, 1.000000000000000000, 0.9238795325112867385, 1.000000000000000000, 0.9238795325112867385, 1.000000000000000000, 0.9238795325112867385, 1.000000000000000000, 0.9238795325112867385, 1.000000000000000000, 0.9238795325112867385, 1.000000000000000000, 0.9238795325112867385, 1.000000000000000000, 0.9238795325112867385, 1.000000000000000000, 0.9238795325112867385, 1.000000000000000000, 0.9238795325112867385, 1.000000000000000000, 0.9238795325112867385, 1.000000000000000000, 0.9238795325112867385, 1.000000000000000000, 0.9238795325112867385, 1.000000000000000000, 0.9238795325112867385, 1.000000000000000000, 0.9238795325112867385, 1.000000000000000000, 0.9238795325112867385, 1.000000000000000000, 0.9238795325112867385, 1.000000000000000000, 0.9238795325112867385, 1.000000000000000000, 0.9238795325112867385, 1.000000000000000000, 0.9238795325112867385, 1.000000000000000000, 0.9238795325112867385, 1.000000000000000000, 0.9238795325112867385, 1.000000000000000000, 0.9238795325112867385, 1.000000000000000000, 0.9238795325112867385, 1.000000000000000000, 0.9238795325112867385, 1.000000000000000000, 0.9238795325112867385, 1.000000000000000000, 0.9238795325112867385, 1.000000000000000000, 0.9238795325112867385, 1.000000000000000000, 0.9238795325112867385, 1.000000000000000000, 0.9238795325112867385, 1.000000000000000000, 0.9238795325112867385, 1.000000000000000000, 0.9238795325112867385, 1.000000000000000000, 0.9238795325112867385, 1.000000000000000000, 0.9238795325112867385, 1.000000000000000000, 0.9238795325112867385, 1.000000000000000000, 0.9238795325112867385, 1.000000000000000000, 0.9238795325112867385, 1.000000000000000000, 0.9238795325112867385, 1.000000000000000000, 0.9238795325112867385, 1.000000000000000000, 0.9238795325112867385, 1.000000000000000000, 0.9238795325112867385, 1.000000000000000000, 0.9238795325112867385, 1.000000000000000000, 0.9238795325112867385, 1.000000000000000000, 0.9238795325112867385, 1.000000000000000000, 0.9238795325112867385, 1.000000000000000000, 0.9324923983805685213, 0.9847233224627454096) ) ) 
 REPRESENTATION_ITEM ( '' )  SURFACE ( )  );
#35310 = ORIENTED_EDGE ( 'NONE', *, *, #6550, .T. ) ;
#35311 = CARTESIAN_POINT ( 'NONE',  ( -22.37417161799345777, -19.75879703283636957, 69.17417994536339165 ) ) ;
#35312 = ADVANCED_FACE ( 'NONE', ( #27588 ), #42627, .T. ) ;
#35313 = CARTESIAN_POINT ( 'NONE',  ( 23.52590614458706852, 3.790747609047893540, 50.53028072113869484 ) ) ;
#35314 = EDGE_CURVE ( 'NONE', #26221, #43409, #4953, .T. ) ;
#35315 = ORIENTED_EDGE ( 'NONE', *, *, #14484, .F. ) ;
#35316 = CARTESIAN_POINT ( 'NONE',  ( -10.60402983012795808, -16.62626367578652520, 57.83193508283319773 ) ) ;
#35317 = DIRECTION ( 'NONE',  ( -2.866981220435666553E-17, 1.000000000000000000, 1.190614954331866791E-16 ) ) ;
#35318 = ADVANCED_FACE ( 'NONE', ( #5435 ), #5909, .T. ) ;
#35320 = EDGE_CURVE ( 'NONE', #13083, #70, #48305, .T. ) ;
#35319 = ORIENTED_EDGE ( 'NONE', *, *, #39347, .T. ) ;
#35321 = CARTESIAN_POINT ( 'NONE',  ( -13.88293547364789049, -20.90532801101632643, 68.75625136993008368 ) ) ;
#35322 = EDGE_CURVE ( 'NONE', #37238, #31278, #17934, .T. ) ;
#35323 = CARTESIAN_POINT ( 'NONE',  ( -21.89264518680100835, -20.26253109894388160, 58.77915004610761684 ) ) ;
#35324 = CIRCLE ( 'NONE', #14836, 4.686499999999998778 ) ;
#35325 =( BOUNDED_CURVE ( )  B_SPLINE_CURVE ( 3, ( #43629, #39679, #36446, #47326 ),
 .UNSPECIFIED., .F., .F. ) 
 B_SPLINE_CURVE_WITH_KNOTS ( ( 4, 4 ),
 ( 6.147240100463205792, 6.283185307179586232 ),
 .UNSPECIFIED. ) 
 CURVE ( )  GEOMETRIC_REPRESENTATION_ITEM ( )  RATIONAL_B_SPLINE_CURVE ( ( 1.000000000000000000, 0.9984605012767906462, 0.9984605012767906462, 1.000000000000000000 ) ) 
 REPRESENTATION_ITEM ( '' )  );
#35326 = CARTESIAN_POINT ( 'NONE',  ( -21.79997194174348607, -9.271457673084677609, 70.27565669584988939 ) ) ;
#35327 = ORIENTED_EDGE ( 'NONE', *, *, #10436, .F. ) ;
#35328 = DIRECTION ( 'NONE',  ( -6.865757635625664415E-07, -1.412849153005328843E-06, -0.9999999999987663202 ) ) ;
#35329 = CARTESIAN_POINT ( 'NONE',  ( -45.92409385541306222, -14.80920654474410902, 71.85000000000000853 ) ) ;
#35330 =( BOUNDED_SURFACE ( )  B_SPLINE_SURFACE ( 3, 1, ( 
 ( #28425, #31633 ),
 ( #9718, #35790 ),
 ( #42721, #46412 ),
 ( #16344, #31136 ),
 ( #38764, #16828 ),
 ( #35063, #13128 ),
 ( #46656, #5539 ) ),
 .UNSPECIFIED., .T., .F., .F. ) 
 B_SPLINE_SURFACE_WITH_KNOTS ( ( 4, 3, 4 ),
 ( 2, 2 ),
 ( 0.000000000000000000, 0.5000000000000000000, 1.000000000000000000 ),
 ( 0.000000000000000000, 1.000000000000000000 ),
 .UNSPECIFIED. ) 
 GEOMETRIC_REPRESENTATION_ITEM ( )  RATIONAL_B_SPLINE_SURFACE ( (
 ( 1.000000000000000000, 1.000000000000000000),
 ( 0.3333333333333335369, 0.3333333333333330373),
 ( 0.3333333333333335369, 0.3333333333333330373),
 ( 1.000000000000000000, 1.000000000000000000),
 ( 0.3333333333333333703, 0.3333333333333333703),
 ( 0.3333333333333333703, 0.3333333333333333703),
 ( 1.000000000000000000, 1.000000000000000000) ) ) 
 REPRESENTATION_ITEM ( '' )  SURFACE ( )  );
#35331 = AXIS2_PLACEMENT_3D ( 'NONE', #47028, #28329, #6396 ) ;
#35333 = CARTESIAN_POINT ( 'NONE',  ( -11.24322483140283069, -11.41063336453235166, 60.88705523236457395 ) ) ;
#35332 = AXIS2_PLACEMENT_3D ( 'NONE', #21233, #36233, #17993 ) ;
#35334 = FACE_BOUND ( 'NONE', #21339, .T. ) ;
#35335 = DIRECTION ( 'NONE',  ( -0.1240347345892083702, 0.000000000000000000, -0.9922778767136676281 ) ) ;
#35336 = DIRECTION ( 'NONE',  ( 0.9180681052388952601, -0.3964226963016431737, 0.000000000000000000 ) ) ;
#35337 = CARTESIAN_POINT ( 'NONE',  ( -12.85169559483840374, -15.89028456787280952, 49.52966884056655772 ) ) ;
#35338 = ORIENTED_EDGE ( 'NONE', *, *, #3191, .F. ) ;
#35339 = CARTESIAN_POINT ( 'NONE',  ( -23.71751471349159601, -11.63122711669449494, 63.23746208799618529 ) ) ;
#35340 = VECTOR ( 'NONE', #2930, 1000.000000000000000 ) ;
#35341 = ORIENTED_EDGE ( 'NONE', *, *, #35447, .T. ) ;
#35342 = DIRECTION ( 'NONE',  ( -3.071710424422018668E-17, 6.404604876783312462E-16, 1.000000000000000000 ) ) ;
#35343 = FACE_OUTER_BOUND ( 'NONE', #36449, .T. ) ;
#35344 = ORIENTED_EDGE ( 'NONE', *, *, #30003, .T. ) ;
#35345 = CARTESIAN_POINT ( 'NONE',  ( -19.97013658168673800, -21.81073013994861398, 68.97836559665680056 ) ) ;
#35346 =( BOUNDED_CURVE ( )  B_SPLINE_CURVE ( 2, ( #8875, #45588, #7914, #1463, #23896, #27090, #38158, #27332, #16478 ),
 .UNSPECIFIED., .F., .F. ) 
 B_SPLINE_CURVE_WITH_KNOTS ( ( 3, 2, 2, 2, 3 ),
 ( 0.5000000000000002220, 0.5104166666666668517, 0.5208333333333334814, 0.5312500000000001110, 0.5416666666666667407 ),
 .UNSPECIFIED. ) 
 CURVE ( )  GEOMETRIC_REPRESENTATION_ITEM ( )  RATIONAL_B_SPLINE_CURVE ( ( 0.9999999999999983347, 0.9238795325112884038, 1.000000000000000000, 0.9238795325112867385, 1.000000000000000000, 0.9238795325112867385, 1.000000000000000000, 0.9238795325112859613, 1.000000000000000888 ) ) 
 REPRESENTATION_ITEM ( '' )  );
#35347 = CARTESIAN_POINT ( 'NONE',  ( -12.74071866071660075, -9.015263582886822391, 70.96429948631303830 ) ) ;
#35348 = ORIENTED_EDGE ( 'NONE', *, *, #3044, .T. ) ;
#35349 = EDGE_CURVE ( 'NONE', #37778, #6964, #44858, .T. ) ;
#35350 = VERTEX_POINT ( 'NONE', #25349 ) ;
#35351 = ORIENTED_EDGE ( 'NONE', *, *, #5463, .T. ) ;
#35352 = CARTESIAN_POINT ( 'NONE',  ( -10.51729497052148155, -16.22293520194095962, 71.74750383215044280 ) ) ;
#35353 = CARTESIAN_POINT ( 'NONE',  ( -24.43851978893111365, -14.10038870526526722, 73.12831301160871078 ) ) ;
#35354 = LINE ( 'NONE', #43244, #24377 ) ;
#35355 = CARTESIAN_POINT ( 'NONE',  ( -50.42409385541304800, -25.10920654474410441, 63.99999999999998579 ) ) ;
#35356 = CARTESIAN_POINT ( 'NONE',  ( -13.34492810635830651, -9.120585717833787243, 60.54836177336171943 ) ) ;
#35357 = ORIENTED_EDGE ( 'NONE', *, *, #24957, .T. ) ;
#35358 = VERTEX_POINT ( 'NONE', #25583 ) ;
#35359 = CARTESIAN_POINT ( 'NONE',  ( -20.36159385650551812, -9.295667164867525756, 49.30633214617472504 ) ) ;
#35360 = CARTESIAN_POINT ( 'NONE',  ( -13.71338950266841650, -20.80363499509022773, 64.98628881289567971 ) ) ;
#35361 = AXIS2_PLACEMENT_3D ( 'NONE', #27569, #23887, #27081 ) ;
#35362 = FACE_OUTER_BOUND ( 'NONE', #20187, .T. ) ;
#35363 = FACE_OUTER_BOUND ( 'NONE', #34207, .T. ) ;
#35364 = CARTESIAN_POINT ( 'NONE',  ( -21.99284385650551243, -7.406986770994973490, 48.81910596585309747 ) ) ;
#35365 = VECTOR ( 'NONE', #23313, 1000.000000000000000 ) ;
#35366 = VERTEX_POINT ( 'NONE', #14464 ) ;
#35367 = CARTESIAN_POINT ( 'NONE',  ( -10.93232766038821424, -17.55941949638709687, 68.38249893951126523 ) ) ;
#35368 = FACE_OUTER_BOUND ( 'NONE', #20715, .T. ) ;
#35369 = VERTEX_POINT ( 'NONE', #32494 ) ;
#35370 = CARTESIAN_POINT ( 'NONE',  ( -11.71918404020638427, -18.95175453447548009, 71.70158022526054253 ) ) ;
#35371 = CARTESIAN_POINT ( 'NONE',  ( -9.973354012397450674, -14.79738236791871664, 71.44127436690867228 ) ) ;
#35372 = LINE ( 'NONE', #6064, #32064 ) ;
#35373 = ADVANCED_FACE ( 'NONE', ( #25826 ), #2456, .T. ) ;
#35374 = ADVANCED_FACE ( 'NONE', ( #7131 ), #47995, .T. ) ;
#35375 = CARTESIAN_POINT ( 'NONE',  ( -22.43322805121811214, -20.32484237088842249, 65.89077003248591780 ) ) ;
#35376 = EDGE_LOOP ( 'NONE', ( #15852, #43884, #40363, #32652 ) ) ;
#35377 = CARTESIAN_POINT ( 'NONE',  ( -24.27331421978716364, -11.70866763410274913, 53.76227901944321275 ) ) ;
#35378 = CARTESIAN_POINT ( 'NONE',  ( -20.12289019246589206, -7.865124395032225380, 73.90592041591946781 ) ) ;
#35379 = EDGE_LOOP ( 'NONE', ( #26416, #8936, #24767, #42104 ) ) ;
#35380 = PLANE ( 'NONE',  #33798 ) ;
#35381 = ORIENTED_EDGE ( 'NONE', *, *, #34504, .T. ) ;
#35382 = CARTESIAN_POINT ( 'NONE',  ( -18.50498591074712706, -7.838904286686645406, 70.57887743023405847 ) ) ;
#35383 = EDGE_CURVE ( 'NONE', #18814, #35636, #24879, .T. ) ;
#35384 = EDGE_CURVE ( 'NONE', #7607, #15639, #4922, .T. ) ;
#35385 = CARTESIAN_POINT ( 'NONE',  ( -23.76104667403178894, -10.32500873748839787, 54.49999999999995026 ) ) ;
#35386 = ORIENTED_EDGE ( 'NONE', *, *, #27926, .F. ) ;
#35387 = FACE_OUTER_BOUND ( 'NONE', #17791, .T. ) ;
#35388 = CARTESIAN_POINT ( 'NONE',  ( -10.40181215838624240, -12.32098906055858478, 57.37211424251319158 ) ) ;
#35389 = CARTESIAN_POINT ( 'NONE',  ( -24.20371252810814866, -12.87440185077122834, 66.58774614429587757 ) ) ;
#35390 = AXIS2_PLACEMENT_3D ( 'NONE', #37117, #30505, #15691 ) ;
#35391 = CARTESIAN_POINT ( 'NONE',  ( -27.42409385541305511, -25.10920654474410441, 63.99999999999998579 ) ) ;
#35392 = ORIENTED_EDGE ( 'NONE', *, *, #26898, .F. ) ;
#35393 = CARTESIAN_POINT ( 'NONE',  ( -11.01197672498280866, -17.74032467813711378, 71.85246142747085685 ) ) ;
#35394 = AXIS2_PLACEMENT_3D ( 'NONE', #43635, #25154, #35731 ) ;
#35395 = CARTESIAN_POINT ( 'NONE',  ( -20.84966316371748363, -20.97445663613623523, 58.52986464729110594 ) ) ;
#35396 = CARTESIAN_POINT ( 'NONE',  ( -10.53876648713876740, -16.36073154998923229, 68.13334680848100788 ) ) ;
#35397 = ORIENTED_EDGE ( 'NONE', *, *, #43993, .T. ) ;
#35398 = CARTESIAN_POINT ( 'NONE',  ( -15.75439910800316845, -7.548642891367095764, 67.18361323375314953 ) ) ;
#35399 = VECTOR ( 'NONE', #3139, 1000.000000000000000 ) ;
#35400 = CARTESIAN_POINT ( 'NONE',  ( -21.78913871579879569, -8.771809629715434653, 70.24637254705723421 ) ) ;
#35401 = EDGE_CURVE ( 'NONE', #16630, #20066, #21652, .T. ) ;
#35402 = ORIENTED_EDGE ( 'NONE', *, *, #16023, .F. ) ;
#35403 = ORIENTED_EDGE ( 'NONE', *, *, #14205, .T. ) ;
#35404 = CARTESIAN_POINT ( 'NONE',  ( -23.83724620116612058, -11.87385095858915207, 63.36706934938042934 ) ) ;
#35405 = CARTESIAN_POINT ( 'NONE',  ( -20.04136243794045313, -21.30156843505427489, 72.69013421047081636 ) ) ;
#35406 = CARTESIAN_POINT ( 'NONE',  ( -10.42707437396587800, -14.56501430223373106, 71.39952884310628178 ) ) ;
#35407 = VECTOR ( 'NONE', #40272, 1000.000000000000000 ) ;
#35408 = CARTESIAN_POINT ( 'NONE',  ( -19.37409385650551741, -9.792211528768504536, 50.49490371617623197 ) ) ;
#35409 = CARTESIAN_POINT ( 'NONE',  ( -14.46752719259218622, -19.14754880513559598, 52.02966884056656482 ) ) ;
#35410 = CARTESIAN_POINT ( 'NONE',  ( -12.36127418495607877, -19.64332424046381576, 57.99970467312913058 ) ) ;
#35411 = CARTESIAN_POINT ( 'NONE',  ( -19.76620107553464933, -21.88153087662584895, 65.57147903976517966 ) ) ;
#35412 = CARTESIAN_POINT ( 'NONE',  ( -16.78341213209640159, -22.23169296657789928, 68.88056055876903372 ) ) ;
#35413 = ORIENTED_EDGE ( 'NONE', *, *, #34226, .F. ) ;
#35414 = ORIENTED_EDGE ( 'NONE', *, *, #48263, .F. ) ;
#35415 = CARTESIAN_POINT ( 'NONE',  ( -12.34237343482028670, -20.25724347209099818, 68.49803924141983202 ) ) ;
#35416 = DIRECTION ( 'NONE',  ( -2.866981220435666553E-17, 1.000000000000000000, 1.190614954331866791E-16 ) ) ;
#35417 = CARTESIAN_POINT ( 'NONE',  ( -24.55871722839809834, -12.66422925090921225, 69.88747596251579353 ) ) ;
#35418 =( BOUNDED_CURVE ( )  B_SPLINE_CURVE ( 3, ( #18608, #9853, #10088, #45238 ),
 .UNSPECIFIED., .F., .F. ) 
 B_SPLINE_CURVE_WITH_KNOTS ( ( 4, 4 ),
 ( 0.9074455897393695070, 1.000000000000000000 ),
 .UNSPECIFIED. ) 
 CURVE ( )  GEOMETRIC_REPRESENTATION_ITEM ( )  RATIONAL_B_SPLINE_CURVE ( ( 0.6983129098261139367, 0.7760317562607162989, 0.8765941196520116163, 1.000000000000000000 ) ) 
 REPRESENTATION_ITEM ( '' )  );
#35419 = FACE_OUTER_BOUND ( 'NONE', #21545, .T. ) ;
#35420 = VERTEX_POINT ( 'NONE', #21175 ) ;
#35421 = CARTESIAN_POINT ( 'NONE',  ( -19.92776479198160189, -21.39998277484045275, 72.41950795000725805 ) ) ;
#35422 = DIRECTION ( 'NONE',  ( -1.000000000000000000, -2.866981220435666553E-17, 0.000000000000000000 ) ) ;
#35423 = VECTOR ( 'NONE', #34728, 1000.000000000000000 ) ;
#35424 = DIRECTION ( 'NONE',  ( 0.000000000000000000, -0.9999954153791273948, -0.003028072113819838245 ) ) ;
#35425 = DIRECTION ( 'NONE',  ( -3.549360974551883545E-17, 6.371834667872732552E-18, 1.000000000000000000 ) ) ;
#35426 = ORIENTED_EDGE ( 'NONE', *, *, #8985, .T. ) ;
#35427 = VECTOR ( 'NONE', #42473, 1000.000000000000000 ) ;
#35428 = CARTESIAN_POINT ( 'NONE',  ( -23.51785832295892931, -11.36449550514380036, 69.89210750611785272 ) ) ;
#35429 = DIRECTION ( 'NONE',  ( -0.3478314405900307937, -0.9375570856950865561, 0.000000000000000000 ) ) ;
#35430 = EDGE_CURVE ( 'NONE', #38940, #34024, #2555, .T. ) ;
#35431 = CARTESIAN_POINT ( 'NONE',  ( -24.42401644153718721, -14.84212863923847081, 59.24300237020570137 ) ) ;
#35432 = VECTOR ( 'NONE', #47180, 1000.000000000000000 ) ;
#35433 = DIRECTION ( 'NONE',  ( -1.000000000000000000, -2.866981220435666553E-17, 0.000000000000000000 ) ) ;
#35434 = CARTESIAN_POINT ( 'NONE',  ( -24.25171796977671335, -16.35308120058899206, 59.42332432118549690 ) ) ;
#35435 = ORIENTED_EDGE ( 'NONE', *, *, #37886, .F. ) ;
#35436 = FACE_OUTER_BOUND ( 'NONE', #15720, .T. ) ;
#35437 = ORIENTED_EDGE ( 'NONE', *, *, #11263, .F. ) ;
#35438 = ADVANCED_FACE ( 'NONE', ( #43837 ), #36891, .T. ) ;
#35439 = CARTESIAN_POINT ( 'NONE',  ( -19.24931602816760190, -7.586122295205923294, 63.55372364550890296 ) ) ;
#35440 = CARTESIAN_POINT ( 'NONE',  ( -18.76558283008973049, -7.480892646508040755, 70.55563411965815135 ) ) ;
#35441 = ORIENTED_EDGE ( 'NONE', *, *, #37879, .F. ) ;
#35442 = CARTESIAN_POINT ( 'NONE',  ( -13.88293403466071396, -20.90532716339074781, 68.60625136993937190 ) ) ;
#35443 = AXIS2_PLACEMENT_3D ( 'NONE', #8438, #34528, #4265 ) ;
#35444 = EDGE_CURVE ( 'NONE', #1437, #45729, #33289, .T. ) ;
#35445 = CARTESIAN_POINT ( 'NONE',  ( -17.38034385650551883, -6.424090610841176385, 49.80797279389978627 ) ) ;
#35446 = ORIENTED_EDGE ( 'NONE', *, *, #14686, .F. ) ;
#35447 = EDGE_CURVE ( 'NONE', #37610, #21448, #40131, .T. ) ;
#35448 = CARTESIAN_POINT ( 'NONE',  ( -15.16478962180274870, -8.127860897350485558, 57.26488623981089177 ) ) ;
#35449 = CARTESIAN_POINT ( 'NONE',  ( -13.49267557974227394, -8.956801037788498121, 60.45422421514565059 ) ) ;
#35450 = VERTEX_POINT ( 'NONE', #48228 ) ;
#35451 = CARTESIAN_POINT ( 'NONE',  ( -24.72409385541305582, -14.90920654474415663, 62.92941176470587550 ) ) ;
#35452 = CARTESIAN_POINT ( 'NONE',  ( -10.85841931818429629, -17.37798394237199062, 64.91267318220633342 ) ) ;
#35453 = DIRECTION ( 'NONE',  ( 0.1240347345892086200, -1.145860353393066553E-16, 0.9922778767136676281 ) ) ;
#35454 = CARTESIAN_POINT ( 'NONE',  ( -21.15336808330806662, -20.73310000539657949, 69.35450185099439580 ) ) ;
#35455 = CARTESIAN_POINT ( 'NONE',  ( -12.15299190543910512, -20.07505386821981119, 65.05330132703942070 ) ) ;
#35456 = VERTEX_POINT ( 'NONE', #238 ) ;
#35457 = ORIENTED_EDGE ( 'NONE', *, *, #6757, .T. ) ;
#35458 = CARTESIAN_POINT ( 'NONE',  ( -24.11881394502254849, -17.01995806294775448, 73.16863963025599560 ) ) ;
#35459 = VERTEX_POINT ( 'NONE', #7870 ) ;
#35460 = CARTESIAN_POINT ( 'NONE',  ( -24.33993967182187035, -15.89175611583846681, 66.07827301765077266 ) ) ;
#35461 = DIRECTION ( 'NONE',  ( 0.9687793358424821033, -0.2479245821708679909, 0.000000000000000000 ) ) ;
#35462 = CARTESIAN_POINT ( 'NONE',  ( -17.99909385759799108, -8.105421454601382081, 49.25000573077640098 ) ) ;
#35463 =( BOUNDED_CURVE ( )  B_SPLINE_CURVE ( 3, ( #37379, #2696, #36898, #26325 ),
 .UNSPECIFIED., .F., .F. ) 
 B_SPLINE_CURVE_WITH_KNOTS ( ( 4, 4 ),
 ( 0.000000000000000000, 0.4074455897393662873 ),
 .UNSPECIFIED. ) 
 CURVE ( )  GEOMETRIC_REPRESENTATION_ITEM ( )  RATIONAL_B_SPLINE_CURVE ( ( 1.000000000000000000, 0.4567392136813298587, 0.3561768502900295452, 0.6983129098260991707 ) ) 
 REPRESENTATION_ITEM ( '' )  );
#35464 = DIRECTION ( 'NONE',  ( -5.731567514496413899E-31, -1.020425574103664789E-16, -1.000000000000000000 ) ) ;
#35465 = CYLINDRICAL_SURFACE ( 'NONE', #7407, 0.1500000000000010769 ) ;
#35466 = CIRCLE ( 'NONE', #29184, 1.250000000000007994 ) ;
#35467 = EDGE_LOOP ( 'NONE', ( #9207, #24776, #2041, #39056, #39871 ) ) ;
#35468 = CARTESIAN_POINT ( 'NONE',  ( -22.94346461125903147, -10.41716915086503725, 66.63362387568147938 ) ) ;
#35469 = CARTESIAN_POINT ( 'NONE',  ( -13.00192122862099531, -8.813424762390464906, 64.06979850922034814 ) ) ;
#35470 = AXIS2_PLACEMENT_3D ( 'NONE', #39180, #38702, #4983 ) ;
#35471 = CARTESIAN_POINT ( 'NONE',  ( -24.03160971261424805, -17.26750559640275640, 69.71339792588547368 ) ) ;
#35472 = CARTESIAN_POINT ( 'NONE',  ( -12.97018521796328017, -9.340428432532196013, 74.73411830381819243 ) ) ;
#35473 = FACE_OUTER_BOUND ( 'NONE', #36627, .T. ) ;
#35474 = B_SPLINE_CURVE_WITH_KNOTS ( 'NONE', 3,
 ( #2632, #17405, #28505, #2144, #3111, #28741, #36827, #21364, #32438, #17145 ),
 .UNSPECIFIED., .F., .F.,
 ( 4, 2, 2, 2, 4 ),
 ( 0.000000000000000000, 0.2500000000000000000, 0.5000000000000000000, 0.7500000000000000000, 1.000000000000000000 ),
 .UNSPECIFIED. ) ;
#35475 =( BOUNDED_CURVE ( )  B_SPLINE_CURVE ( 3, ( #42969, #35333, #21299, #28914 ),
 .UNSPECIFIED., .F., .F. ) 
 B_SPLINE_CURVE_WITH_KNOTS ( ( 4, 4 ),
 ( 0.000000000000000000, 0.4074455897393631787 ),
 .UNSPECIFIED. ) 
 CURVE ( )  GEOMETRIC_REPRESENTATION_ITEM ( )  RATIONAL_B_SPLINE_CURVE ( ( 1.000000000000000000, 0.4567392136813281378, 0.3561768502900288791, 0.6983129098261022794 ) ) 
 REPRESENTATION_ITEM ( '' )  );
#35476 = ORIENTED_EDGE ( 'NONE', *, *, #27195, .F. ) ;
#35477 = VERTEX_POINT ( 'NONE', #34417 ) ;
#35478 = EDGE_LOOP ( 'NONE', ( #2211, #25476, #32857, #44906 ) ) ;
#35479 = CARTESIAN_POINT ( 'NONE',  ( -23.28921155407422106, -22.22116534042542213, 53.49999999999995026 ) ) ;
#35480 = AXIS2_PLACEMENT_3D ( 'NONE', #40296, #35852, #13195 ) ;
#35481 = CARTESIAN_POINT ( 'NONE',  ( -45.85858821786030859, -14.20920654474410760, 71.05212771298751306 ) ) ;
#35482 = CARTESIAN_POINT ( 'NONE',  ( -21.74938187378823784, -9.305322344061284667, 63.47688388556134242 ) ) ;
#35483 = B_SPLINE_CURVE_WITH_KNOTS ( 'NONE', 3,
 ( #10010, #16894, #14154, #47201, #20621, #10264, #6317, #2850, #39563, #46948 ),
 .UNSPECIFIED., .F., .F.,
 ( 4, 2, 2, 2, 4 ),
 ( 0.000000000000000000, 0.2500000000000000000, 0.5000000000000000000, 0.7500000000000000000, 1.000000000000000000 ),
 .UNSPECIFIED. ) ;
#35484 = EDGE_CURVE ( 'NONE', #21822, #2374, #213, .T. ) ;
#35485 = ORIENTED_EDGE ( 'NONE', *, *, #3727, .F. ) ;
#35486 = CARTESIAN_POINT ( 'NONE',  ( -50.42609385541305755, -14.90920654474416907, 63.93529411764704662 ) ) ;
#35487 = CIRCLE ( 'NONE', #4824, 1.999999999999999334 ) ;
#35488 = CARTESIAN_POINT ( 'NONE',  ( -10.42131017383741032, -15.64935787052201910, 57.45304097017945111 ) ) ;
#35489 = VERTEX_POINT ( 'NONE', #38119 ) ;
#35490 = B_SPLINE_CURVE_WITH_KNOTS ( 'NONE', 3,
 ( #25500, #40512, #43999, #40755, #47912, #40044, #6059, #6789, #33106, #6310 ),
 .UNSPECIFIED., .F., .F.,
 ( 4, 2, 2, 2, 4 ),
 ( 0.000000000000000000, 0.2500000000000000000, 0.5000000000000000000, 0.7500000000000000000, 1.000000000000000000 ),
 .UNSPECIFIED. ) ;
#35491 = AXIS2_PLACEMENT_3D ( 'NONE', #42924, #34549, #833 ) ;
#35492 = DIRECTION ( 'NONE',  ( -3.071710424422018668E-17, 6.404604876783312462E-16, 1.000000000000000000 ) ) ;
#35493 = CARTESIAN_POINT ( 'NONE',  ( -23.78474285830518653, -17.73496384451835794, 62.70190779623644062 ) ) ;
#35494 = ORIENTED_EDGE ( 'NONE', *, *, #33812, .F. ) ;
#35495 = CARTESIAN_POINT ( 'NONE',  ( -48.42409385541304800, -25.10920654474410441, 47.99999999999998579 ) ) ;
#35496 = VERTEX_POINT ( 'NONE', #11796 ) ;
#35497 = FACE_OUTER_BOUND ( 'NONE', #9254, .T. ) ;
#35498 = ORIENTED_EDGE ( 'NONE', *, *, #44962, .F. ) ;
#35499 = CARTESIAN_POINT ( 'NONE',  ( -24.87385082706414607, -14.87839859077033822, 59.49946141495512819 ) ) ;
#35500 = DIRECTION ( 'NONE',  ( 3.071710424422018668E-17, -6.404604876783312462E-16, -1.000000000000000000 ) ) ;
#35501 = CARTESIAN_POINT ( 'NONE',  ( -19.30706997687812887, -22.01740875295033462, 58.64012098774584558 ) ) ;
#35502 = VERTEX_POINT ( 'NONE', #26566 ) ;
#35503 = CARTESIAN_POINT ( 'NONE',  ( -17.42409385541299471, -14.80920654474435594, 52.02966884056656482 ) ) ;
#35504 = CARTESIAN_POINT ( 'NONE',  ( -24.70168866369219529, -16.40345363474641260, 59.28365756255518448 ) ) ;
#35505 = EDGE_CURVE ( 'NONE', #16942, #38159, #17909, .T. ) ;
#35506 = DIRECTION ( 'NONE',  ( 0.000000000000000000, 0.000000000000000000, 1.000000000000000000 ) ) ;
#35507 = AXIS2_PLACEMENT_3D ( 'NONE', #29011, #43323, #21862 ) ;
#35508 = ADVANCED_FACE ( 'NONE', ( #11541 ), #33941, .T. ) ;
#35509 = DIRECTION ( 'NONE',  ( -1.000000000000000000, 4.164305804376849172E-17, -1.614929280266638808E-16 ) ) ;
#35510 = CARTESIAN_POINT ( 'NONE',  ( -10.46835785932885621, -15.59614926455694572, 61.03789074737235154 ) ) ;
#35511 = B_SPLINE_CURVE_WITH_KNOTS ( 'NONE', 1,
 ( #32835, #22256 ),
 .UNSPECIFIED., .F., .F.,
 ( 2, 2 ),
 ( 0.000000000000000000, 1.000000000000000000 ),
 .UNSPECIFIED. ) ;
#35512 = LINE ( 'NONE', #31824, #29783 ) ;
#35513 = ORIENTED_EDGE ( 'NONE', *, *, #44427, .F. ) ;
#35514 = PLANE ( 'NONE',  #23936 ) ;
#35515 = CARTESIAN_POINT ( 'NONE',  ( -13.01616685277437568, -9.306763517318225709, 70.86397465682092900 ) ) ;
#35516 = DIRECTION ( 'NONE',  ( -0.9893521221787096032, 0.1455416721783832079, 6.188545272020283923E-08 ) ) ;
#35517 = DIRECTION ( 'NONE',  ( 0.000000000000000000, 0.000000000000000000, -1.000000000000000000 ) ) ;
#35518 = EDGE_CURVE ( 'NONE', #39956, #15214, #35928, .T. ) ;
#35519 = CARTESIAN_POINT ( 'NONE',  ( -19.97164353606484255, -21.81018995992316079, 69.11977899231902711 ) ) ;
#35520 = CARTESIAN_POINT ( 'NONE',  ( -17.74284385650551599, -8.811426318492348031, 52.18089403414751359 ) ) ;
#35521 = AXIS2_PLACEMENT_3D ( 'NONE', #18477, #48281, #14283 ) ;
#35522 = EDGE_LOOP ( 'NONE', ( #36590, #5935, #33274, #6621 ) ) ;
#35523 = DIRECTION ( 'NONE',  ( 0.000000000000000000, 1.000000000000000000, 0.000000000000000000 ) ) ;
#35524 = ORIENTED_EDGE ( 'NONE', *, *, #23253, .T. ) ;
#35525 = CARTESIAN_POINT ( 'NONE',  ( -11.52461732454066023, -18.67456722079397125, 68.63178522425482697 ) ) ;
#35526 = DIRECTION ( 'NONE',  ( -3.071710424422018668E-17, 6.404604876783312462E-16, 1.000000000000000000 ) ) ;
#35527 = LINE ( 'NONE', #2528, #34944 ) ;
#35528 = CARTESIAN_POINT ( 'NONE',  ( -23.09608884140482132, -18.99645705127922923, 62.35966695639078239 ) ) ;
#35529 = CYLINDRICAL_SURFACE ( 'NONE', #23463, 0.3999999999999975797 ) ;
#35530 = EDGE_CURVE ( 'NONE', #8372, #11939, #26531, .T. ) ;
#35531 = VERTEX_POINT ( 'NONE', #12035 ) ;
#35532 = CARTESIAN_POINT ( 'NONE',  ( -12.09375059738624714, -9.604167670197291784, 57.22789050401003408 ) ) ;
#35533 = FACE_OUTER_BOUND ( 'NONE', #40742, .T. ) ;
#35534 = VECTOR ( 'NONE', #22597, 1000.000000000000114 ) ;
#35535 = DIRECTION ( 'NONE',  ( -3.071710424422018668E-17, 6.404604876783312462E-16, 1.000000000000000000 ) ) ;
#35536 = EDGE_LOOP ( 'NONE', ( #8736, #4252, #39389, #4789, #21093 ) ) ;
#35537 = CARTESIAN_POINT ( 'NONE',  ( -17.22121256223034536, -7.361891212656819228, 70.74681744497029001 ) ) ;
#35538 = CIRCLE ( 'NONE', #4096, 1.500000000000001332 ) ;
#35539 = CARTESIAN_POINT ( 'NONE',  ( -41.30129973776600139, -14.80920654474425291, 71.98235294117645822 ) ) ;
#35540 = DIRECTION ( 'NONE',  ( -3.071710424422018668E-17, 6.404604876783312462E-16, 1.000000000000000000 ) ) ;
#35541 = CARTESIAN_POINT ( 'NONE',  ( -16.48034385759799392, -9.360768649639298999, 51.01397948905923130 ) ) ;
#35542 = CARTESIAN_POINT ( 'NONE',  ( -20.95545100651803594, -20.91135505560678354, 65.59926067308570907 ) ) ;
#35543 = ORIENTED_EDGE ( 'NONE', *, *, #25497, .F. ) ;
#35544 = ORIENTED_EDGE ( 'NONE', *, *, #12988, .T. ) ;
#35545 = CARTESIAN_POINT ( 'NONE',  ( -21.34284385541304374, -7.587656875400192291, 49.25157356644813689 ) ) ;
#35546 = DIRECTION ( 'NONE',  ( 0.8603613874411337736, -0.3191920208248667512, 0.3973597071195127395 ) ) ;
#35547 = CARTESIAN_POINT ( 'NONE',  ( -14.11518482969570876, -8.134170225034605295, 70.89104128859074194 ) ) ;
#35548 = EDGE_CURVE ( 'NONE', #18372, #4771, #4815, .T. ) ;
#35549 = PLANE ( 'NONE',  #46905 ) ;
#35550 = CARTESIAN_POINT ( 'NONE',  ( -23.77487038158592014, -11.74745262826995429, 62.96690348473899235 ) ) ;
#35551 = DIRECTION ( 'NONE',  ( -7.110378524392051906E-06, -9.728165310344191876E-06, 0.9999999999274027385 ) ) ;
#35552 = EDGE_LOOP ( 'NONE', ( #4134, #27139, #4152, #8540, #4033 ) ) ;
#35553 = DIRECTION ( 'NONE',  ( 1.927470528863184130E-16, 1.434740771370715221E-29, -1.000000000000000000 ) ) ;
#35554 = CARTESIAN_POINT ( 'NONE',  ( -21.57946453887431204, -8.565578233975859490, 54.27966884056655061 ) ) ;
#35555 = ORIENTED_EDGE ( 'NONE', *, *, #32635, .F. ) ;
#35556 = CARTESIAN_POINT ( 'NONE',  ( -24.18037252889021005, -17.94870914462638822, 59.18873732074431615 ) ) ;
#35557 = EDGE_CURVE ( 'NONE', #30449, #27032, #17648, .T. ) ;
#35558 = VERTEX_POINT ( 'NONE', #18671 ) ;
#35559 = CARTESIAN_POINT ( 'NONE',  ( -17.63866254341385442, -7.362211269489866261, 63.66561597723832477 ) ) ;
#35560 = CARTESIAN_POINT ( 'NONE',  ( -18.63519442141342353, -21.70370385402750912, 72.51184200825215953 ) ) ;
#35561 = VERTEX_POINT ( 'NONE', #45293 ) ;
#35562 = CARTESIAN_POINT ( 'NONE',  ( -18.19389434033494268, -22.21941471489327569, 65.53027570717884487 ) ) ;
#35563 = ADVANCED_FACE ( 'NONE', ( #45539 ), #38336, .T. ) ;
#35564 = CARTESIAN_POINT ( 'NONE',  ( -12.01648161716052776, -10.28590799842451098, 67.79896869921920199 ) ) ;
#35565 = B_SPLINE_CURVE_WITH_KNOTS ( 'NONE', 3,
 ( #32802, #22221, #47831, #21729, #18013, #33033, #26645, #15290, #34503, #45618 ),
 .UNSPECIFIED., .F., .F.,
 ( 4, 2, 2, 2, 4 ),
 ( 0.1272669073658538319, 0.2522669073463332245, 0.3772669073268126727, 0.5022669073072920654, 0.6272669072877714580 ),
 .UNSPECIFIED. ) ;
#35566 = B_SPLINE_CURVE_WITH_KNOTS ( 'NONE', 1,
 ( #5417, #23894 ),
 .UNSPECIFIED., .F., .F.,
 ( 2, 2 ),
 ( 0.000000000000000000, 1.000000000000000000 ),
 .UNSPECIFIED. ) ;
#35567 = LINE ( 'NONE', #31882, #31335 ) ;
#35568 = CARTESIAN_POINT ( 'NONE',  ( -8.039996143071578061, -9.893874759132541996, 53.49999999999995026 ) ) ;
#35569 = ORIENTED_EDGE ( 'NONE', *, *, #12366, .T. ) ;
#35570 = CARTESIAN_POINT ( 'NONE',  ( -10.62096356601691660, -12.92974252456203743, 60.95420737114066156 ) ) ;
#35571 = DIRECTION ( 'NONE',  ( -0.000000000000000000, -1.000000000000000000, -0.000000000000000000 ) ) ;
#35572 = CARTESIAN_POINT ( 'NONE',  ( -11.05863916172663330, -11.77843433669154827, 71.38301090529685666 ) ) ;
#35573 = EDGE_CURVE ( 'NONE', #3501, #12328, #8977, .T. ) ;
#35574 = CARTESIAN_POINT ( 'NONE',  ( -18.77534723317123877, -22.20510239617831516, 54.02312124697527906 ) ) ;
#35575 = CARTESIAN_POINT ( 'NONE',  ( -22.04378365035703879, -20.13510231884741231, 62.24911246861644543 ) ) ;
#35576 = CARTESIAN_POINT ( 'NONE',  ( 18.54465614458695910, 3.140487395509476976, 50.61810660878216339 ) ) ;
#35577 = VERTEX_POINT ( 'NONE', #41334 ) ;
#35578 = DIRECTION ( 'NONE',  ( 0.9757441136919974278, 0.2189141945955501434, 0.000000000000000000 ) ) ;
#35579 = EDGE_CURVE ( 'NONE', #1628, #18527, #9802, .T. ) ;
#35580 = CARTESIAN_POINT ( 'NONE',  ( -19.36557164464469594, -19.08778335711045671, 52.02966884056656482 ) ) ;
#35581 = B_SPLINE_CURVE_WITH_KNOTS ( 'NONE', 3,
 ( #12748, #15943, #944, #42793, #46245, #30986, #19898, #23118, #38346, #4390 ),
 .UNSPECIFIED., .F., .F.,
 ( 4, 2, 2, 2, 4 ),
 ( 0.6272669072878013230, 0.7522669073073041668, 0.8772669073268071216, 1.002266907346309965, 1.127266907365812809 ),
 .UNSPECIFIED. ) ;
#35582 = VERTEX_POINT ( 'NONE', #44805 ) ;
#35583 = CARTESIAN_POINT ( 'NONE',  ( -19.60932529797995727, -21.51514414075818493, 69.34971148877966129 ) ) ;
#35584 = ORIENTED_EDGE ( 'NONE', *, *, #38689, .F. ) ;
#35585 = EDGE_LOOP ( 'NONE', ( #16753, #39469 ) ) ;
#35586 = ORIENTED_EDGE ( 'NONE', *, *, #32771, .T. ) ;
#35587 = LINE ( 'NONE', #9752, #38307 ) ;
#35588 = DIRECTION ( 'NONE',  ( -1.000000000000000000, 0.000000000000000000, 0.000000000000000000 ) ) ;
#35589 = CARTESIAN_POINT ( 'NONE',  ( -17.38444741023572959, -7.359303210311908927, 67.22028379401484699 ) ) ;
#35590 = ADVANCED_FACE ( 'NONE', ( #11062 ), #26084, .T. ) ;
#35591 = CARTESIAN_POINT ( 'NONE',  ( -17.04413539470109740, -21.84925844046378174, 72.45071136019464575 ) ) ;
#35592 = CARTESIAN_POINT ( 'NONE',  ( -23.48344415125163565, -18.41350569598871090, 73.04896097104848707 ) ) ;
#35593 = ADVANCED_FACE ( 'NONE', ( #12757 ), #31800, .T. ) ;
#35594 = EDGE_LOOP ( 'NONE', ( #29717, #1275, #43394, #41590, #1928, #15116, #12604, #13884 ) ) ;
#35595 = ORIENTED_EDGE ( 'NONE', *, *, #37765, .F. ) ;
#35596 = CARTESIAN_POINT ( 'NONE',  ( -20.86784385650551954, -6.428312510596451368, 51.20221977374900035 ) ) ;
#35597 = EDGE_CURVE ( 'NONE', #31055, #7816, #25389, .T. ) ;
#35598 = CARTESIAN_POINT ( 'NONE',  ( -21.48052744822966531, -21.05892743585564375, 72.71101825924023387 ) ) ;
#35599 = CARTESIAN_POINT ( 'NONE',  ( -12.61628475940923089, -19.96571365470544990, 68.34217200571772821 ) ) ;
#35600 =( BOUNDED_CURVE ( )  B_SPLINE_CURVE ( 3, ( #28915, #2806, #28447, #32836 ),
 .UNSPECIFIED., .F., .F. ) 
 B_SPLINE_CURVE_WITH_KNOTS ( ( 4, 4 ),
 ( 0.4074455897393610138, 0.5000000000000000000 ),
 .UNSPECIFIED. ) 
 CURVE ( )  GEOMETRIC_REPRESENTATION_ITEM ( )  RATIONAL_B_SPLINE_CURVE ( ( 0.6983129098260827394, 0.7760317562607027542, 0.8765941196520123935, 1.000000000000021316 ) ) 
 REPRESENTATION_ITEM ( '' )  );
#35601 = CARTESIAN_POINT ( 'NONE',  ( -22.10534385650551670, -8.801233750844183135, 48.81488406609782515 ) ) ;
#35602 = ORIENTED_EDGE ( 'NONE', *, *, #18831, .F. ) ;
#35603 = FACE_OUTER_BOUND ( 'NONE', #524, .T. ) ;
#35604 = DIRECTION ( 'NONE',  ( 3.549360974551883545E-17, -6.371834667872732552E-18, -1.000000000000000000 ) ) ;
#35605 = DIRECTION ( 'NONE',  ( 0.8017593358536257986, 0.5976470257363775129, -1.209213344958501974E-07 ) ) ;
#35606 = ORIENTED_EDGE ( 'NONE', *, *, #14894, .F. ) ;
#35607 = CARTESIAN_POINT ( 'NONE',  ( -11.73051513911133981, -18.96706119963912940, 71.69245704744217562 ) ) ;
#35608 =( BOUNDED_SURFACE ( )  B_SPLINE_SURFACE ( 3, 1, ( 
 ( #427, #48187 ),
 ( #14417, #41288 ),
 ( #7573, #29478 ),
 ( #44508, #12224 ),
 ( #23562, #45741 ),
 ( #19865, #27001 ),
 ( #15904, #27244 ) ),
 .UNSPECIFIED., .T., .F., .F. ) 
 B_SPLINE_SURFACE_WITH_KNOTS ( ( 4, 3, 4 ),
 ( 2, 2 ),
 ( 0.000000000000000000, 0.5000000000000000000, 1.000000000000000000 ),
 ( 0.000000000000000000, 1.000000000000000000 ),
 .UNSPECIFIED. ) 
 GEOMETRIC_REPRESENTATION_ITEM ( )  RATIONAL_B_SPLINE_SURFACE ( (
 ( 1.000000000000000000, 1.000000000000000000),
 ( 0.3333333333333335369, 0.3333333333333330373),
 ( 0.3333333333333335369, 0.3333333333333330373),
 ( 1.000000000000000000, 1.000000000000000000),
 ( 0.3333333333333333703, 0.3333333333333333703),
 ( 0.3333333333333333703, 0.3333333333333333703),
 ( 1.000000000000000000, 1.000000000000000000) ) ) 
 REPRESENTATION_ITEM ( '' )  SURFACE ( )  );
#35609 = CARTESIAN_POINT ( 'NONE',  ( -10.37821464302998109, -14.49231327520767465, 71.74271303568544056 ) ) ;
#35610 = CARTESIAN_POINT ( 'NONE',  ( -10.41531639268335496, -14.04517892474411589, 60.93293405735092705 ) ) ;
#35611 = LINE ( 'NONE', #27227, #15321 ) ;
#35612 = AXIS2_PLACEMENT_3D ( 'NONE', #15874, #11706, #46173 ) ;
#35613 = ORIENTED_EDGE ( 'NONE', *, *, #22561, .F. ) ;
#35614 = CARTESIAN_POINT ( 'NONE',  ( -10.92750425249182022, -11.16255029878774252, 64.26386639478288032 ) ) ;
#35615 = B_SPLINE_CURVE_WITH_KNOTS ( 'NONE', 3,
 ( #24125, #28546, #5664, #35668, #35909, #25747, #1951, #16948, #17194, #31994 ),
 .UNSPECIFIED., .F., .F.,
 ( 4, 2, 2, 2, 4 ),
 ( 0.000000000000000000, 0.2500000000000000000, 0.5000000000000000000, 0.7500000000000000000, 1.000000000000000000 ),
 .UNSPECIFIED. ) ;
#35616 = DIRECTION ( 'NONE',  ( 0.8083598999316399247, 0.5886886037477750966, 6.671815825018553389E-08 ) ) ;
#35617 = ORIENTED_EDGE ( 'NONE', *, *, #44602, .F. ) ;
#35618 = LINE ( 'NONE', #19652, #17283 ) ;
#35619 =( BOUNDED_CURVE ( )  B_SPLINE_CURVE ( 2, ( #18287, #48337, #14569, #41935, #38715, #333, #27157, #1053, #15318 ),
 .UNSPECIFIED., .F., .F. ) 
 B_SPLINE_CURVE_WITH_KNOTS ( ( 3, 2, 2, 2, 3 ),
 ( 0.04327498545061642110, 0.04425837495377543673, 0.04524176445693445237, 0.04622515396009346106, 0.04720854346325247669 ),
 .UNSPECIFIED. ) 
 CURVE ( )  GEOMETRIC_REPRESENTATION_ITEM ( )  RATIONAL_B_SPLINE_CURVE ( ( 1.000000000000174527, 0.9238795325111123224, 1.000000000000000000, 0.9238795325112867385, 1.000000000000000000, 0.9238795325112867385, 1.000000000000000000, 0.9238795325112583168, 1.000000000000028422 ) ) 
 REPRESENTATION_ITEM ( '' )  );
#35620 = VERTEX_POINT ( 'NONE', #4898 ) ;
#35621 = CARTESIAN_POINT ( 'NONE',  ( -9.974346092350561577, -14.73447246694985147, 71.44969959282907723 ) ) ;
#35622 = CARTESIAN_POINT ( 'NONE',  ( -9.982343128696857804, -14.45766102835504263, 68.05138424084104543 ) ) ;
#35624 = EDGE_CURVE ( 'NONE', #16796, #39956, #26421, .T. ) ;
#35623 = EDGE_LOOP ( 'NONE', ( #17292, #46663 ) ) ;
#35625 = CARTESIAN_POINT ( 'NONE',  ( -10.68602809008750576, -16.88409676349039046, 57.70232650191087487 ) ) ;
#35626 = CARTESIAN_POINT ( 'NONE',  ( -21.80761086145510674, -20.26839064256230571, 58.83613193677467734 ) ) ;
#35627 = CARTESIAN_POINT ( 'NONE',  ( -36.42409385541304800, -8.109206544743658540, 50.50000000000030553 ) ) ;
#35628 = DIRECTION ( 'NONE',  ( -0.9524241471993249997, -0.3047743298226212039, -0.0009228828802129951337 ) ) ;
#35629 = ORIENTED_EDGE ( 'NONE', *, *, #4482, .F. ) ;
#35630 = CARTESIAN_POINT ( 'NONE',  ( -10.90176001668674743, -17.49323270848192635, 71.98206789237249836 ) ) ;
#35631 = DIRECTION ( 'NONE',  ( -1.000000000000000000, 0.000000000000000000, 0.000000000000000000 ) ) ;
#35632 = CARTESIAN_POINT ( 'NONE',  ( -15.17160733334415212, -8.120315110694912519, 74.23552617732688930 ) ) ;
#35633 = EDGE_LOOP ( 'NONE', ( #35344, #4912, #14771, #24828, #32820, #10634, #19327, #8914, #21528, #4249, #40043, #13523, #19301, #7152, #3857, #969, #2426, #8549, #37078, #34636, #40426, #4087, #16861, #36447, #8688, #12939 ) ) ;
#35634 = CARTESIAN_POINT ( 'NONE',  ( -17.62621216070176544, -7.758391551400871222, 67.32039556304484051 ) ) ;
#35635 = CARTESIAN_POINT ( 'NONE',  ( -50.42609385541305755, -14.80920654474422271, 68.96470588235293064 ) ) ;
#35636 = VERTEX_POINT ( 'NONE', #42801 ) ;
#35637 = VERTEX_POINT ( 'NONE', #39581 ) ;
#35638 = CARTESIAN_POINT ( 'NONE',  ( -24.45634967269333160, -15.35895078922937529, 73.00303538218732058 ) ) ;
#35639 = CARTESIAN_POINT ( 'NONE',  ( -19.96994574550859980, -21.32983827578761193, 72.40478737306770540 ) ) ;
#35640 = CARTESIAN_POINT ( 'NONE',  ( -11.35719102664687874, -18.40077844947705543, 58.09242476654641507 ) ) ;
#35641 = CARTESIAN_POINT ( 'NONE',  ( -18.30534385650551954, -8.801233750844183135, 48.81488406609782515 ) ) ;
#35642 = CARTESIAN_POINT ( 'NONE',  ( -17.23552066371262725, -19.49191114800217051, 52.02966884056656482 ) ) ;
#35643 = CARTESIAN_POINT ( 'NONE',  ( -13.08938031007640213, -9.312742571539336822, 67.66477384774475468 ) ) ;
#35644 = EDGE_CURVE ( 'NONE', #3562, #39905, #27533, .T. ) ;
#35645 = DIRECTION ( 'NONE',  ( 0.9687793358424821033, -0.2479245821708680464, 0.000000000000000000 ) ) ;
#35646 = EDGE_LOOP ( 'NONE', ( #30845, #42752, #45451, #3012 ) ) ;
#35647 = ORIENTED_EDGE ( 'NONE', *, *, #33310, .T. ) ;
#35648 = CARTESIAN_POINT ( 'NONE',  ( -10.96921284960095555, -11.97350354382807680, 74.84368195529052059 ) ) ;
#35649 = ADVANCED_FACE ( 'NONE', ( #2148 ), #7598, .T. ) ;
#35650 = EDGE_CURVE ( 'NONE', #21669, #44245, #11326, .T. ) ;
#35651 = DIRECTION ( 'NONE',  ( 0.000000000000000000, 0.000000000000000000, 1.000000000000000000 ) ) ;
#35652 = VECTOR ( 'NONE', #20977, 1000.000000000000000 ) ;
#35653 = CARTESIAN_POINT ( 'NONE',  ( -12.12786991918758339, -13.32596279628197600, 53.49899999999994549 ) ) ;
#35654 = CARTESIAN_POINT ( 'NONE',  ( -22.48114103837971101, -19.64927616005747879, 72.64400547034465205 ) ) ;
#35655 = CARTESIAN_POINT ( 'NONE',  ( -21.97169192525862869, -15.94174089086206791, 52.02966884056656482 ) ) ;
#35656 = B_SPLINE_CURVE_WITH_KNOTS ( 'NONE', 3,
 ( #15081, #45392, #16053, #571, #11647, #26924, #19778, #335, #4034, #41437 ),
 .UNSPECIFIED., .F., .F.,
 ( 4, 2, 2, 2, 4 ),
 ( 0.000000000000000000, 0.2500000000000000000, 0.5000000000000000000, 0.7500000000000000000, 1.000000000000000000 ),
 .UNSPECIFIED. ) ;
#35657 = ORIENTED_EDGE ( 'NONE', *, *, #18818, .F. ) ;
#35658 = CARTESIAN_POINT ( 'NONE',  ( -14.92764478915313653, -21.34891159457319532, 61.63600440564275829 ) ) ;
#35659 = CARTESIAN_POINT ( 'NONE',  ( -23.99713630548045273, -11.30230610301594574, 66.52876207254645635 ) ) ;
#35660 = FACE_OUTER_BOUND ( 'NONE', #36072, .T. ) ;
#35661 = CARTESIAN_POINT ( 'NONE',  ( -24.11881394502254849, -17.01995806294775448, 73.16863963025599560 ) ) ;
#35662 = ORIENTED_EDGE ( 'NONE', *, *, #33942, .T. ) ;
#35663 = DIRECTION ( 'NONE',  ( 1.000000000000000000, 2.866981220435666553E-17, 0.000000000000000000 ) ) ;
#35664 = CARTESIAN_POINT ( 'NONE',  ( -22.20390354280803180, -19.99167827517580420, 65.70981500101784434 ) ) ;
#35665 = CARTESIAN_POINT ( 'NONE',  ( -10.78978129071826686, -12.42417052737942917, 57.32857332104949677 ) ) ;
#35666 = EDGE_CURVE ( 'NONE', #42513, #42051, #36514, .T. ) ;
#35667 = CARTESIAN_POINT ( 'NONE',  ( -17.42409385541299471, -14.80920654474435594, 52.02966884056656482 ) ) ;
#35668 = CARTESIAN_POINT ( 'NONE',  ( -23.45033742471730420, -11.24757414297479663, 69.96498761153686985 ) ) ;
#35669 = ORIENTED_EDGE ( 'NONE', *, *, #44681, .T. ) ;
#35670 = CARTESIAN_POINT ( 'NONE',  ( -10.48584418858393796, -13.88064117961823563, 57.44825077271759284 ) ) ;
#35671 = ORIENTED_EDGE ( 'NONE', *, *, #26130, .F. ) ;
#35672 = DIRECTION ( 'NONE',  ( 1.224646799147353207E-16, 1.000000000000000000, -1.912410701131276611E-32 ) ) ;
#35673 = CARTESIAN_POINT ( 'NONE',  ( -21.19428927390184114, -8.848463597801222491, 73.48639860482715847 ) ) ;
#35674 = VERTEX_POINT ( 'NONE', #35151 ) ;
#35675 = LINE ( 'NONE', #42620, #35224 ) ;
#35676 = AXIS2_PLACEMENT_3D ( 'NONE', #23481, #822, #15572 ) ;
#35677 = CARTESIAN_POINT ( 'NONE',  ( -14.51159385650551492, -6.922745924619793101, 51.69366785382590024 ) ) ;
#35678 = ORIENTED_EDGE ( 'NONE', *, *, #1758, .T. ) ;
#35679 = CARTESIAN_POINT ( 'NONE',  ( -15.22116837037893866, -21.50650591823945845, 68.59065000974109694 ) ) ;
#35680 = CARTESIAN_POINT ( 'NONE',  ( -24.05845762361657947, -12.57644656616312773, 73.24225570276865938 ) ) ;
#35681 = FACE_OUTER_BOUND ( 'NONE', #12208, .T. ) ;
#35682 = EDGE_LOOP ( 'NONE', ( #1619, #32975, #45367, #42556 ) ) ;
#35683 = DIRECTION ( 'NONE',  ( -0.5351595679979683773, -0.8447509909909712844, 0.000000000000000000 ) ) ;
#35684 = CARTESIAN_POINT ( 'NONE',  ( -10.44881520703817479, -17.42631679175528703, 64.74244059074541724 ) ) ;
#35685 = FACE_OUTER_BOUND ( 'NONE', #11347, .T. ) ;
#35686 = DIRECTION ( 'NONE',  ( -2.866981220435666553E-17, 1.000000000000000000, 1.190614954331866791E-16 ) ) ;
#35687 = ORIENTED_EDGE ( 'NONE', *, *, #18647, .T. ) ;
#35688 = ORIENTED_EDGE ( 'NONE', *, *, #1712, .T. ) ;
#35689 = DIRECTION ( 'NONE',  ( -1.000000000000000000, 0.000000000000000000, 9.637352644315596475E-17 ) ) ;
#35690 = CARTESIAN_POINT ( 'NONE',  ( -21.00588228679873382, -20.88502978299158741, 69.46939052609951659 ) ) ;
#35691 = VERTEX_POINT ( 'NONE', #1421 ) ;
#35692 = CARTESIAN_POINT ( 'NONE',  ( -22.28468842640968006, -19.91619389767071269, 65.98949666203347419 ) ) ;
#35693 = CARTESIAN_POINT ( 'NONE',  ( -10.47425561207849753, -17.49314520081206936, 64.81234810402725088 ) ) ;
#35694 = CARTESIAN_POINT ( 'NONE',  ( -17.60534385759799036, -7.595227055684746986, 51.75156210489594599 ) ) ;
#35695 = CARTESIAN_POINT ( 'NONE',  ( -13.05080691482932487, -8.777874379507830227, 64.10957736189999423 ) ) ;
#35696 = DIRECTION ( 'NONE',  ( -2.866981220435666553E-17, 1.000000000000000000, 1.190614954331866791E-16 ) ) ;
#35697 = FACE_OUTER_BOUND ( 'NONE', #37882, .T. ) ;
#35698 = ORIENTED_EDGE ( 'NONE', *, *, #36572, .F. ) ;
#35699 = CARTESIAN_POINT ( 'NONE',  ( -22.94545718403308854, -10.41951498227516204, 66.84182396041623520 ) ) ;
#35700 = EDGE_CURVE ( 'NONE', #40656, #45424, #45971, .T. ) ;
#35701 = CARTESIAN_POINT ( 'NONE',  ( -19.04853579327176760, -7.948602568230340282, 63.71617106789811658 ) ) ;
#35702 = B_SPLINE_CURVE_WITH_KNOTS ( 'NONE', 3,
 ( #30111, #34017, #29859, #19013, #30596, #41174, #33771, #14789, #7703, #37712 ),
 .UNSPECIFIED., .F., .F.,
 ( 4, 2, 2, 2, 4 ),
 ( 0.6272669072877665730, 0.7522669073072862922, 0.8772669073268060114, 1.002266907346325731, 1.127266907365845450 ),
 .UNSPECIFIED. ) ;
#35703 = CARTESIAN_POINT ( 'NONE',  ( -12.83007325466668114, -20.09077588727113550, 72.10653676829758751 ) ) ;
#35704 = CARTESIAN_POINT ( 'NONE',  ( -12.63291411399994146, -9.103221862242449447, 74.50578369661835154 ) ) ;
#35705 = CARTESIAN_POINT ( 'NONE',  ( -10.82867520472564848, -11.34449427682889677, 67.73369198428547122 ) ) ;
#35706 = ORIENTED_EDGE ( 'NONE', *, *, #2306, .T. ) ;
#35707 = ORIENTED_EDGE ( 'NONE', *, *, #45664, .F. ) ;
#35708 = VECTOR ( 'NONE', #25187, 1000.000000000000000 ) ;
#35709 = EDGE_CURVE ( 'NONE', #11362, #39854, #13169, .T. ) ;
#35710 = EDGE_CURVE ( 'NONE', #28414, #15343, #46516, .T. ) ;
#35711 = ORIENTED_EDGE ( 'NONE', *, *, #15939, .F. ) ;
#35712 = CARTESIAN_POINT ( 'NONE',  ( -10.86332160119170354, -12.36740434215989737, 57.34473927219137579 ) ) ;
#35713 = AXIS2_PLACEMENT_3D ( 'NONE', #42857, #20451, #35683 ) ;
#35714 = SURFACE_STYLE_FILL_AREA ( #24663 ) ;
#35715 = EDGE_CURVE ( 'NONE', #26003, #19831, #9533, .T. ) ;
#35716 = CARTESIAN_POINT ( 'NONE',  ( -16.43987971142158599, -21.73979382505777735, 62.05568083039364780 ) ) ;
#35717 = EDGE_CURVE ( 'NONE', #43808, #19690, #43536, .T. ) ;
#35718 = ORIENTED_EDGE ( 'NONE', *, *, #41170, .F. ) ;
#35719 = CARTESIAN_POINT ( 'NONE',  ( -22.79734409636068904, -10.24514240368273477, 66.54182257473807738 ) ) ;
#35720 = CARTESIAN_POINT ( 'NONE',  ( -10.37255316239921044, -15.11044245508572459, 57.71225695896244190 ) ) ;
#35721 = EDGE_CURVE ( 'NONE', #22869, #42245, #38079, .T. ) ;
#35722 = ORIENTED_EDGE ( 'NONE', *, *, #33024, .F. ) ;
#35723 = CARTESIAN_POINT ( 'NONE',  ( -10.62531315016929767, -17.85539008243733861, 71.66694575197517736 ) ) ;
#35724 = DIRECTION ( 'NONE',  ( 2.866981220435666553E-17, -1.000000000000000000, -1.190614954331866791E-16 ) ) ;
#35725 = VERTEX_POINT ( 'NONE', #25771 ) ;
#35726 = CARTESIAN_POINT ( 'NONE',  ( -33.52409385541305653, -6.359206544744109735, 52.29999999999998295 ) ) ;
#35727 = ORIENTED_EDGE ( 'NONE', *, *, #25067, .F. ) ;
#35728 = CARTESIAN_POINT ( 'NONE',  ( -11.93522140360746064, -14.45952210441258501, 53.49999999999995026 ) ) ;
#35729 = VERTEX_POINT ( 'NONE', #44030 ) ;
#35730 = CARTESIAN_POINT ( 'NONE',  ( -16.02567528876233993, -7.491550372963335924, 63.92656979170173059 ) ) ;
#35731 = DIRECTION ( 'NONE',  ( 5.104528489711356381E-07, 5.317498756133547718E-07, 0.9999999999997283284 ) ) ;
#35732 = CARTESIAN_POINT ( 'NONE',  ( -19.23951954158338751, -22.03540154427634334, 58.71162761787055473 ) ) ;
#35733 = ORIENTED_EDGE ( 'NONE', *, *, #9269, .F. ) ;
#35734 = CARTESIAN_POINT ( 'NONE',  ( -22.58065782673598676, -12.89613362149922260, 53.49899999999994549 ) ) ;
#35735 = CARTESIAN_POINT ( 'NONE',  ( -50.42609385541305755, -14.80920654474419074, 65.94705882352940307 ) ) ;
#35736 = FACE_OUTER_BOUND ( 'NONE', #16844, .T. ) ;
#35737 =( BOUNDED_CURVE ( )  B_SPLINE_CURVE ( 3, ( #16544, #13803, #46842, #13328 ),
 .UNSPECIFIED., .F., .F. ) 
 B_SPLINE_CURVE_WITH_KNOTS ( ( 4, 4 ),
 ( 0.000000000000000000, 0.4074455897393627901 ),
 .UNSPECIFIED. ) 
 CURVE ( )  GEOMETRIC_REPRESENTATION_ITEM ( )  RATIONAL_B_SPLINE_CURVE ( ( 1.000000000000000000, 0.4567392136813325787, 0.3561768502900305444, 0.6983129098260937306 ) ) 
 REPRESENTATION_ITEM ( '' )  );
#35738 = LINE ( 'NONE', #32316, #3063 ) ;
#35739 = DIRECTION ( 'NONE',  ( 0.8705373987491421550, -0.4921022631314296847, 4.758021987246392719E-08 ) ) ;
#35740 = DIRECTION ( 'NONE',  ( -1.224646799147353207E-16, -1.000000000000000000, 1.935130192142698731E-16 ) ) ;
#35741 = ORIENTED_EDGE ( 'NONE', *, *, #12761, .T. ) ;
#35742 = FACE_OUTER_BOUND ( 'NONE', #27812, .T. ) ;
#35743 = CARTESIAN_POINT ( 'NONE',  ( -11.77745829805909850, -9.948221969229217976, 67.68552175396945358 ) ) ;
#35744 = CARTESIAN_POINT ( 'NONE',  ( -10.37541943412130863, -14.96049300415475614, 75.08306784598362071 ) ) ;
#35745 = VECTOR ( 'NONE', #27060, 1000.000000000000000 ) ;
#35746 = CARTESIAN_POINT ( 'NONE',  ( -28.42409385541305511, -6.359206544744109735, 47.99999999999997868 ) ) ;
#35747 = DIRECTION ( 'NONE',  ( 3.071710424422018668E-17, -6.404604876783312462E-16, -1.000000000000000000 ) ) ;
#35748 = CARTESIAN_POINT ( 'NONE',  ( -17.96784385650551741, -6.428312510596451368, 51.20221977374900035 ) ) ;
#35749 = CIRCLE ( 'NONE', #34987, 5.249999999999998224 ) ;
#35750 = VERTEX_POINT ( 'NONE', #36832 ) ;
#35751 = CARTESIAN_POINT ( 'NONE',  ( -13.17762867948185601, -11.72213130924974678, 50.77966884056655772 ) ) ;
#35752 = FACE_OUTER_BOUND ( 'NONE', #44789, .T. ) ;
#35753 = ORIENTED_EDGE ( 'NONE', *, *, #23650, .F. ) ;
#35754 = CARTESIAN_POINT ( 'NONE',  ( -11.67943375510494697, -18.89645239624664441, 68.50217487844219022 ) ) ;
#35755 = DIRECTION ( 'NONE',  ( 3.549360974554993999E-17, -6.371834667797928663E-18, -1.000000000000000000 ) ) ;
#35756 = CARTESIAN_POINT ( 'NONE',  ( -23.07906255732286738, -9.958937815627702861, 66.72677557046061736 ) ) ;
#35757 = CARTESIAN_POINT ( 'NONE',  ( -22.80481760130283675, -10.24931098477615166, 70.42667203218238114 ) ) ;
#35758 = CARTESIAN_POINT ( 'NONE',  ( 6.575906144586949331, -6.859212275519752211, 50.50378509014259265 ) ) ;
#35759 = EDGE_CURVE ( 'NONE', #3842, #34970, #28671, .T. ) ;
#35760 = VERTEX_POINT ( 'NONE', #40790 ) ;
#35761 = CARTESIAN_POINT ( 'NONE',  ( -24.80650529658183956, -15.81082447850069883, 69.63969160935214120 ) ) ;
#35762 =( BOUNDED_CURVE ( )  B_SPLINE_CURVE ( 3, ( #46787, #1732, #38904, #5183 ),
 .UNSPECIFIED., .F., .F. ) 
 B_SPLINE_CURVE_WITH_KNOTS ( ( 4, 4 ),
 ( 0.9074455897393619574, 1.000000000000000000 ),
 .UNSPECIFIED. ) 
 CURVE ( )  GEOMETRIC_REPRESENTATION_ITEM ( )  RATIONAL_B_SPLINE_CURVE ( ( 0.6983129098260971723, 0.7760317562607017550, 0.8765941196520027345, 1.000000000000000000 ) ) 
 REPRESENTATION_ITEM ( '' )  );
#35763 = DIRECTION ( 'NONE',  ( 3.549360974554993999E-17, -6.371834667797928663E-18, -1.000000000000000000 ) ) ;
#35764 = B_SPLINE_CURVE_WITH_KNOTS ( 'NONE', 3,
 ( #34655, #43016, #31207, #9054, #4624, #24072, #31695, #16417, #19649, #27512 ),
 .UNSPECIFIED., .F., .F.,
 ( 4, 2, 2, 2, 4 ),
 ( 0.000000000000000000, 0.2500000000000000000, 0.5000000000000000000, 0.7500000000000000000, 1.000000000000000000 ),
 .UNSPECIFIED. ) ;
#35765 = PLANE ( 'NONE',  #25147 ) ;
#35766 = EDGE_CURVE ( 'NONE', #1460, #31052, #19207, .T. ) ;
#35767 = ORIENTED_EDGE ( 'NONE', *, *, #19032, .F. ) ;
#35768 = DIRECTION ( 'NONE',  ( 2.866981220435666553E-17, -1.000000000000000000, -1.190614954331866791E-16 ) ) ;
#35769 = CARTESIAN_POINT ( 'NONE',  ( -15.74783386771837890, -7.961078896070159061, 70.62461975990308360 ) ) ;
#35770 = B_SPLINE_CURVE_WITH_KNOTS ( 'NONE', 1,
 ( #10498, #7047 ),
 .UNSPECIFIED., .F., .F.,
 ( 2, 2 ),
 ( 0.000000000000000000, 1.000000000000000000 ),
 .UNSPECIFIED. ) ;
#35771 = LINE ( 'NONE', #43433, #42900 ) ;
#35772 = CARTESIAN_POINT ( 'NONE',  ( -24.59748878097435210, -12.79772186451832994, 66.34600794915635902 ) ) ;
#35773 = CARTESIAN_POINT ( 'NONE',  ( -10.42334091404133645, -15.64104667191196185, 61.33789045260130024 ) ) ;
#35774 = CARTESIAN_POINT ( 'NONE',  ( -6.424093855413055110, -25.10920654474410441, 47.99999999999998579 ) ) ;
#35775 = ORIENTED_EDGE ( 'NONE', *, *, #29177, .T. ) ;
#35776 = VERTEX_POINT ( 'NONE', #21370 ) ;
#35777 = CARTESIAN_POINT ( 'NONE',  ( -19.82409385541304303, -9.359200813967568422, 50.49621490985803263 ) ) ;
#35778 = CARTESIAN_POINT ( 'NONE',  ( -10.66160677810301038, -13.00123309306513697, 67.73832347541063825 ) ) ;
#35779 = EDGE_CURVE ( 'NONE', #5540, #19035, #27718, .T. ) ;
#35780 = B_SPLINE_CURVE_WITH_KNOTS ( 'NONE', 1,
 ( #31823, #43890 ),
 .UNSPECIFIED., .F., .F.,
 ( 2, 2 ),
 ( 0.000000000000000000, 1.000000000000000000 ),
 .UNSPECIFIED. ) ;
#35781 = CARTESIAN_POINT ( 'NONE',  ( -15.56465948913147557, -7.543361525925788236, 53.49999999999994316 ) ) ;
#35782 = ADVANCED_FACE ( 'NONE', ( #32901 ), #22991, .T. ) ;
#35783 = AXIS2_PLACEMENT_3D ( 'NONE', #536, #15528, #26895 ) ;
#35784 = EDGE_CURVE ( 'NONE', #8895, #6650, #13464, .T. ) ;
#35785 = DIRECTION ( 'NONE',  ( -3.071710424422018668E-17, 6.404604876783312462E-16, 1.000000000000000000 ) ) ;
#35786 = CARTESIAN_POINT ( 'NONE',  ( -17.42409385541305511, -14.80920654474410725, 48.99999999999997868 ) ) ;
#35787 = AXIS2_PLACEMENT_3D ( 'NONE', #46185, #42974, #12442 ) ;
#35788 = ORIENTED_EDGE ( 'NONE', *, *, #40411, .T. ) ;
#35789 = CARTESIAN_POINT ( 'NONE',  ( -10.99586697244644640, -11.04334986774487781, 60.86381167495338929 ) ) ;
#35790 = CARTESIAN_POINT ( 'NONE',  ( -24.44334717380189659, -17.30795561478116085, 69.52684539094292404 ) ) ;
#35791 = EDGE_CURVE ( 'NONE', #17461, #31125, #31452, .T. ) ;
#35792 = ORIENTED_EDGE ( 'NONE', *, *, #47526, .F. ) ;
#35793 = DIRECTION ( 'NONE',  ( -0.1240347345892086200, 1.145860353393066553E-16, -0.9922778767136676281 ) ) ;
#35794 = CARTESIAN_POINT ( 'NONE',  ( -17.04628566472521811, -7.819299315193825706, 73.96018289602247364 ) ) ;
#35795 = ORIENTED_EDGE ( 'NONE', *, *, #40165, .T. ) ;
#35796 = CARTESIAN_POINT ( 'NONE',  ( -10.43949455435184603, -13.84896052950683476, 57.46297163929641982 ) ) ;
#35797 = CARTESIAN_POINT ( 'NONE',  ( -11.30759946633453339, -18.32231678669580077, 61.36891081969880446 ) ) ;
#35798 = ORIENTED_EDGE ( 'NONE', *, *, #15106, .T. ) ;
#35799 = CARTESIAN_POINT ( 'NONE',  ( -17.79108452803360763, -21.84994637594637723, 58.69081321602850920 ) ) ;
#35800 = CARTESIAN_POINT ( 'NONE',  ( -10.00891317999088592, -15.53039051438984863, 57.72826173703180075 ) ) ;
#35801 = CARTESIAN_POINT ( 'NONE',  ( -20.51116909090755769, -10.56274136881318526, 49.52966884056655772 ) ) ;
#35802 = CARTESIAN_POINT ( 'NONE',  ( -11.08752838525962048, -17.78389909896315402, 71.79391619061119911 ) ) ;
#35803 = ORIENTED_EDGE ( 'NONE', *, *, #7655, .F. ) ;
#35804 = CARTESIAN_POINT ( 'NONE',  ( -22.11801181964649388, -9.023811091936513762, 63.44799684341401047 ) ) ;
#35805 = CARTESIAN_POINT ( 'NONE',  ( -10.75331649400429868, -16.93069871048427544, 57.68760548944693056 ) ) ;
#35806 = FACE_OUTER_BOUND ( 'NONE', #2201, .T. ) ;
#35807 = DIRECTION ( 'NONE',  ( 0.8394943004421986377, -0.3114503813636534946, -0.4452504682462426477 ) ) ;
#35808 = FACE_OUTER_BOUND ( 'NONE', #35137, .T. ) ;
#35809 = CARTESIAN_POINT ( 'NONE',  ( -11.46947365556686371, -11.12676018782347320, 60.75056137761610842 ) ) ;
#35810 = CARTESIAN_POINT ( 'NONE',  ( -10.00439786467154057, -15.48048233825869424, 57.71792808022589583 ) ) ;
#35811 = CARTESIAN_POINT ( 'NONE',  ( -12.16327279079253820, -10.11041878036023967, 67.79896963893753536 ) ) ;
#35812 = ORIENTED_EDGE ( 'NONE', *, *, #45538, .F. ) ;
#35813 = CARTESIAN_POINT ( 'NONE',  ( -13.85393650630732054, -8.270265118416840977, 74.38450092284953996 ) ) ;
#35814 = CARTESIAN_POINT ( 'NONE',  ( -13.60167271156757707, -11.21037387301822008, 52.02966884056656482 ) ) ;
#35815 = CARTESIAN_POINT ( 'NONE',  ( -13.38108913796246746, -20.52371920327048826, 58.04650125921649817 ) ) ;
#35816 = EDGE_CURVE ( 'NONE', #47755, #19754, #20124, .T. ) ;
#35817 = VERTEX_POINT ( 'NONE', #46382 ) ;
#35818 = LINE ( 'NONE', #25244, #44389 ) ;
#35819 = AXIS2_PLACEMENT_3D ( 'NONE', #44892, #40215, #44174 ) ;
#35820 = VERTEX_POINT ( 'NONE', #42198 ) ;
#35821 = ORIENTED_EDGE ( 'NONE', *, *, #16746, .T. ) ;
#35822 = VERTEX_POINT ( 'NONE', #31352 ) ;
#35823 = DIRECTION ( 'NONE',  ( 0.2189141945955467017, -0.9757441136919982050, 0.000000000000000000 ) ) ;
#35824 = CARTESIAN_POINT ( 'NONE',  ( -12.90354087724769272, -8.887350501024684490, 67.49447389996370816 ) ) ;
#35825 = FACE_OUTER_BOUND ( 'NONE', #17606, .T. ) ;
#35826 = CARTESIAN_POINT ( 'NONE',  ( -40.92409385541305511, -14.80920654474410725, 74.99999999999998579 ) ) ;
#35827 = DIRECTION ( 'NONE',  ( 2.866981220435666553E-17, -1.000000000000000000, -1.190614954331866791E-16 ) ) ;
#35828 = ORIENTED_EDGE ( 'NONE', *, *, #12608, .F. ) ;
#35829 = ORIENTED_EDGE ( 'NONE', *, *, #37047, .F. ) ;
#35830 = CARTESIAN_POINT ( 'NONE',  ( -20.13659385650551670, -6.915538690918075382, 49.31353937987644542 ) ) ;
#35831 = EDGE_CURVE ( 'NONE', #35760, #46816, #24789, .T. ) ;
#35832 = CARTESIAN_POINT ( 'NONE',  ( -21.00380416015782004, -21.34292312329482399, 62.22976100777699315 ) ) ;
#35833 = FACE_OUTER_BOUND ( 'NONE', #8586, .T. ) ;
#35834 = ADVANCED_FACE ( 'NONE', ( #29966 ), #16336, .T. ) ;
#35835 = CARTESIAN_POINT ( 'NONE',  ( -22.66784385650551670, -6.428312510596451368, 51.20221977374900035 ) ) ;
#35836 = VERTEX_POINT ( 'NONE', #5022 ) ;
#35837 = ADVANCED_FACE ( 'NONE', ( #11004 ), #8461, .T. ) ;
#35838 = CARTESIAN_POINT ( 'NONE',  ( -24.72409385541305582, -14.90920654474416907, 63.93529411764704662 ) ) ;
#35839 = CARTESIAN_POINT ( 'NONE',  ( -10.85841931818429629, -17.37798394237198707, 64.91267318220633342 ) ) ;
#35840 = DIRECTION ( 'NONE',  ( -2.866981220435666553E-17, 1.000000000000000000, 1.190614954331866791E-16 ) ) ;
#35841 = EDGE_CURVE ( 'NONE', #22864, #6140, #36462, .T. ) ;
#35842 = EDGE_LOOP ( 'NONE', ( #36820, #44403, #15678, #48437 ) ) ;
#35843 = CARTESIAN_POINT ( 'NONE',  ( -11.66088694488815314, -18.78249085348093672, 68.51689682890159361 ) ) ;
#35844 = CIRCLE ( 'NONE', #35081, 2.000000000000003109 ) ;
#35845 = CARTESIAN_POINT ( 'NONE',  ( -10.65515204393805959, -12.82555568974835580, 61.00673515780317757 ) ) ;
#35846 = CARTESIAN_POINT ( 'NONE',  ( -11.25385002771267473, -18.98553936430136702, 68.40345028533118921 ) ) ;
#35847 = DIRECTION ( 'NONE',  ( 0.9687793358424817702, -0.2479245821708684350, 0.000000000000000000 ) ) ;
#35848 = VERTEX_POINT ( 'NONE', #27413 ) ;
#35849 = DIRECTION ( 'NONE',  ( 0.9942595023566571655, -0.1069955231469582047, 3.800058679842194246E-08 ) ) ;
#35850 = EDGE_CURVE ( 'NONE', #24736, #38529, #29433, .T. ) ;
#35851 = CARTESIAN_POINT ( 'NONE',  ( -11.73296596577226936, -10.64774513788296417, 74.72412863062541533 ) ) ;
#35852 = DIRECTION ( 'NONE',  ( 0.6043825497304157190, -0.7966942535134532433, 5.656674838975381179E-08 ) ) ;
#35853 = ORIENTED_EDGE ( 'NONE', *, *, #37854, .F. ) ;
#35854 = CYLINDRICAL_SURFACE ( 'NONE', #18079, 1.999999999999999112 ) ;
#35855 = EDGE_CURVE ( 'NONE', #5832, #18426, #23745, .T. ) ;
#35856 = VERTEX_POINT ( 'NONE', #33376 ) ;
#35857 = LINE ( 'NONE', #17136, #42339 ) ;
#35858 = CARTESIAN_POINT ( 'NONE',  ( -14.65075332640449091, -7.894636944940137901, 60.42022027453841559 ) ) ;
#35859 = ORIENTED_EDGE ( 'NONE', *, *, #2974, .F. ) ;
#35860 = CARTESIAN_POINT ( 'NONE',  ( -10.42546210075913748, -12.25520342886974845, 57.44361899967025664 ) ) ;
#35861 = FACE_OUTER_BOUND ( 'NONE', #45247, .T. ) ;
#35862 = CARTESIAN_POINT ( 'NONE',  ( -17.01436944207222624, -7.370403393205478437, 74.21664194825545735 ) ) ;
#35863 = B_SPLINE_CURVE_WITH_KNOTS ( 'NONE', 3,
 ( #39619, #22059, #28045, #1948, #43071, #31992, #47005, #11705, #8040, #14878 ),
 .UNSPECIFIED., .F., .F.,
 ( 4, 2, 2, 2, 4 ),
 ( 0.000000000000000000, 0.2500000000000000000, 0.5000000000000000000, 0.7500000000000000000, 1.000000000000000000 ),
 .UNSPECIFIED. ) ;
#35864 = CYLINDRICAL_SURFACE ( 'NONE', #25881, 1.049999999999998934 ) ;
#35865 = ORIENTED_EDGE ( 'NONE', *, *, #270, .F. ) ;
#35866 = CARTESIAN_POINT ( 'NONE',  ( -17.00410623003636346, -7.771727578618798482, 74.11018273220987851 ) ) ;
#35867 = DIRECTION ( 'NONE',  ( -0.1240347345892086200, 1.145860353393066553E-16, -0.9922778767136676281 ) ) ;
#35868 = CARTESIAN_POINT ( 'NONE',  ( -10.09291371782238045, -16.13494220690481384, 68.16263107114907882 ) ) ;
#35869 = ORIENTED_EDGE ( 'NONE', *, *, #33585, .T. ) ;
#35870 = DIRECTION ( 'NONE',  ( 0.000000000000000000, 1.000000000000000000, -0.000000000000000000 ) ) ;
#35871 = CARTESIAN_POINT ( 'NONE',  ( -24.19028598586675116, -12.80082241304059210, 62.98831023884616798 ) ) ;
#35872 = VERTEX_POINT ( 'NONE', #48419 ) ;
#35873 = ORIENTED_EDGE ( 'NONE', *, *, #11049, .T. ) ;
#35874 = CARTESIAN_POINT ( 'NONE',  ( -20.46655431664719060, -21.17292242669622837, 58.73655241890688927 ) ) ;
#35875 = DIRECTION ( 'NONE',  ( 0.8324837747691379297, 0.5540494244615070674, 4.550593720660606642E-17 ) ) ;
#35876 = CARTESIAN_POINT ( 'NONE',  ( -20.46316679850361808, -18.39244407412632043, 49.52966884056656482 ) ) ;
#35877 = CARTESIAN_POINT ( 'NONE',  ( -18.69909385650551670, -8.114302828567740988, 52.18300498402516041 ) ) ;
#35878 = CARTESIAN_POINT ( 'NONE',  ( -18.77178190320302775, -7.889067033164298692, 70.37627854585417708 ) ) ;
#35879 = CARTESIAN_POINT ( 'NONE',  ( -19.54417908753315558, -21.48049550124873619, 62.22176935888264637 ) ) ;
#35880 =( BOUNDED_SURFACE ( )  B_SPLINE_SURFACE ( 3, 1, ( 
 ( #198, #27010 ),
 ( #26042, #30481 ),
 ( #37339, #45496 ),
 ( #3626, #33641 ),
 ( #48682, #14926 ),
 ( #29983, #41295 ),
 ( #7581, #3885 ) ),
 .UNSPECIFIED., .T., .F., .F. ) 
 B_SPLINE_SURFACE_WITH_KNOTS ( ( 4, 3, 4 ),
 ( 2, 2 ),
 ( 0.000000000000000000, 0.5000000000000000000, 1.000000000000000000 ),
 ( 0.000000000000000000, 1.000000000000000000 ),
 .UNSPECIFIED. ) 
 GEOMETRIC_REPRESENTATION_ITEM ( )  RATIONAL_B_SPLINE_SURFACE ( (
 ( 1.000000000000000000, 1.000000000000000000),
 ( 0.3333333333333335369, 0.3333333333333330373),
 ( 0.3333333333333335369, 0.3333333333333330373),
 ( 1.000000000000000000, 1.000000000000000000),
 ( 0.3333333333333333703, 0.3333333333333333703),
 ( 0.3333333333333333703, 0.3333333333333333703),
 ( 1.000000000000000000, 1.000000000000000000) ) ) 
 REPRESENTATION_ITEM ( '' )  SURFACE ( )  );
#35881 = CARTESIAN_POINT ( 'NONE',  ( -12.32124988467013615, -19.60105808195379140, 58.21217042357060478 ) ) ;
#35882 = DIRECTION ( 'NONE',  ( -0.7670373483544791204, -0.6416024518573234525, 2.496223344567222868E-08 ) ) ;
#35883 = CARTESIAN_POINT ( 'NONE',  ( -43.14308517176575464, -27.10920654474410796, 57.24806946917839667 ) ) ;
#35884 = VECTOR ( 'NONE', #7897, 1000.000000000000000 ) ;
#35885 = VECTOR ( 'NONE', #15920, 1000.000000000000000 ) ;
#35886 = ORIENTED_EDGE ( 'NONE', *, *, #21141, .F. ) ;
#35887 = ORIENTED_EDGE ( 'NONE', *, *, #14611, .F. ) ;
#35888 = LINE ( 'NONE', #35653, #1587 ) ;
#35889 = FACE_OUTER_BOUND ( 'NONE', #8804, .T. ) ;
#35890 = CARTESIAN_POINT ( 'NONE',  ( -13.88419686192642111, -8.703135698866935499, 57.11400917758039952 ) ) ;
#35891 = DIRECTION ( 'NONE',  ( -1.000000000000000000, 2.276824562219560297E-16, 0.000000000000000000 ) ) ;
#35892 = CARTESIAN_POINT ( 'NONE',  ( -22.91784385650551670, -9.790100578890868377, 49.79778022625162492 ) ) ;
#35893 =( BOUNDED_CURVE ( )  B_SPLINE_CURVE ( 3, ( #21969, #22457, #3002, #36965 ),
 .UNSPECIFIED., .F., .F. ) 
 B_SPLINE_CURVE_WITH_KNOTS ( ( 4, 4 ),
 ( 0.5000000000000000000, 0.9074455897393716164 ),
 .UNSPECIFIED. ) 
 CURVE ( )  GEOMETRIC_REPRESENTATION_ITEM ( )  RATIONAL_B_SPLINE_CURVE ( ( 1.000000000000037081, 0.4567392136813289705, 0.3561768502900032329, 0.6983129098260999479 ) ) 
 REPRESENTATION_ITEM ( '' )  );
#35894 = ORIENTED_EDGE ( 'NONE', *, *, #37987, .F. ) ;
#35895 = ADVANCED_FACE ( 'NONE', ( #7326 ), #21400, .T. ) ;
#35896 = CARTESIAN_POINT ( 'NONE',  ( -20.03518388220226143, -21.78744935781895009, 72.59133997248245862 ) ) ;
#35897 = CARTESIAN_POINT ( 'NONE',  ( -19.92776479198160189, -21.39998277484045275, 72.41950795000725805 ) ) ;
#35898 = EDGE_CURVE ( 'NONE', #18094, #43051, #34610, .T. ) ;
#35899 = CARTESIAN_POINT ( 'NONE',  ( -17.42409385541299471, -14.80920654474435594, 52.02966884056656482 ) ) ;
#35900 = CARTESIAN_POINT ( 'NONE',  ( -18.18535082455230523, -22.22026082442155115, 65.45193850245834710 ) ) ;
#35901 = ORIENTED_EDGE ( 'NONE', *, *, #15990, .T. ) ;
#35902 = CARTESIAN_POINT ( 'NONE',  ( -10.13608973233657196, -13.26381535464663131, 74.87155958832882163 ) ) ;
#35903 =( BOUNDED_CURVE ( )  B_SPLINE_CURVE ( 2, ( #36557, #36089, #39796, #25742, #25502, #2370, #14383, #44472, #6557 ),
 .UNSPECIFIED., .F., .F. ) 
 B_SPLINE_CURVE_WITH_KNOTS ( ( 3, 2, 2, 2, 3 ),
 ( 0.03147235863061165206, 0.03245579865619469678, 0.03343923868177773456, 0.03442267870736077234, 0.03540611873294381706 ),
 .UNSPECIFIED. ) 
 CURVE ( )  GEOMETRIC_REPRESENTATION_ITEM ( )  RATIONAL_B_SPLINE_CURVE ( ( 1.000000000000000888, 0.9238795325112859613, 1.000000000000000000, 0.9238795325112867385, 1.000000000000000000, 0.9238795325112867385, 1.000000000000000000, 0.9238795325112112433, 1.000000000000075495 ) ) 
 REPRESENTATION_ITEM ( '' )  );
#35904 = CARTESIAN_POINT ( 'NONE',  ( -13.76849323099554567, -20.83774554052356365, 65.27156739751333703 ) ) ;
#35905 = CARTESIAN_POINT ( 'NONE',  ( -12.81585776823299483, -9.539872998625803291, 74.31922966058063196 ) ) ;
#35906 = SURFACE_STYLE_FILL_AREA ( #16946 ) ;
#35907 = CARTESIAN_POINT ( 'NONE',  ( -18.97054302448013985, -7.521389842619064403, 67.08567168106696954 ) ) ;
#35908 = B_SPLINE_CURVE_WITH_KNOTS ( 'NONE', 1,
 ( #9019, #31413 ),
 .UNSPECIFIED., .F., .F.,
 ( 2, 2 ),
 ( 0.000000000000000000, 1.000000000000000000 ),
 .UNSPECIFIED. ) ;
#35909 = CARTESIAN_POINT ( 'NONE',  ( -23.44282052155508111, -11.23500321550520731, 70.00096727704672617 ) ) ;
#35910 = EDGE_CURVE ( 'NONE', #36791, #45046, #35527, .T. ) ;
#35911 = CARTESIAN_POINT ( 'NONE',  ( -20.92516765556211666, -8.685814626085017309, 59.93305413929914494 ) ) ;
#35912 = ORIENTED_EDGE ( 'NONE', *, *, #13950, .F. ) ;
#35913 = CARTESIAN_POINT ( 'NONE',  ( -17.63665770386090514, -10.11555421891856099, 49.52966884056655772 ) ) ;
#35914 = EDGE_CURVE ( 'NONE', #43983, #35477, #8921, .T. ) ;
#35915 = AXIS2_PLACEMENT_3D ( 'NONE', #44096, #40599, #10349 ) ;
#35916 = ORIENTED_EDGE ( 'NONE', *, *, #19149, .F. ) ;
#35917 = CARTESIAN_POINT ( 'NONE',  ( -11.68335550665270794, -18.81469308649876737, 68.21689631955439381 ) ) ;
#35918 = CARTESIAN_POINT ( 'NONE',  ( -10.22391373207313237, -12.89608419319863053, 67.93821120038428774 ) ) ;
#35919 = ORIENTED_EDGE ( 'NONE', *, *, #1037, .T. ) ;
#35920 = EDGE_CURVE ( 'NONE', #45327, #28927, #3055, .T. ) ;
#35921 = EDGE_CURVE ( 'NONE', #31348, #12784, #15342, .T. ) ;
#35922 = ADVANCED_FACE ( 'NONE', ( #9689 ), #26137, .T. ) ;
#35923 = CARTESIAN_POINT ( 'NONE',  ( -13.44284385650551705, -8.811426318492348031, 52.18089403414752070 ) ) ;
#35924 = ORIENTED_EDGE ( 'NONE', *, *, #34889, .T. ) ;
#35925 = CARTESIAN_POINT ( 'NONE',  ( -15.19548991633585011, -21.91815178685365595, 68.76088227238139439 ) ) ;
#35926 = CIRCLE ( 'NONE', #19450, 2.000000000000001776 ) ;
#35927 = CARTESIAN_POINT ( 'NONE',  ( -24.72409385541305582, -14.80920654474418896, 65.94705882352940307 ) ) ;
#35928 = B_SPLINE_CURVE_WITH_KNOTS ( 'NONE', 1,
 ( #38353, #41586 ),
 .UNSPECIFIED., .F., .F.,
 ( 2, 2 ),
 ( 0.000000000000000000, 1.000000000000000000 ),
 .UNSPECIFIED. ) ;
#35929 = FACE_OUTER_BOUND ( 'NONE', #43984, .T. ) ;
#35930 = ORIENTED_EDGE ( 'NONE', *, *, #8484, .T. ) ;
#35931 = CARTESIAN_POINT ( 'NONE',  ( -27.42409385541305511, -25.10920654474410441, 45.99999999999998579 ) ) ;
#35932 = CARTESIAN_POINT ( 'NONE',  ( -11.73296596577226936, -10.64774513788296240, 74.72412863062541533 ) ) ;
#35933 = CARTESIAN_POINT ( 'NONE',  ( -18.30727046116018286, -21.75326869042403288, 69.11514702556002021 ) ) ;
#35934 = CYLINDRICAL_SURFACE ( 'NONE', #31093, 1.999999999999999556 ) ;
#35935 = ORIENTED_EDGE ( 'NONE', *, *, #42902, .T. ) ;
#35936 = ORIENTED_EDGE ( 'NONE', *, *, #201, .T. ) ;
#35937 = CARTESIAN_POINT ( 'NONE',  ( -23.81420843745974381, -18.63945674058080826, 72.94085094053922091 ) ) ;
#35938 = CARTESIAN_POINT ( 'NONE',  ( -21.36284888653444725, -21.13297021396988384, 69.16954901539321554 ) ) ;
#35939 = ORIENTED_EDGE ( 'NONE', *, *, #44042, .F. ) ;
#35940 = CARTESIAN_POINT ( 'NONE',  ( -10.63483715323753565, -17.87674169505483235, 71.75213630217804450 ) ) ;
#35941 = CARTESIAN_POINT ( 'NONE',  ( -10.68008709410406354, -12.75422072778657601, 64.27395902318073695 ) ) ;
#35942 = CARTESIAN_POINT ( 'NONE',  ( -17.04284385759799036, -7.587656875400192291, 49.25157356644813689 ) ) ;
#35943 = CARTESIAN_POINT ( 'NONE',  ( -36.42409385541304800, -6.859212275519750435, 50.50378509014258555 ) ) ;
#35944 = DIRECTION ( 'NONE',  ( 1.000000000000000000, 0.000000000000000000, 0.000000000000000000 ) ) ;
#35945 = CARTESIAN_POINT ( 'NONE',  ( -15.62100938680255524, -7.580606089661849012, 70.72494556531428600 ) ) ;
#35946 = VERTEX_POINT ( 'NONE', #47104 ) ;
#35947 = DIRECTION ( 'NONE',  ( -0.8017593358536256876, -0.5976470257363775129, 1.209213344977627448E-07 ) ) ;
#35948 = ADVANCED_FACE ( 'NONE', ( #24705 ), #5975, .T. ) ;
#35949 = CARTESIAN_POINT ( 'NONE',  ( -19.17247957453286844, -7.567181637230756763, 63.61584517348745038 ) ) ;
#35950 = DIRECTION ( 'NONE',  ( -3.071710424422018668E-17, 6.404604876783312462E-16, 1.000000000000000000 ) ) ;
#35951 = CARTESIAN_POINT ( 'NONE',  ( -10.82516083999262690, -11.35126292582506302, 67.72590458424124904 ) ) ;
#35952 = CIRCLE ( 'NONE', #28092, 4.686499999999998778 ) ;
#35953 = ORIENTED_EDGE ( 'NONE', *, *, #47687, .F. ) ;
#35954 = AXIS2_PLACEMENT_3D ( 'NONE', #13502, #36391, #21158 ) ;
#35955 = ORIENTED_EDGE ( 'NONE', *, *, #29318, .F. ) ;
#35956 = CARTESIAN_POINT ( 'NONE',  ( -12.56172001024846452, -20.45377019276184427, 71.99149100736865137 ) ) ;
#35957 = CARTESIAN_POINT ( 'NONE',  ( -14.08076552632586420, -21.02024474708484192, 68.45624882270347200 ) ) ;
#35958 = ADVANCED_FACE ( 'NONE', ( #9919 ), #11129, .T. ) ;
#35959 = CARTESIAN_POINT ( 'NONE',  ( -10.71125836907356543, -12.65457585138356400, 61.09293791546713948 ) ) ;
#35960 = AXIS2_PLACEMENT_3D ( 'NONE', #21470, #9671, #14281 ) ;
#35961 = EDGE_LOOP ( 'NONE', ( #26796, #433 ) ) ;
#35962 = DIRECTION ( 'NONE',  ( 1.224646799147353207E-16, 1.000000000000000000, -1.912410701131276611E-32 ) ) ;
#35963 = CARTESIAN_POINT ( 'NONE',  ( -18.34288178775629419, -10.21365315202000268, 52.02966884056656482 ) ) ;
#35964 = VERTEX_POINT ( 'NONE', #15037 ) ;
#35965 = CARTESIAN_POINT ( 'NONE',  ( -10.60881404221464663, -17.81840116198948820, 71.67444023447058044 ) ) ;
#35966 = CARTESIAN_POINT ( 'NONE',  ( -19.76711226259482856, -21.88123280879678134, 65.65760363486209883 ) ) ;
#35967 = VERTEX_POINT ( 'NONE', #18495 ) ;
#35968 = CARTESIAN_POINT ( 'NONE',  ( -23.04402284766838349, -19.06632961612601918, 59.16938527523783620 ) ) ;
#35969 = EDGE_LOOP ( 'NONE', ( #33053, #40154 ) ) ;
#35970 = CARTESIAN_POINT ( 'NONE',  ( -10.61357140615669792, -13.19155887971477448, 71.50828586566468914 ) ) ;
#35971 = VERTEX_POINT ( 'NONE', #40663 ) ;
#35972 = CARTESIAN_POINT ( 'NONE',  ( -20.35208293893518672, -8.450992964911224092, 67.08104082230126153 ) ) ;
#35973 = CARTESIAN_POINT ( 'NONE',  ( -22.83095763869631512, -19.93459457198476770, 72.82895875648904394 ) ) ;
#35974 = CARTESIAN_POINT ( 'NONE',  ( -20.89788161767221197, -20.94431024770144489, 62.39999296070408974 ) ) ;
#35975 = ORIENTED_EDGE ( 'NONE', *, *, #12330, .F. ) ;
#35976 = CARTESIAN_POINT ( 'NONE',  ( -13.41271538705132116, -9.007285817396986971, 57.17787480142766299 ) ) ;
#35977 = EDGE_CURVE ( 'NONE', #25499, #9944, #29577, .T. ) ;
#35978 = EDGE_CURVE ( 'NONE', #30260, #7661, #14301, .T. ) ;
#35979 = CARTESIAN_POINT ( 'NONE',  ( -24.04021708909630206, -12.36549076622675791, 73.12736853451067986 ) ) ;
#35980 = CYLINDRICAL_SURFACE ( 'NONE', #3747, 0.1499999999999994948 ) ;
#35981 = VECTOR ( 'NONE', #17264, 1000.000000000000227 ) ;
#35982 = CARTESIAN_POINT ( 'NONE',  ( -13.75553675855627134, -8.845634611387561463, 57.15894934091076607 ) ) ;
#35983 = CARTESIAN_POINT ( 'NONE',  ( -13.49145512112739276, -18.65424914341562967, 53.49999999999995026 ) ) ;
#35984 = CARTESIAN_POINT ( 'NONE',  ( -19.24944996930525676, -8.051263618916641107, 60.26092964427753884 ) ) ;
#35985 = EDGE_LOOP ( 'NONE', ( #43486, #38550, #18023, #17783, #42552 ) ) ;
#35986 = DIRECTION ( 'NONE',  ( 0.9524241471993248886, -0.3047743298226213149, -0.0009228828802126874372 ) ) ;
#35987 = AXIS2_PLACEMENT_3D ( 'NONE', #48062, #22209, #36701 ) ;
#35988 = VECTOR ( 'NONE', #18101, 1000.000000000000000 ) ;
#35989 = CARTESIAN_POINT ( 'NONE',  ( -16.78411497196904278, -21.83009869597352903, 68.69560651670111895 ) ) ;
#35990 = FACE_OUTER_BOUND ( 'NONE', #18912, .T. ) ;
#35991 = EDGE_CURVE ( 'NONE', #5827, #40125, #47117, .T. ) ;
#35992 = EDGE_CURVE ( 'NONE', #45391, #43613, #14198, .T. ) ;
#35993 = CARTESIAN_POINT ( 'NONE',  ( -13.13238435621759237, -20.89891265215350913, 58.15375942484206462 ) ) ;
#35994 = CARTESIAN_POINT ( 'NONE',  ( -17.88659385759798681, -7.222650657624104298, 49.61879703869476543 ) ) ;
#35995 = ORIENTED_EDGE ( 'NONE', *, *, #10613, .F. ) ;
#35996 = CARTESIAN_POINT ( 'NONE',  ( -21.24554520941113367, -21.20453976546471608, 65.76949229983627276 ) ) ;
#35997 = DIRECTION ( 'NONE',  ( -2.027460363947684990E-06, -1.195255637520530846E-05, 0.9999999999265128947 ) ) ;
#35998 = ORIENTED_EDGE ( 'NONE', *, *, #29252, .F. ) ;
#35999 = LINE ( 'NONE', #47587, #31565 ) ;
#36000 = CARTESIAN_POINT ( 'NONE',  ( -43.17409385541305511, -25.10920654474410441, 56.99999999999999289 ) ) ;
#36001 = CARTESIAN_POINT ( 'NONE',  ( -14.62687819956926027, -8.392386103536567887, 64.08978840643771946 ) ) ;
#36002 = AXIS2_PLACEMENT_3D ( 'NONE', #3474, #29837, #41152 ) ;
#36003 = CARTESIAN_POINT ( 'NONE',  ( -12.10131192688100477, -10.18592936015514638, 64.31442259820508411 ) ) ;
#36004 = DIRECTION ( 'NONE',  ( 1.927470528863119542E-16, 0.000000000000000000, -1.000000000000000000 ) ) ;
#36005 = ORIENTED_EDGE ( 'NONE', *, *, #15666, .F. ) ;
#36006 = CARTESIAN_POINT ( 'NONE',  ( -16.50258162057404832, -20.23145840177225807, 53.49999999999995026 ) ) ;
#36007 = DIRECTION ( 'NONE',  ( -3.484385612528001215E-15, 0.000000000000000000, 1.000000000000000000 ) ) ;
#36008 = CARTESIAN_POINT ( 'NONE',  ( -20.81696265954430558, -20.93198702957875668, 62.11471400680572685 ) ) ;
#36009 = ADVANCED_FACE ( 'NONE', ( #21718 ), #7445, .T. ) ;
#36010 = VERTEX_POINT ( 'NONE', #25182 ) ;
#36011 = PLANE ( 'NONE',  #29818 ) ;
#36012 = CARTESIAN_POINT ( 'NONE',  ( -13.41535183621916438, -9.069180408055801834, 64.13776496077019829 ) ) ;
#36013 = CARTESIAN_POINT ( 'NONE',  ( -20.88270815654435353, -21.40782497263450068, 58.82970582236164603 ) ) ;
#36014 = CARTESIAN_POINT ( 'NONE',  ( -23.44980260057077714, -18.46889688393208218, 72.76368236443251192 ) ) ;
#36015 = ORIENTED_EDGE ( 'NONE', *, *, #34150, .T. ) ;
#36016 = VERTEX_POINT ( 'NONE', #25649 ) ;
#36017 = CARTESIAN_POINT ( 'NONE',  ( -16.39284385541304800, -8.630756214087126565, 51.74842643355248129 ) ) ;
#36018 = CARTESIAN_POINT ( 'NONE',  ( -13.18702109819586710, -9.237203801506172596, 64.01832437545327537 ) ) ;
#36019 = AXIS2_PLACEMENT_3D ( 'NONE', #4334, #20319, #38783 ) ;
#36020 = CARTESIAN_POINT ( 'NONE',  ( -12.06140467229625912, -20.05244645202335008, 53.49999999999994316 ) ) ;
#36021 = CIRCLE ( 'NONE', #9293, 1.000000000000000888 ) ;
#36022 = AXIS2_PLACEMENT_3D ( 'NONE', #30875, #12628, #41705 ) ;
#36023 = VECTOR ( 'NONE', #24324, 1000.000000000000000 ) ;
#36024 = CARTESIAN_POINT ( 'NONE',  ( -22.91174631722474686, -10.46344187337216169, 59.79306521909829542 ) ) ;
#36025 = LINE ( 'NONE', #17315, #27750 ) ;
#36026 = ORIENTED_EDGE ( 'NONE', *, *, #39825, .T. ) ;
#36027 = DIRECTION ( 'NONE',  ( 1.000000000000000000, 0.000000000000000000, 0.000000000000000000 ) ) ;
#36028 = CIRCLE ( 'NONE', #691, 2.000000000000000000 ) ;
#36029 = FACE_OUTER_BOUND ( 'NONE', #1668, .T. ) ;
#36030 = VERTEX_POINT ( 'NONE', #18004 ) ;
#36031 =( BOUNDED_CURVE ( )  B_SPLINE_CURVE ( 3, ( #293, #18483, #4452, #41890 ),
 .UNSPECIFIED., .F., .F. ) 
 B_SPLINE_CURVE_WITH_KNOTS ( ( 4, 4 ),
 ( 0.000000000000000000, 0.4074455897393691739 ),
 .UNSPECIFIED. ) 
 CURVE ( )  GEOMETRIC_REPRESENTATION_ITEM ( )  RATIONAL_B_SPLINE_CURVE ( ( 1.000000000000000000, 0.4567392136813293035, 0.3561768502900293232, 0.6983129098261000589 ) ) 
 REPRESENTATION_ITEM ( '' )  );
#36032 = CARTESIAN_POINT ( 'NONE',  ( -23.04367457972577427, -10.55211693511195215, 59.75203429192391269 ) ) ;
#36033 = CARTESIAN_POINT ( 'NONE',  ( -11.91076409904084699, -14.84341972694825884, 53.69233794759168177 ) ) ;
#36034 = ORIENTED_EDGE ( 'NONE', *, *, #47664, .F. ) ;
#36035 = PLANE ( 'NONE',  #18160 ) ;
#36036 = DIRECTION ( 'NONE',  ( -3.071710424422018668E-17, 6.404604876783312462E-16, 1.000000000000000000 ) ) ;
#36037 = EDGE_LOOP ( 'NONE', ( #45745, #12551, #2007, #7509 ) ) ;
#36038 = CARTESIAN_POINT ( 'NONE',  ( -17.52077441883401576, -21.86154573861348283, 58.82041992746825798 ) ) ;
#36039 = ADVANCED_FACE ( 'NONE', ( #29352 ), #33258, .F. ) ;
#36040 = CARTESIAN_POINT ( 'NONE',  ( -24.42668993457695592, -13.99045928592870958, 73.40799407547365263 ) ) ;
#36041 = DIRECTION ( 'NONE',  ( -3.071710424422018668E-17, 6.404604876783312462E-16, 1.000000000000000000 ) ) ;
#36042 = CARTESIAN_POINT ( 'NONE',  ( -24.69524243360033111, -13.18581942010154506, 59.50121368153175183 ) ) ;
#36043 = VERTEX_POINT ( 'NONE', #44384 ) ;
#36044 = FACE_OUTER_BOUND ( 'NONE', #40935, .T. ) ;
#36045 = DIRECTION ( 'NONE',  ( 0.9687793358424821033, -0.2479245821708677133, 0.000000000000000000 ) ) ;
#36047 =( BOUNDED_SURFACE ( )  B_SPLINE_SURFACE ( 3, 1, ( 
 ( #4519, #27175 ),
 ( #2279, #13342 ),
 ( #47357, #39708 ),
 ( #16799, #28861 ),
 ( #43905, #32556 ),
 ( #5973, #24465 ),
 ( #20996, #17287 ) ),
 .UNSPECIFIED., .T., .F., .F. ) 
 B_SPLINE_SURFACE_WITH_KNOTS ( ( 4, 3, 4 ),
 ( 2, 2 ),
 ( 0.000000000000000000, 0.5000000000000000000, 1.000000000000000000 ),
 ( 0.000000000000000000, 1.000000000000000000 ),
 .UNSPECIFIED. ) 
 GEOMETRIC_REPRESENTATION_ITEM ( )  RATIONAL_B_SPLINE_SURFACE ( (
 ( 1.000000000000000000, 1.000000000000000000),
 ( 0.3333333333333335369, 0.3333333333333330373),
 ( 0.3333333333333335369, 0.3333333333333330373),
 ( 1.000000000000000000, 1.000000000000000000),
 ( 0.3333333333333333703, 0.3333333333333333703),
 ( 0.3333333333333333703, 0.3333333333333333703),
 ( 1.000000000000000000, 1.000000000000000000) ) ) 
 REPRESENTATION_ITEM ( '' )  SURFACE ( )  );
#36046 = DIRECTION ( 'NONE',  ( -0.000000000000000000, 1.000000000000000000, -0.000000000000000000 ) ) ;
#36048 = EDGE_CURVE ( 'NONE', #22956, #14468, #43109, .T. ) ;
#36049 = DIRECTION ( 'NONE',  ( 0.9687793358424822143, -0.2479245821708672415, 0.000000000000000000 ) ) ;
#36050 = EDGE_CURVE ( 'NONE', #41929, #8183, #18450, .T. ) ;
#36051 = AXIS2_PLACEMENT_3D ( 'NONE', #7188, #10395, #33003 ) ;
#36052 = DIRECTION ( 'NONE',  ( 0.9687793358424821033, -0.2479245821708679076, 0.000000000000000000 ) ) ;
#36053 = DIRECTION ( 'NONE',  ( -6.651268172957068788E-06, -3.577353461959433263E-06, -0.9999999999714815901 ) ) ;
#36054 = ORIENTED_EDGE ( 'NONE', *, *, #305, .F. ) ;
#36055 = CARTESIAN_POINT ( 'NONE',  ( -13.84130163926618451, -8.277085044245813705, 74.35988050052598908 ) ) ;
#36056 = EDGE_CURVE ( 'NONE', #9562, #12573, #33380, .T. ) ;
#36057 = CARTESIAN_POINT ( 'NONE',  ( -13.49145512112739631, -18.65424914341562612, 54.07175714974879099 ) ) ;
#36058 = DIRECTION ( 'NONE',  ( 2.866981220435666553E-17, -1.000000000000000000, -1.190614954331866791E-16 ) ) ;
#36059 = ORIENTED_EDGE ( 'NONE', *, *, #7034, .F. ) ;
#36060 = CARTESIAN_POINT ( 'NONE',  ( -23.74619265052512418, -11.68934008440959893, 62.95218278636777143 ) ) ;
#36061 = VECTOR ( 'NONE', #35867, 1000.000000000000114 ) ;
#36062 = AXIS2_PLACEMENT_3D ( 'NONE', #2578, #17580, #21048 ) ;
#36063 = ORIENTED_EDGE ( 'NONE', *, *, #18242, .F. ) ;
#36064 = VERTEX_POINT ( 'NONE', #22210 ) ;
#36065 = EDGE_LOOP ( 'NONE', ( #17125, #47327 ) ) ;
#36066 = CARTESIAN_POINT ( 'NONE',  ( -14.07761835836965858, -20.95746660330474143, 72.22607703844037985 ) ) ;
#36067 = VECTOR ( 'NONE', #11176, 1000.000000000000114 ) ;
#36068 = CARTESIAN_POINT ( 'NONE',  ( -23.76771070410665132, -11.84943609209516424, 59.48235735874851571 ) ) ;
#36069 = PLANE ( 'NONE',  #8671 ) ;
#36070 = CARTESIAN_POINT ( 'NONE',  ( -15.13034385759799072, -6.857644439848019857, 49.98602051094139398 ) ) ;
#36071 = CARTESIAN_POINT ( 'NONE',  ( -27.42409385541305156, -14.65920654474411045, 52.21286476528344878 ) ) ;
#36072 = EDGE_LOOP ( 'NONE', ( #39741, #42089, #47383, #43992 ) ) ;
#36073 = ORIENTED_EDGE ( 'NONE', *, *, #32649, .T. ) ;
#36074 = CARTESIAN_POINT ( 'NONE',  ( -18.67409385650551457, -9.792211528768504536, 50.49490371617623197 ) ) ;
#36075 = CARTESIAN_POINT ( 'NONE',  ( -18.46801905451614445, -7.836623195388688679, 74.12592262855558545 ) ) ;
#36076 = CARTESIAN_POINT ( 'NONE',  ( -11.77193539988124371, -19.02301398277157318, 71.98685856039797670 ) ) ;
#36077 = CARTESIAN_POINT ( 'NONE',  ( -19.40534385650551741, -8.801233750844183135, 48.81488406609782515 ) ) ;
#36078 = EDGE_LOOP ( 'NONE', ( #19559, #316, #13507, #11834 ) ) ;
#36079 = CARTESIAN_POINT ( 'NONE',  ( -15.41904748403203484, -7.634001509309876532, 74.19490257054667381 ) ) ;
#36080 = AXIS2_PLACEMENT_3D ( 'NONE', #43069, #25331, #47499 ) ;
#36081 = CARTESIAN_POINT ( 'NONE',  ( -24.87421550414592986, -14.80086288727809141, 59.42017156831820301 ) ) ;
#36082 = CARTESIAN_POINT ( 'NONE',  ( -14.11784385759798965, -6.860780111191487229, 51.02154966934377711 ) ) ;
#36083 = EDGE_CURVE ( 'NONE', #11147, #28351, #37197, .T. ) ;
#36084 = ORIENTED_EDGE ( 'NONE', *, *, #4299, .F. ) ;
#36085 = CARTESIAN_POINT ( 'NONE',  ( -17.42409385541299471, -14.80920654474434883, 62.02966884056656482 ) ) ;
#36086 = AXIS2_PLACEMENT_3D ( 'NONE', #11600, #26629, #18737 ) ;
#36087 = VECTOR ( 'NONE', #12088, 1000.000000000000227 ) ;
#36088 = ORIENTED_EDGE ( 'NONE', *, *, #28900, .F. ) ;
#36089 = CARTESIAN_POINT ( 'NONE',  ( -19.76784385541295919, -9.357632978295972848, 49.97845033065677001 ) ) ;
#36090 = CARTESIAN_POINT ( 'NONE',  ( -16.28253830925437384, -21.71555932027983715, 58.57120154339385465 ) ) ;
#36091 = CARTESIAN_POINT ( 'NONE',  ( -18.97054410961560578, -7.521390078327941708, 67.08567059339527816 ) ) ;
#36092 = ORIENTED_EDGE ( 'NONE', *, *, #40438, .T. ) ;
#36093 = VECTOR ( 'NONE', #41637, 1000.000000000000000 ) ;
#36094 = CARTESIAN_POINT ( 'NONE',  ( -19.37484727228654080, -7.619050864103940057, 60.14588289477547534 ) ) ;
#36095 = CARTESIAN_POINT ( 'NONE',  ( -23.12535468111908443, -10.01343724238356359, 66.65686954956312604 ) ) ;
#36096 = CARTESIAN_POINT ( 'NONE',  ( -20.18941624216641273, -7.891347737435665977, 73.83601159825586535 ) ) ;
#36097 = ORIENTED_EDGE ( 'NONE', *, *, #5511, .F. ) ;
#36098 = CYLINDRICAL_SURFACE ( 'NONE', #12620, 0.1499999999999986067 ) ;
#36099 = CARTESIAN_POINT ( 'NONE',  ( -24.45714095472541771, -14.31630891555218987, 69.66747352629326429 ) ) ;
#36100 = EDGE_LOOP ( 'NONE', ( #47536, #36059, #13228, #34049 ) ) ;
#36101 = CARTESIAN_POINT ( 'NONE',  ( -13.45889463159840282, -8.979947265385323618, 60.43950308547118766 ) ) ;
#36102 = PLANE ( 'NONE',  #9161 ) ;
#36103 = ORIENTED_EDGE ( 'NONE', *, *, #39276, .F. ) ;
#36104 = CARTESIAN_POINT ( 'NONE',  ( -20.19053640067075506, -7.838066347919499854, 53.49999999999994316 ) ) ;
#36105 = DIRECTION ( 'NONE',  ( -0.2479245821708678799, -0.9687793358424819923, -2.626836608253746575E-18 ) ) ;
#36106 = CARTESIAN_POINT ( 'NONE',  ( -24.46506355971582991, -17.24406257311080992, 72.99840714145864240 ) ) ;
#36107 = ADVANCED_FACE ( 'NONE', ( #1018 ), #23189, .T. ) ;
#36108 = CARTESIAN_POINT ( 'NONE',  ( -45.92409385541306222, -14.20920654474410760, 70.50000000000000000 ) ) ;
#36109 = ORIENTED_EDGE ( 'NONE', *, *, #493, .T. ) ;
#36110 = CARTESIAN_POINT ( 'NONE',  ( -23.44980356754079054, -18.46889531339634871, 72.91368236442116313 ) ) ;
#36111 = EDGE_CURVE ( 'NONE', #29137, #656, #24177, .T. ) ;
#36112 = CARTESIAN_POINT ( 'NONE',  ( -19.12409385759799108, -9.359200813967568422, 50.49621490985803263 ) ) ;
#36113 = CARTESIAN_POINT ( 'NONE',  ( -24.93953149451673568, -10.04808947811604902, 53.49999999999995026 ) ) ;
#36114 = EDGE_LOOP ( 'NONE', ( #28895, #6036 ) ) ;
#36115 = ADVANCED_FACE ( 'NONE', ( #38681 ), #31170, .T. ) ;
#36116 = CARTESIAN_POINT ( 'NONE',  ( -17.92193035392797285, -21.84160718002658541, 61.87535923543195793 ) ) ;
#36117 = B_SPLINE_CURVE_WITH_KNOTS ( 'NONE', 1,
 ( #18097, #44243 ),
 .UNSPECIFIED., .F., .F.,
 ( 2, 2 ),
 ( 0.000000000000000000, 1.000000000000000000 ),
 .UNSPECIFIED. ) ;
#36118 = ORIENTED_EDGE ( 'NONE', *, *, #7851, .T. ) ;
#36119 = ORIENTED_EDGE ( 'NONE', *, *, #7303, .T. ) ;
#36120 = CARTESIAN_POINT ( 'NONE',  ( -10.37497031247464463, -14.69804315800203476, 71.62782692816419683 ) ) ;
#36121 = CARTESIAN_POINT ( 'NONE',  ( -15.66732230932660741, -10.46443543628982553, 49.52966884056655772 ) ) ;
#36123 = CARTESIAN_POINT ( 'NONE',  ( -10.02024861317775262, -15.63870305697176377, 61.19935569097407324 ) ) ;
#36122 = VECTOR ( 'NONE', #40822, 1000.000000000000000 ) ;
#36124 =( BOUNDED_SURFACE ( )  B_SPLINE_SURFACE ( 3, 1, ( 
 ( #29051, #47533 ),
 ( #13767, #25364 ),
 ( #32737, #7140 ),
 ( #14245, #25592 ),
 ( #36183, #28811 ),
 ( #26094, #17944 ),
 ( #10583, #44098 ) ),
 .UNSPECIFIED., .T., .F., .F. ) 
 B_SPLINE_SURFACE_WITH_KNOTS ( ( 4, 3, 4 ),
 ( 2, 2 ),
 ( 0.000000000000000000, 0.5000000000000000000, 1.000000000000000000 ),
 ( 0.000000000000000000, 1.000000000000000000 ),
 .UNSPECIFIED. ) 
 GEOMETRIC_REPRESENTATION_ITEM ( )  RATIONAL_B_SPLINE_SURFACE ( (
 ( 1.000000000000000000, 1.000000000000000000),
 ( 0.3333333333333335369, 0.3333333333333330373),
 ( 0.3333333333333335369, 0.3333333333333330373),
 ( 1.000000000000000000, 1.000000000000000000),
 ( 0.3333333333333333703, 0.3333333333333333703),
 ( 0.3333333333333333703, 0.3333333333333333703),
 ( 1.000000000000000000, 1.000000000000000000) ) ) 
 REPRESENTATION_ITEM ( '' )  SURFACE ( )  );
#36125 = CARTESIAN_POINT ( 'NONE',  ( -19.99284385650551243, -7.406986770994973490, 48.81910596585309747 ) ) ;
#36126 = DIRECTION ( 'NONE',  ( -0.6105870317843965500, -0.7919491628991826015, 6.540688078712152548E-08 ) ) ;
#36128 = EDGE_CURVE ( 'NONE', #2367, #48136, #27137, .T. ) ;
#36127 = CARTESIAN_POINT ( 'NONE',  ( -23.89279295945009096, -11.11331726805715725, 69.93564813258274171 ) ) ;
#36129 = CARTESIAN_POINT ( 'NONE',  ( -14.93036884410937937, -8.267093201351965348, 60.39166468221263528 ) ) ;
#36130 = CARTESIAN_POINT ( 'NONE',  ( -12.24887892415898172, -20.16835215658221969, 65.05949058504921823 ) ) ;
#36131 = VECTOR ( 'NONE', #44321, 1000.000000000000114 ) ;
#36132 = ORIENTED_EDGE ( 'NONE', *, *, #27670, .T. ) ;
#36133 = ORIENTED_EDGE ( 'NONE', *, *, #37210, .T. ) ;
#36134 = FACE_OUTER_BOUND ( 'NONE', #23066, .T. ) ;
#36135 = CARTESIAN_POINT ( 'NONE',  ( -23.06991199560340533, -9.948164920181065796, 66.68035737299506138 ) ) ;
#36136 = LINE ( 'NONE', #2421, #44116 ) ;
#36137 = VECTOR ( 'NONE', #1014, 1000.000000000000000 ) ;
#36138 = FACE_OUTER_BOUND ( 'NONE', #7060, .T. ) ;
#36139 = CARTESIAN_POINT ( 'NONE',  ( -20.48427295952909688, -21.16374346551129548, 59.05963865090804887 ) ) ;
#36140 = CARTESIAN_POINT ( 'NONE',  ( -19.88034385650552238, -6.424090610841174609, 49.80797279389977916 ) ) ;
#36141 = VERTEX_POINT ( 'NONE', #19735 ) ;
#36142 = CARTESIAN_POINT ( 'NONE',  ( -10.44881481234349252, -17.42631575494719698, 64.74243950200344955 ) ) ;
#36143 = CARTESIAN_POINT ( 'NONE',  ( -22.82423354248128078, -9.676858997600051637, 73.63161091602947295 ) ) ;
#36144 = CARTESIAN_POINT ( 'NONE',  ( -23.44980260057077714, -18.46889688393208573, 72.76368236443251192 ) ) ;
#36145 = ADVANCED_FACE ( 'NONE', ( #30346 ), #34745, .T. ) ;
#36146 = ORIENTED_EDGE ( 'NONE', *, *, #45364, .T. ) ;
#36147 = DIRECTION ( 'NONE',  ( -0.1240347345892086200, 2.341226830773357975E-16, -0.9922778767136676281 ) ) ;
#36148 = CYLINDRICAL_SURFACE ( 'NONE', #36080, 1.250000000000001110 ) ;
#36149 = DIRECTION ( 'NONE',  ( 0.000000000000000000, -0.007114381193220334181, 0.9999746924698833528 ) ) ;
#36150 = VECTOR ( 'NONE', #39067, 1000.000000000000000 ) ;
#36151 = FACE_OUTER_BOUND ( 'NONE', #23209, .T. ) ;
#36152 = EDGE_LOOP ( 'NONE', ( #28616, #2944, #21850, #46035, #28997 ) ) ;
#36153 = ADVANCED_FACE ( 'NONE', ( #31291 ), #46074, .T. ) ;
#36154 = DIRECTION ( 'NONE',  ( 8.560949391518745609E-06, -2.380493834460222846E-06, 0.9999999999605218015 ) ) ;
#36155 = VECTOR ( 'NONE', #25480, 1000.000000000000000 ) ;
#36156 = EDGE_LOOP ( 'NONE', ( #27855, #34589 ) ) ;
#36157 = CARTESIAN_POINT ( 'NONE',  ( -22.25476733894167580, -19.94415178569153468, 66.00421729349081090 ) ) ;
#36158 = CARTESIAN_POINT ( 'NONE',  ( -10.01510117332873584, -14.02744298369021969, 61.09634062789294973 ) ) ;
#36159 = ORIENTED_EDGE ( 'NONE', *, *, #27818, .F. ) ;
#36160 = CARTESIAN_POINT ( 'NONE',  ( -12.71302066933910524, -9.037873161084162277, 70.99925350880062069 ) ) ;
#36161 = CARTESIAN_POINT ( 'NONE',  ( -13.66784385650551670, -6.428312510596451368, 51.20221977374900035 ) ) ;
#36162 = ORIENTED_EDGE ( 'NONE', *, *, #37407, .F. ) ;
#36163 = LINE ( 'NONE', #43588, #8702 ) ;
#36164 =( BOUNDED_SURFACE ( )  B_SPLINE_SURFACE ( 3, 1, ( 
 ( #44409, #10663 ),
 ( #25927, #40940 ),
 ( #6969, #36983 ),
 ( #32813, #17311 ),
 ( #43685, #47844 ),
 ( #29133, #40451 ),
 ( #38198, #41188 ) ),
 .UNSPECIFIED., .T., .F., .F. ) 
 B_SPLINE_SURFACE_WITH_KNOTS ( ( 4, 3, 4 ),
 ( 2, 2 ),
 ( 0.000000000000000000, 0.5000000000000000000, 1.000000000000000000 ),
 ( 0.000000000000000000, 1.000000000000000000 ),
 .UNSPECIFIED. ) 
 GEOMETRIC_REPRESENTATION_ITEM ( )  RATIONAL_B_SPLINE_SURFACE ( (
 ( 1.000000000000000000, 1.000000000000000000),
 ( 0.3333333333333335369, 0.3333333333333330373),
 ( 0.3333333333333335369, 0.3333333333333330373),
 ( 1.000000000000000000, 1.000000000000000000),
 ( 0.3333333333333333703, 0.3333333333333333703),
 ( 0.3333333333333333703, 0.3333333333333333703),
 ( 1.000000000000000000, 1.000000000000000000) ) ) 
 REPRESENTATION_ITEM ( '' )  SURFACE ( )  );
#36165 = CARTESIAN_POINT ( 'NONE',  ( -20.00946503018472811, -8.250368534377352958, 73.72096600125085786 ) ) ;
#36166 = FACE_OUTER_BOUND ( 'NONE', #17010, .T. ) ;
#36167 = EDGE_LOOP ( 'NONE', ( #40167, #38432, #46913, #37653, #8423 ) ) ;
#36168 = CARTESIAN_POINT ( 'NONE',  ( -13.47245400663725690, -21.12492667118925382, 65.10133491818508844 ) ) ;
#36169 = DIRECTION ( 'NONE',  ( -0.7506333037770538397, 0.6607190350373941534, 0.000000000000000000 ) ) ;
#36170 = EDGE_CURVE ( 'NONE', #30487, #40380, #36186, .T. ) ;
#36171 = CARTESIAN_POINT ( 'NONE',  ( -11.32604004198825365, -11.37209441256710463, 60.86988868631853933 ) ) ;
#36172 = CARTESIAN_POINT ( 'NONE',  ( -22.91943239076679006, -10.38811108791941429, 59.48714571049892896 ) ) ;
#36174 = CLOSED_SHELL ( 'NONE', ( #40917, #8819, #39251, #14005, #21564, #24503, #78, #12257, #26049, #25267, #32184, #36792, #14079, #41238, #37845, #22127, #15659, #16642, #22727, #42577, #43213, #20726, #37901, #8747, #4109, #22631, #9564, #30229, #16143, #1971, #30123, #37133, #40700, #43668, #5818, #39906, #16873, #13781, #21922, #29564, #46164, #27624, #14739 ) ) ;
#36173 = ORIENTED_EDGE ( 'NONE', *, *, #30849, .F. ) ;
#36175 = ORIENTED_EDGE ( 'NONE', *, *, #44201, .T. ) ;
#36176 = EDGE_CURVE ( 'NONE', #37218, #35836, #9833, .T. ) ;
#36177 = CARTESIAN_POINT ( 'NONE',  ( -23.79811132998510459, -18.66596081585729650, 72.86344597896119524 ) ) ;
#36178 = DIRECTION ( 'NONE',  ( 0.000000000000000000, 1.000000000000000000, -9.912705577010318647E-16 ) ) ;
#36179 = ORIENTED_EDGE ( 'NONE', *, *, #10619, .T. ) ;
#36180 = CARTESIAN_POINT ( 'NONE',  ( -20.75149224175378748, -8.143498925893005946, 63.50459817289195996 ) ) ;
#36181 = EDGE_CURVE ( 'NONE', #26883, #10524, #39703, .T. ) ;
#36182 = CARTESIAN_POINT ( 'NONE',  ( -18.05534385759799321, -8.623186033802570094, 49.24843789510466507 ) ) ;
#36183 = CARTESIAN_POINT ( 'NONE',  ( -23.89460186926044472, -11.99007647016461320, 63.09651074612323640 ) ) ;
#36184 = DIRECTION ( 'NONE',  ( 1.000000000000000000, 0.000000000000000000, 0.000000000000000000 ) ) ;
#36185 = CARTESIAN_POINT ( 'NONE',  ( -15.61945779041031201, -7.581001026129836617, 70.86635785818099009 ) ) ;
#36186 =( BOUNDED_CURVE ( )  B_SPLINE_CURVE ( 3, ( #42387, #8657, #26385, #41400 ),
 .UNSPECIFIED., .F., .F. ) 
 B_SPLINE_CURVE_WITH_KNOTS ( ( 4, 4 ),
 ( 0.000000000000000000, 0.4074455897393690629 ),
 .UNSPECIFIED. ) 
 CURVE ( )  GEOMETRIC_REPRESENTATION_ITEM ( )  RATIONAL_B_SPLINE_CURVE ( ( 1.000000000000000000, 0.4567392136813264170, 0.3561768502900282130, 0.6983129098261053880 ) ) 
 REPRESENTATION_ITEM ( '' )  );
#36187 = VERTEX_POINT ( 'NONE', #41653 ) ;
#36188 = DIRECTION ( 'NONE',  ( 0.9687793358424821033, -0.2479245821708678243, 0.000000000000000000 ) ) ;
#36189 = B_SPLINE_CURVE_WITH_KNOTS ( 'NONE', 3,
 ( #24412, #5214, #35229, #1504 ),
 .UNSPECIFIED., .F., .F.,
 ( 4, 4 ),
 ( 0.000000000000000000, 0.1735808155647264317 ),
 .UNSPECIFIED. ) ;
#36190 = DIRECTION ( 'NONE',  ( -2.081668171172170091E-15, 0.000000000000000000, 1.000000000000000000 ) ) ;
#36191 = CARTESIAN_POINT ( 'NONE',  ( -22.80485643099853021, -9.656470841191969967, 73.67435257262538073 ) ) ;
#36192 = CARTESIAN_POINT ( 'NONE',  ( -16.58312381330344110, -22.21171629078730092, 65.40281258638998452 ) ) ;
#36193 = ADVANCED_FACE ( 'NONE', ( #20465 ), #46801, .F. ) ;
#36194 = AXIS2_PLACEMENT_3D ( 'NONE', #40681, #41414, #37458 ) ;
#36195 = EDGE_CURVE ( 'NONE', #25586, #42260, #12611, .T. ) ;
#36196 = ORIENTED_EDGE ( 'NONE', *, *, #7241, .T. ) ;
#36197 =( BOUNDED_CURVE ( )  B_SPLINE_CURVE ( 3, ( #38026, #44466, #37285, #25992 ),
 .UNSPECIFIED., .F., .F. ) 
 B_SPLINE_CURVE_WITH_KNOTS ( ( 4, 4 ),
 ( 0.5000000000000000000, 0.9074455897393720605 ),
 .UNSPECIFIED. ) 
 CURVE ( )  GEOMETRIC_REPRESENTATION_ITEM ( )  RATIONAL_B_SPLINE_CURVE ( ( 0.9999999999999906741, 0.4567392136813236414, 0.3561768502900335420, 0.6983129098261104950 ) ) 
 REPRESENTATION_ITEM ( '' )  );
#36198 = ORIENTED_EDGE ( 'NONE', *, *, #42706, .F. ) ;
#36199 = ADVANCED_FACE ( 'NONE', ( #35219 ), #16739, .F. ) ;
#36200 = EDGE_CURVE ( 'NONE', #19733, #32100, #46004, .T. ) ;
#36201 = CARTESIAN_POINT ( 'NONE',  ( -10.85011828021597857, -12.40413123133334850, 57.32857331434495052 ) ) ;
#36202 = CARTESIAN_POINT ( 'NONE',  ( -22.60238019587661995, -10.09889146956836825, 70.31178508704351771 ) ) ;
#36203 = FACE_OUTER_BOUND ( 'NONE', #7189, .T. ) ;
#36204 = CIRCLE ( 'NONE', #7908, 5.249999999999998224 ) ;
#36205 = EDGE_LOOP ( 'NONE', ( #14939, #17728, #4352, #20638 ) ) ;
#36206 = B_SPLINE_CURVE_WITH_KNOTS ( 'NONE', 3,
 ( #4165, #26555, #12259, #230, #42308, #34667, #15443, #30515, #38605, #19897 ),
 .UNSPECIFIED., .F., .F.,
 ( 4, 2, 2, 2, 4 ),
 ( 0.000000000000000000, 0.2500000000000000000, 0.5000000000000000000, 0.7500000000000000000, 1.000000000000000000 ),
 .UNSPECIFIED. ) ;
#36207 = CARTESIAN_POINT ( 'NONE',  ( -16.16063032598464133, -7.467038112641824377, 60.38523865926408263 ) ) ;
#36208 = CARTESIAN_POINT ( 'NONE',  ( -12.57881008754452345, -9.149975892475048056, 74.57568945445216002 ) ) ;
#36209 = CIRCLE ( 'NONE', #5595, 7.000000000000000888 ) ;
#36210 = EDGE_LOOP ( 'NONE', ( #43734, #7828, #20954, #46386, #10609 ) ) ;
#36211 = CARTESIAN_POINT ( 'NONE',  ( -10.99655682251556144, -18.57624055219563175, 57.99209882808910521 ) ) ;
#36212 = CARTESIAN_POINT ( 'NONE',  ( -12.52433193127781408, -20.42124925782731992, 71.90679425634165511 ) ) ;
#36213 = CARTESIAN_POINT ( 'NONE',  ( -15.88656107989463706, -7.980151544674868980, 67.14007279409138107 ) ) ;
#36214 = ORIENTED_EDGE ( 'NONE', *, *, #24685, .F. ) ;
#36215 = CARTESIAN_POINT ( 'NONE',  ( -24.16181610925939793, -12.90510579204740083, 69.96170108456067283 ) ) ;
#36216 = ORIENTED_EDGE ( 'NONE', *, *, #15879, .T. ) ;
#36217 = CARTESIAN_POINT ( 'NONE',  ( -24.34442481654545176, -17.56831618823577301, 65.98711337262309939 ) ) ;
#36218 = CARTESIAN_POINT ( 'NONE',  ( -18.39284385759799179, -8.630756214087126565, 51.74842643355248129 ) ) ;
#36219 = DIRECTION ( 'NONE',  ( 0.6172023957221189905, 0.7799807200343574776, 0.1033986416233889649 ) ) ;
#36220 = ORIENTED_EDGE ( 'NONE', *, *, #21553, .F. ) ;
#36221 = PLANE ( 'NONE',  #41186 ) ;
#36222 = ADVANCED_FACE ( 'NONE', ( #5200 ), #39160, .T. ) ;
#36223 = CARTESIAN_POINT ( 'NONE',  ( -10.48245863704348579, -16.06162050378864592, 64.50771356773347520 ) ) ;
#36224 = CARTESIAN_POINT ( 'NONE',  ( -14.60689786731817286, -8.346551761976032324, 63.93978840692965093 ) ) ;
#36225 = VECTOR ( 'NONE', #36403, 1000.000000000000000 ) ;
#36226 = FACE_OUTER_BOUND ( 'NONE', #16777, .T. ) ;
#36227 = LINE ( 'NONE', #13804, #20599 ) ;
#36228 = CARTESIAN_POINT ( 'NONE',  ( -20.52513420828390878, -21.08626482067204577, 58.87305014468301323 ) ) ;
#36229 = ORIENTED_EDGE ( 'NONE', *, *, #9829, .T. ) ;
#36230 = CIRCLE ( 'NONE', #858, 2.000000000000002665 ) ;
#36231 = CARTESIAN_POINT ( 'NONE',  ( -18.36828968083242231, -10.20659317963781021, 49.52966884056655772 ) ) ;
#36232 = CARTESIAN_POINT ( 'NONE',  ( -11.64187585391237612, -10.11031112578646152, 67.61241562450165077 ) ) ;
#36233 = DIRECTION ( 'NONE',  ( -0.9753750245375039096, -0.2205528542287732985, -7.244220463057848842E-08 ) ) ;
#36234 = CARTESIAN_POINT ( 'NONE',  ( -13.35818949714929360, -21.05197827947291955, 61.70141596610112344 ) ) ;
#36235 = EDGE_CURVE ( 'NONE', #20160, #31757, #5126, .T. ) ;
#36236 = CARTESIAN_POINT ( 'NONE',  ( -23.88415217903648369, -17.63235132829416685, 62.77360984996715842 ) ) ;
#36237 = CARTESIAN_POINT ( 'NONE',  ( -13.52409385650551599, -6.426201560718813433, 50.50509628382439331 ) ) ;
#36238 = VERTEX_POINT ( 'NONE', #47294 ) ;
#36239 = VERTEX_POINT ( 'NONE', #39649 ) ;
#36240 = DIRECTION ( 'NONE',  ( -1.000000000000000000, 0.000000000000000000, -8.260587980841940012E-17 ) ) ;
#36241 = LINE ( 'NONE', #21242, #3789 ) ;
#36242 = VERTEX_POINT ( 'NONE', #35693 ) ;
#36243 = CARTESIAN_POINT ( 'NONE',  ( -11.76008542200333018, -19.01204350050032232, 68.10200740694565980 ) ) ;
#36244 = CARTESIAN_POINT ( 'NONE',  ( -10.47603521207407518, -16.02136065384195973, 71.86239274348770323 ) ) ;
#36245 = CIRCLE ( 'NONE', #6375, 1.250000000000001110 ) ;
#36246 = CARTESIAN_POINT ( 'NONE',  ( -11.64235026963700470, -18.84330375823651949, 68.21689631561287115 ) ) ;
#36247 = DIRECTION ( 'NONE',  ( -1.474291233076046698E-06, -1.298191854940810726E-06, 0.9999999999980706544 ) ) ;
#36248 = DIRECTION ( 'NONE',  ( -0.9939059412784551073, -0.1102314832132140487, -5.576311684675194245E-08 ) ) ;
#36249 = ORIENTED_EDGE ( 'NONE', *, *, #25297, .T. ) ;
#36250 = FACE_BOUND ( 'NONE', #46870, .T. ) ;
#36251 = CARTESIAN_POINT ( 'NONE',  ( -23.88506662780487133, -17.50400919611850270, 65.95973823122339752 ) ) ;
#36252 = CARTESIAN_POINT ( 'NONE',  ( -45.92409385541306222, -13.51240245935757578, 70.50000000000000000 ) ) ;
#36253 = CARTESIAN_POINT ( 'NONE',  ( -20.73422126667899690, -8.581213913796407411, 63.72610227039507436 ) ) ;
#36254 = ORIENTED_EDGE ( 'NONE', *, *, #10036, .T. ) ;
#36255 = AXIS2_PLACEMENT_3D ( 'NONE', #17622, #44010, #10265 ) ;
#36256 = CARTESIAN_POINT ( 'NONE',  ( -11.02370713164636129, -10.86456322469730118, 54.02312124697527906 ) ) ;
#36257 = CARTESIAN_POINT ( 'NONE',  ( -18.73538018142495432, -21.73996178052156836, 72.28510691925902165 ) ) ;
#36258 = CARTESIAN_POINT ( 'NONE',  ( -16.93941734680482725, -7.775588144984237005, 74.24546186738449194 ) ) ;
#36259 = CARTESIAN_POINT ( 'NONE',  ( -24.20371252810814866, -12.87440185077122834, 66.58774614429587757 ) ) ;
#36260 = FACE_OUTER_BOUND ( 'NONE', #7376, .T. ) ;
#36261 = DIRECTION ( 'NONE',  ( -0.1464579420318390945, 0.9892168979631277281, 7.284849527811297202E-08 ) ) ;
#36263 = EDGE_LOOP ( 'NONE', ( #25440, #48647 ) ) ;
#36262 = EDGE_CURVE ( 'NONE', #8500, #27898, #17625, .T. ) ;
#36264 = ORIENTED_EDGE ( 'NONE', *, *, #46851, .F. ) ;
#36265 = CARTESIAN_POINT ( 'NONE',  ( -17.29284385541304303, -8.630756214087126565, 51.74842643355248129 ) ) ;
#36266 = EDGE_CURVE ( 'NONE', #13505, #34212, #38876, .T. ) ;
#36267 = ADVANCED_FACE ( 'NONE', ( #46325 ), #42640, .T. ) ;
#36268 = DIRECTION ( 'NONE',  ( -5.731567514496413899E-31, -1.020425574103664789E-16, -1.000000000000000000 ) ) ;
#36269 = CIRCLE ( 'NONE', #127, 2.000000000000000888 ) ;
#36270 = DIRECTION ( 'NONE',  ( -0.9998756790481366785, -0.01576789294826319923, -3.907472230461692677E-09 ) ) ;
#36271 = AXIS2_PLACEMENT_3D ( 'NONE', #2494, #21213, #17497 ) ;
#36272 = EDGE_CURVE ( 'NONE', #22946, #32101, #19514, .T. ) ;
#36273 = EDGE_CURVE ( 'NONE', #1406, #19538, #42978, .T. ) ;
#36274 = CARTESIAN_POINT ( 'NONE',  ( -24.59706333651279664, -12.79617740830267891, 66.48742133194130588 ) ) ;
#36275 = CARTESIAN_POINT ( 'NONE',  ( -24.31823732957325745, -17.63313362019280106, 66.05861802595141796 ) ) ;
#36276 = EDGE_LOOP ( 'NONE', ( #37560, #29099 ) ) ;
#36277 = CARTESIAN_POINT ( 'NONE',  ( -19.30706890485013005, -22.01740903849647069, 58.64011989901568711 ) ) ;
#36278 = CARTESIAN_POINT ( 'NONE',  ( -20.89788161767221197, -20.94431024770144489, 62.39999296070408974 ) ) ;
#36279 = ORIENTED_EDGE ( 'NONE', *, *, #6819, .F. ) ;
#36280 = CARTESIAN_POINT ( 'NONE',  ( -17.93641254378128025, -22.24158300746090333, 61.97561672547572442 ) ) ;
#36281 = CARTESIAN_POINT ( 'NONE',  ( -20.61159385541303379, -8.990409506049216404, 49.61344411288074241 ) ) ;
#36282 = ORIENTED_EDGE ( 'NONE', *, *, #10169, .F. ) ;
#36283 = CARTESIAN_POINT ( 'NONE',  ( -33.95962776134579286, -8.109206544744111511, 51.75000000000000711 ) ) ;
#36284 = CARTESIAN_POINT ( 'NONE',  ( -10.42310822017611649, -15.66923192643957385, 57.77612719067403191 ) ) ;
#36285 = ORIENTED_EDGE ( 'NONE', *, *, #45972, .F. ) ;
#36286 = CARTESIAN_POINT ( 'NONE',  ( -20.20256548602924696, -7.896530927994315441, 73.88243076186758174 ) ) ;
#36287 = EDGE_CURVE ( 'NONE', #33881, #22937, #47580, .T. ) ;
#36288 = AXIS2_PLACEMENT_3D ( 'NONE', #20742, #35739, #47569 ) ;
#36289 = CARTESIAN_POINT ( 'NONE',  ( -24.44334717380189659, -17.30795561478116085, 69.52684539094292404 ) ) ;
#36290 = CARTESIAN_POINT ( 'NONE',  ( -16.59344707466788549, -21.75974795715521282, 65.52564390620075585 ) ) ;
#36291 = ORIENTED_EDGE ( 'NONE', *, *, #3328, .F. ) ;
#36292 = PLANE ( 'NONE',  #27383 ) ;
#36293 = CARTESIAN_POINT ( 'NONE',  ( -24.26384900572966075, -13.06773595597165460, 69.91676003018049812 ) ) ;
#36294 = CARTESIAN_POINT ( 'NONE',  ( -12.37139604325248499, -19.73008851950320519, 57.81193715039307079 ) ) ;
#36295 = AXIS2_PLACEMENT_3D ( 'NONE', #44235, #47907, #33340 ) ;
#36296 = CARTESIAN_POINT ( 'NONE',  ( -17.42409385541299471, -14.80920654474435771, 49.52966884056655772 ) ) ;
#36297 = CARTESIAN_POINT ( 'NONE',  ( -22.41159385650551528, -6.922745924619793101, 51.69366785382590024 ) ) ;
#36298 = CARTESIAN_POINT ( 'NONE',  ( -23.11971029740161754, -18.96910916387263768, 66.23878312252503520 ) ) ;
#36299 = ORIENTED_EDGE ( 'NONE', *, *, #13411, .T. ) ;
#36300 = CARTESIAN_POINT ( 'NONE',  ( -13.91015139505516984, -8.239921989797695190, 74.30680484912956274 ) ) ;
#36301 = CARTESIAN_POINT ( 'NONE',  ( -18.55453542384412557, -21.76813569768954792, 72.57951126079657911 ) ) ;
#36302 = CARTESIAN_POINT ( 'NONE',  ( -10.00346675491595683, -15.47019071557144443, 57.76804009592240874 ) ) ;
#36303 = ORIENTED_EDGE ( 'NONE', *, *, #3993, .T. ) ;
#36304 = CARTESIAN_POINT ( 'NONE',  ( -17.74284385541294284, -7.587656875400116796, 49.25157356644795925 ) ) ;
#36305 = ORIENTED_EDGE ( 'NONE', *, *, #14808, .F. ) ;
#36306 = ORIENTED_EDGE ( 'NONE', *, *, #2479, .F. ) ;
#36307 = ORIENTED_EDGE ( 'NONE', *, *, #1089, .T. ) ;
#36308 = CARTESIAN_POINT ( 'NONE',  ( -18.82836516733858900, -7.492696928432808434, 70.47793897115684558 ) ) ;
#36309 = AXIS2_PLACEMENT_3D ( 'NONE', #44411, #25930, #48320 ) ;
#36310 = DIRECTION ( 'NONE',  ( 0.5097212845717490337, -0.8603395911234853477, 0.000000000000000000 ) ) ;
#36311 = CARTESIAN_POINT ( 'NONE',  ( -17.43166586245951422, -7.359124596637800053, 67.13544155391683432 ) ) ;
#36312 = DIRECTION ( 'NONE',  ( -0.7847243476406478013, -0.6198448985189424221, 4.433022207822356401E-08 ) ) ;
#36313 = VERTEX_POINT ( 'NONE', #689 ) ;
#36314 = VERTEX_POINT ( 'NONE', #8562 ) ;
#36315 = CARTESIAN_POINT ( 'NONE',  ( -18.89909385650551599, -8.114302828567740988, 52.18300498402516041 ) ) ;
#36316 = ADVANCED_FACE ( 'NONE', ( #23830 ), #975, .T. ) ;
#36317 = CARTESIAN_POINT ( 'NONE',  ( 18.46573386768564973, 0.6667653706753842169, 50.27657325150214973 ) ) ;
#36318 = CARTESIAN_POINT ( 'NONE',  ( -21.84079957929829874, -9.314189696129254514, 63.19153755727187161 ) ) ;
#36319 =( BOUNDED_CURVE ( )  B_SPLINE_CURVE ( 3, ( #1844, #39998, #32832, #2324 ),
 .UNSPECIFIED., .F., .F. ) 
 B_SPLINE_CURVE_WITH_KNOTS ( ( 4, 4 ),
 ( 0.000000000000000000, 0.4074455897393609582 ),
 .UNSPECIFIED. ) 
 CURVE ( )  GEOMETRIC_REPRESENTATION_ITEM ( )  RATIONAL_B_SPLINE_CURVE ( ( 1.000000000000000000, 0.4567392136813415160, 0.3561768502900338196, 0.6983129098260768552 ) ) 
 REPRESENTATION_ITEM ( '' )  );
#36320 = CARTESIAN_POINT ( 'NONE',  ( -18.73034385650551670, -9.794322478646142471, 51.19202720610083901 ) ) ;
#36321 = B_SPLINE_CURVE_WITH_KNOTS ( 'NONE', 1,
 ( #42684, #35271 ),
 .UNSPECIFIED., .F., .F.,
 ( 2, 2 ),
 ( 0.000000000000000000, 1.000000000000000000 ),
 .UNSPECIFIED. ) ;
#36322 = ADVANCED_FACE ( 'NONE', ( #38329 ), #34650, .T. ) ;
#36324 = ORIENTED_EDGE ( 'NONE', *, *, #9343, .T. ) ;
#36323 = EDGE_CURVE ( 'NONE', #42514, #1374, #45989, .T. ) ;
#36325 = CARTESIAN_POINT ( 'NONE',  ( -10.99490523303392742, -17.71099535734608210, 68.09721976853542458 ) ) ;
#36326 = EDGE_CURVE ( 'NONE', #33012, #15747, #41231, .T. ) ;
#36327 = CIRCLE ( 'NONE', #23778, 2.000000000000000000 ) ;
#36328 = CARTESIAN_POINT ( 'NONE',  ( -46.92409385541305511, -17.80920654474410370, 61.49999999999999289 ) ) ;
#36329 = EDGE_CURVE ( 'NONE', #16401, #36429, #11404, .T. ) ;
#36330 = ORIENTED_EDGE ( 'NONE', *, *, #15512, .F. ) ;
#36331 = DIRECTION ( 'NONE',  ( -3.071710424422018668E-17, 6.404604876783312462E-16, 1.000000000000000000 ) ) ;
#36332 =( BOUNDED_CURVE ( )  B_SPLINE_CURVE ( 3, ( #12754, #28262, #32202, #16676 ),
 .UNSPECIFIED., .F., .F. ) 
 B_SPLINE_CURVE_WITH_KNOTS ( ( 4, 4 ),
 ( 0.5000000000000000000, 0.9074455897393691739 ),
 .UNSPECIFIED. ) 
 CURVE ( )  GEOMETRIC_REPRESENTATION_ITEM ( )  RATIONAL_B_SPLINE_CURVE ( ( 1.000000000000011324, 0.4567392136813279158, 0.3561768502900207189, 0.6983129098261022794 ) ) 
 REPRESENTATION_ITEM ( '' )  );
#36333 = VERTEX_POINT ( 'NONE', #23586 ) ;
#36334 = CYLINDRICAL_SURFACE ( 'NONE', #132, 2.500000000000002220 ) ;
#36335 = CARTESIAN_POINT ( 'NONE',  ( -50.42609385541305755, -14.80920654474416764, 63.03529411764704804 ) ) ;
#36336 = CARTESIAN_POINT ( 'NONE',  ( -18.98390459359973548, -7.933620001262258192, 66.91543923465638954 ) ) ;
#36337 = EDGE_CURVE ( 'NONE', #17527, #43029, #14491, .T. ) ;
#36338 = EDGE_LOOP ( 'NONE', ( #42404, #19862 ) ) ;
#36339 = LINE ( 'NONE', #28722, #47806 ) ;
#36340 = LINE ( 'NONE', #39804, #20344 ) ;
#36341 = CARTESIAN_POINT ( 'NONE',  ( -21.06702863216100496, -20.84540773593990792, 65.86981821684420879 ) ) ;
#36342 = ORIENTED_EDGE ( 'NONE', *, *, #44993, .T. ) ;
#36343 = CARTESIAN_POINT ( 'NONE',  ( -17.42409385541305511, -14.80920654474411080, 47.99999999999997868 ) ) ;
#36344 = CARTESIAN_POINT ( 'NONE',  ( -24.43574572327428740, -14.04659777256190623, 69.53786587444344036 ) ) ;
#36345 = EDGE_LOOP ( 'NONE', ( #13064, #15319, #27324, #12057, #31070 ) ) ;
#36346 = FACE_OUTER_BOUND ( 'NONE', #14914, .T. ) ;
#36347 = CARTESIAN_POINT ( 'NONE',  ( -24.28619334359350290, -16.42731978468327014, 59.13804568661029037 ) ) ;
#36348 = ORIENTED_EDGE ( 'NONE', *, *, #1997, .F. ) ;
#36349 = CARTESIAN_POINT ( 'NONE',  ( -10.35650339757981442, -17.16777133705972602, 57.80105215977741295 ) ) ;
#36350 = CARTESIAN_POINT ( 'NONE',  ( -27.30749335439299585, -15.43885699713180770, 53.49999999999995026 ) ) ;
#36351 = CARTESIAN_POINT ( 'NONE',  ( -24.48810873059073856, -17.17637193698283582, 73.06831349224263761 ) ) ;
#36352 = CARTESIAN_POINT ( 'NONE',  ( -22.71955294612819998, -10.22924750400738070, 70.24008358658993245 ) ) ;
#36353 = VERTEX_POINT ( 'NONE', #11774 ) ;
#36354 = CARTESIAN_POINT ( 'NONE',  ( -17.42409385541299471, -14.80920654474435594, 52.02966884056656482 ) ) ;
#36355 = LINE ( 'NONE', #17148, #3814 ) ;
#36356 = CARTESIAN_POINT ( 'NONE',  ( -21.55251373718371966, -8.607551109076327478, 73.77845607332120892 ) ) ;
#36357 = ORIENTED_EDGE ( 'NONE', *, *, #32715, .F. ) ;
#36358 = CARTESIAN_POINT ( 'NONE',  ( -10.37795889460693033, -14.56696403379599403, 68.14328054657653411 ) ) ;
#36359 = CARTESIAN_POINT ( 'NONE',  ( -12.00862336911722927, -9.692924116444773475, 60.81563991731260188 ) ) ;
#36360 = ORIENTED_EDGE ( 'NONE', *, *, #32912, .F. ) ;
#36361 = VERTEX_POINT ( 'NONE', #4151 ) ;
#36362 = CARTESIAN_POINT ( 'NONE',  ( -10.66160677810301038, -13.00123309306513697, 67.73832347541063825 ) ) ;
#36363 = CARTESIAN_POINT ( 'NONE',  ( -17.03658212107600889, -14.90837637761275403, 52.02966884056655061 ) ) ;
#36364 = CARTESIAN_POINT ( 'NONE',  ( -13.92409385541305511, -10.60920654474410618, 79.49999999999998579 ) ) ;
#36365 = CARTESIAN_POINT ( 'NONE',  ( -23.81133579610617090, -11.82462377160084799, 59.77675971422009127 ) ) ;
#36366 = CARTESIAN_POINT ( 'NONE',  ( -19.45050378258324741, -7.639967419432419860, 60.13905765641194989 ) ) ;
#36367 = EDGE_CURVE ( 'NONE', #31856, #2275, #4258, .T. ) ;
#36368 = DIRECTION ( 'NONE',  ( -1.000000000000000000, 1.224646799147353207E-16, -4.267285103686820140E-17 ) ) ;
#36369 = CARTESIAN_POINT ( 'NONE',  ( -17.05328393105827089, -14.65920654474411045, 52.21286476528345588 ) ) ;
#36370 = CARTESIAN_POINT ( 'NONE',  ( -20.43185948505062299, -8.432683554863363184, 66.79576150497511833 ) ) ;
#36371 = ORIENTED_EDGE ( 'NONE', *, *, #11322, .F. ) ;
#36372 = VERTEX_POINT ( 'NONE', #4376 ) ;
#36373 = DIRECTION ( 'NONE',  ( -8.226841962295982234E-06, 2.386003339349608660E-06, 0.9999999999633130132 ) ) ;
#36374 = EDGE_CURVE ( 'NONE', #23071, #35729, #38930, .T. ) ;
#36375 = CARTESIAN_POINT ( 'NONE',  ( -18.67235195658554403, -19.33882101600501713, 49.52966884056656482 ) ) ;
#36376 = CARTESIAN_POINT ( 'NONE',  ( -19.77435985551070274, -21.87886194922281646, 65.64981515446680760 ) ) ;
#36377 = CARTESIAN_POINT ( 'NONE',  ( -18.95651257885568342, -7.518342207144577571, 67.06105106039149177 ) ) ;
#36378 = CARTESIAN_POINT ( 'NONE',  ( -20.12289019246589206, -7.865124395032225380, 73.90592041591946781 ) ) ;
#36379 = CARTESIAN_POINT ( 'NONE',  ( -20.27409385650551599, -9.792211528768504536, 50.49490371617623197 ) ) ;
#36380 = ORIENTED_EDGE ( 'NONE', *, *, #31301, .F. ) ;
#36381 = CARTESIAN_POINT ( 'NONE',  ( -12.64995474452274138, -19.99670071527213366, 68.63657438322856308 ) ) ;
#36382 = VECTOR ( 'NONE', #10207, 1000.000000000000114 ) ;
#36383 = EDGE_CURVE ( 'NONE', #11500, #32302, #25360, .T. ) ;
#36384 = CYLINDRICAL_SURFACE ( 'NONE', #1709, 1.999999999999999112 ) ;
#36385 = CARTESIAN_POINT ( 'NONE',  ( -18.12273401612753077, -22.22646211661374593, 65.46036745194116691 ) ) ;
#36386 = EDGE_CURVE ( 'NONE', #31760, #8273, #39935, .T. ) ;
#36387 = ORIENTED_EDGE ( 'NONE', *, *, #34901, .T. ) ;
#36388 = ADVANCED_FACE ( 'NONE', ( #16658 ), #38061, .T. ) ;
#36389 = CARTESIAN_POINT ( 'NONE',  ( -10.58210918802064526, -16.28842348006157081, 71.46252756767603387 ) ) ;
#36390 = CARTESIAN_POINT ( 'NONE',  ( -17.77594409791816688, -7.367433943401969998, 60.26556080592736464 ) ) ;
#36391 = DIRECTION ( 'NONE',  ( -3.071710424422018668E-17, 6.404604876783312462E-16, 1.000000000000000000 ) ) ;
#36392 = EDGE_CURVE ( 'NONE', #12228, #24038, #13188, .T. ) ;
#36393 = DIRECTION ( 'NONE',  ( 0.3926557917762825145, -0.9196855055857631189, -5.808111619717074757E-09 ) ) ;
#36394 = ORIENTED_EDGE ( 'NONE', *, *, #45968, .T. ) ;
#36395 = CARTESIAN_POINT ( 'NONE',  ( -23.01149708753333201, -19.02605167522872520, 59.16945258677317554 ) ) ;
#36396 = ORIENTED_EDGE ( 'NONE', *, *, #38450, .T. ) ;
#36397 = CARTESIAN_POINT ( 'NONE',  ( -15.09544305450467938, -21.46351983957133669, 65.40596681500470311 ) ) ;
#36398 = CARTESIAN_POINT ( 'NONE',  ( -33.52409385541305653, -25.10920654474410441, 48.79999999999998295 ) ) ;
#36399 = ORIENTED_EDGE ( 'NONE', *, *, #35505, .F. ) ;
#36400 = CARTESIAN_POINT ( 'NONE',  ( -20.39466380231803200, -8.415554760933066092, 66.78104085373595922 ) ) ;
#36401 = CARTESIAN_POINT ( 'NONE',  ( -14.11784385650551776, -9.790100578890868377, 49.79778022625163203 ) ) ;
#36402 = ORIENTED_EDGE ( 'NONE', *, *, #17029, .T. ) ;
#36403 = DIRECTION ( 'NONE',  ( -3.071710424422018668E-17, 6.404604876783312462E-16, 1.000000000000000000 ) ) ;
#36404 =( BOUNDED_CURVE ( )  B_SPLINE_CURVE ( 3, ( #1754, #24408, #28344, #20950 ),
 .UNSPECIFIED., .F., .F. ) 
 B_SPLINE_CURVE_WITH_KNOTS ( ( 4, 4 ),
 ( 0.9074455897393640669, 1.000000000000000000 ),
 .UNSPECIFIED. ) 
 CURVE ( )  GEOMETRIC_REPRESENTATION_ITEM ( )  RATIONAL_B_SPLINE_CURVE ( ( 0.6983129098260925094, 0.7760317562606977582, 0.8765941196520002920, 1.000000000000000000 ) ) 
 REPRESENTATION_ITEM ( '' )  );
#36405 = CARTESIAN_POINT ( 'NONE',  ( -19.84080129957490612, -21.85712737670714390, 65.57830891090566183 ) ) ;
#36406 = DIRECTION ( 'NONE',  ( -3.071710424422018668E-17, 6.404604876783312462E-16, 1.000000000000000000 ) ) ;
#36407 = ORIENTED_EDGE ( 'NONE', *, *, #44912, .F. ) ;
#36408 = CARTESIAN_POINT ( 'NONE',  ( -13.33151401730585306, -20.55006798877650454, 58.06122216312902395 ) ) ;
#36409 = CARTESIAN_POINT ( 'NONE',  ( -17.13503149044196405, -7.764836982087095052, 70.77563787455143540 ) ) ;
#36410 = B_SPLINE_CURVE_WITH_KNOTS ( 'NONE', 3,
 ( #42989, #1369, #12461, #9028, #24047, #31908, #27245, #15906, #42271, #1624 ),
 .UNSPECIFIED., .F., .F.,
 ( 4, 2, 2, 2, 4 ),
 ( 0.000000000000000000, 0.2500000000000000000, 0.5000000000000000000, 0.7500000000000000000, 1.000000000000000000 ),
 .UNSPECIFIED. ) ;
#36411 = CARTESIAN_POINT ( 'NONE',  ( -24.16575376147897458, -12.74704232990201547, 69.77243002240838621 ) ) ;
#36412 = DIRECTION ( 'NONE',  ( -7.166348394334737576E-06, 1.030346079289304524E-05, 0.9999999999212411117 ) ) ;
#36413 = VECTOR ( 'NONE', #34844, 1000.000000000000000 ) ;
#36414 = VERTEX_POINT ( 'NONE', #32651 ) ;
#36415 = ORIENTED_EDGE ( 'NONE', *, *, #10297, .T. ) ;
#36416 = CARTESIAN_POINT ( 'NONE',  ( -11.76162984098805708, -18.92470629761549006, 68.28977573079643548 ) ) ;
#36417 = CARTESIAN_POINT ( 'NONE',  ( -22.10677449762105340, -15.19398901379252642, 52.02966884056656482 ) ) ;
#36418 = ORIENTED_EDGE ( 'NONE', *, *, #11192, .F. ) ;
#36419 = CARTESIAN_POINT ( 'NONE',  ( -20.77205709590035454, -8.153671001013822917, 63.45088146699718834 ) ) ;
#36420 = CARTESIAN_POINT ( 'NONE',  ( -18.11159385759799179, -8.990409506049200417, 49.61344411288074951 ) ) ;
#36421 = ADVANCED_FACE ( 'NONE', ( #28720 ), #1888, .T. ) ;
#36422 = DIRECTION ( 'NONE',  ( 0.9687793358424821033, -0.2479245821708680464, 0.000000000000000000 ) ) ;
#36423 = CARTESIAN_POINT ( 'NONE',  ( -20.86860741727135959, -11.63137574808859931, 49.52966884056655772 ) ) ;
#36424 = ORIENTED_EDGE ( 'NONE', *, *, #28049, .T. ) ;
#36425 = CARTESIAN_POINT ( 'NONE',  ( -10.54479291434905797, -13.51458092965912705, 74.75105665847443959 ) ) ;
#36426 = CARTESIAN_POINT ( 'NONE',  ( -14.16498672988215191, -8.109065889264286398, 70.91612917212019340 ) ) ;
#36427 = LINE ( 'NONE', #2706, #9894 ) ;
#36428 = CARTESIAN_POINT ( 'NONE',  ( -17.42409385541299471, -14.80920654474435771, 49.52966884056655772 ) ) ;
#36429 = VERTEX_POINT ( 'NONE', #32421 ) ;
#36430 = ORIENTED_EDGE ( 'NONE', *, *, #40392, .T. ) ;
#36431 = CARTESIAN_POINT ( 'NONE',  ( -17.02294265308554344, -7.369891754266058470, 74.13831026345251018 ) ) ;
#36432 = DIRECTION ( 'NONE',  ( 0.04108628546905852136, 0.9991556020692448081, -1.019563928860402442E-16 ) ) ;
#36433 = ADVANCED_FACE ( 'NONE', ( #20369 ), #45005, .T. ) ;
#36434 = CARTESIAN_POINT ( 'NONE',  ( -10.01222935355948529, -14.05624259999535042, 61.01847049672689138 ) ) ;
#36435 = CARTESIAN_POINT ( 'NONE',  ( -11.51240771850610933, -10.27427218717217627, 71.08237763624090633 ) ) ;
#36436 = ORIENTED_EDGE ( 'NONE', *, *, #47403, .F. ) ;
#36437 = CARTESIAN_POINT ( 'NONE',  ( -24.23620318903103410, -13.19799477795856824, 59.43555865750501965 ) ) ;
#36438 = EDGE_CURVE ( 'NONE', #30553, #5535, #43011, .T. ) ;
#36439 = CARTESIAN_POINT ( 'NONE',  ( -10.89357934009856521, -11.22367372050276302, 64.19236096111531253 ) ) ;
#36440 = VECTOR ( 'NONE', #40719, 1000.000000000000114 ) ;
#36441 = ORIENTED_EDGE ( 'NONE', *, *, #1758, .F. ) ;
#36442 = CARTESIAN_POINT ( 'NONE',  ( -10.96149970135419061, -18.51576062833312974, 58.06360531077050524 ) ) ;
#36443 = EDGE_CURVE ( 'NONE', #4590, #1374, #35611, .T. ) ;
#36444 = CARTESIAN_POINT ( 'NONE',  ( -19.75127562985729313, -21.88641334670167282, 65.66474991182012388 ) ) ;
#36445 =( BOUNDED_CURVE ( )  B_SPLINE_CURVE ( 3, ( #2699, #32735, #20940, #10099 ),
 .UNSPECIFIED., .F., .F. ) 
 B_SPLINE_CURVE_WITH_KNOTS ( ( 4, 4 ),
 ( 0.9074455897393601811, 1.000000000000000000 ),
 .UNSPECIFIED. ) 
 CURVE ( )  GEOMETRIC_REPRESENTATION_ITEM ( )  RATIONAL_B_SPLINE_CURVE ( ( 0.6983129098260881795, 0.7760317562606939834, 0.8765941196519979606, 1.000000000000000000 ) ) 
 REPRESENTATION_ITEM ( '' )  );
#36446 = CARTESIAN_POINT ( 'NONE',  ( -45.94601335259982022, -14.20017296387473138, 71.05663168951065245 ) ) ;
#36447 = ORIENTED_EDGE ( 'NONE', *, *, #9932, .T. ) ;
#36448 = CARTESIAN_POINT ( 'NONE',  ( -19.81036900135710965, -9.838928235415560053, 53.88362224778186516 ) ) ;
#36449 = EDGE_LOOP ( 'NONE', ( #21431, #11540, #4260, #20634 ) ) ;
#36450 = LINE ( 'NONE', #19155, #34643 ) ;
#36451 = CARTESIAN_POINT ( 'NONE',  ( -22.56207008003183745, -19.63703213565221262, 72.92928497383269359 ) ) ;
#36452 = DIRECTION ( 'NONE',  ( 0.2479245821708705166, 0.9687793358424813261, 2.626836608334030890E-18 ) ) ;
#36453 = ORIENTED_EDGE ( 'NONE', *, *, #42489, .T. ) ;
#36454 = FACE_OUTER_BOUND ( 'NONE', #21607, .T. ) ;
#36455 = FACE_OUTER_BOUND ( 'NONE', #45837, .T. ) ;
#36456 = DIRECTION ( 'NONE',  ( 1.000000000000000000, 2.866981220435666553E-17, 0.000000000000000000 ) ) ;
#36457 = EDGE_CURVE ( 'NONE', #28688, #47772, #11844, .T. ) ;
#36458 = CARTESIAN_POINT ( 'NONE',  ( -10.77704936818085812, -17.00411804736975085, 57.70262972533568302 ) ) ;
#36459 = DIRECTION ( 'NONE',  ( 0.9687793358424817702, -0.2479245821708686570, 0.000000000000000000 ) ) ;
#36460 = CARTESIAN_POINT ( 'NONE',  ( -17.05328393105827089, -14.65920654474411045, 47.99999999999998579 ) ) ;
#36461 = EDGE_LOOP ( 'NONE', ( #17732, #44579, #2455, #42673 ) ) ;
#36463 = CARTESIAN_POINT ( 'NONE',  ( -24.87123160714014958, -14.59964084223042491, 62.89791924484052998 ) ) ;
#36462 =( BOUNDED_CURVE ( )  B_SPLINE_CURVE ( 3, ( #37565, #16070, #12391, #3364 ),
 .UNSPECIFIED., .F., .F. ) 
 B_SPLINE_CURVE_WITH_KNOTS ( ( 4, 4 ),
 ( 0.9074455897393681747, 1.000000000000000000 ),
 .UNSPECIFIED. ) 
 CURVE ( )  GEOMETRIC_REPRESENTATION_ITEM ( )  RATIONAL_B_SPLINE_CURVE ( ( 0.6983129098261009471, 0.7760317562607050856, 0.8765941196520047329, 1.000000000000000000 ) ) 
 REPRESENTATION_ITEM ( '' )  );
#36464 = EDGE_CURVE ( 'NONE', #43757, #12901, #30451, .T. ) ;
#36465 = DIRECTION ( 'NONE',  ( 0.04287186434519785205, 0.9990805789562555717, -2.806673972535357682E-09 ) ) ;
#36466 = DIRECTION ( 'NONE',  ( -0.3739781583979218116, -0.9274375111247651349, -6.296758467538796555E-09 ) ) ;
#36467 = FACE_OUTER_BOUND ( 'NONE', #42341, .T. ) ;
#36468 = DIRECTION ( 'NONE',  ( 6.885933443815673122E-06, -1.077603661396111343E-05, 0.9999999999182304089 ) ) ;
#36469 = EDGE_CURVE ( 'NONE', #45223, #3454, #41526, .T. ) ;
#36470 = CARTESIAN_POINT ( 'NONE',  ( -14.42409385650551457, -6.426201560718813433, 50.50509628382439331 ) ) ;
#36471 = ORIENTED_EDGE ( 'NONE', *, *, #38880, .T. ) ;
#36472 = ORIENTED_EDGE ( 'NONE', *, *, #6046, .F. ) ;
#36473 = DIRECTION ( 'NONE',  ( -0.2479245821708774278, -0.9687793358424795498, 0.000000000000000000 ) ) ;
#36474 = CARTESIAN_POINT ( 'NONE',  ( -22.07022430586338402, -11.86582892075562334, 53.49899999999994549 ) ) ;
#36475 = ORIENTED_EDGE ( 'NONE', *, *, #40837, .F. ) ;
#36476 = CARTESIAN_POINT ( 'NONE',  ( -20.66848101912799862, -8.549761622307149977, 60.12653141481577990 ) ) ;
#36477 = CARTESIAN_POINT ( 'NONE',  ( -42.07024770156689897, -27.10920654474410796, 65.83076923076922071 ) ) ;
#36478 = CARTESIAN_POINT ( 'NONE',  ( -23.19494370299929287, -18.77118727246694263, 65.82389430425217824 ) ) ;
#36479 = CARTESIAN_POINT ( 'NONE',  ( -13.76436681951595098, -7.422085961289871747, 53.49999999999995026 ) ) ;
#36480 = DIRECTION ( 'NONE',  ( -0.3478314405900309603, -0.9375570856950864451, 0.000000000000000000 ) ) ;
#36481 = CARTESIAN_POINT ( 'NONE',  ( -23.85820692815676480, -17.57049044119773029, 66.05430223995341521 ) ) ;
#36482 = DIRECTION ( 'NONE',  ( -0.6771828760946863035, 0.7358147540815750398, -3.419290845356464001E-09 ) ) ;
#36483 =( BOUNDED_CURVE ( )  B_SPLINE_CURVE ( 3, ( #16280, #34774, #1045, #26913 ),
 .UNSPECIFIED., .F., .F. ) 
 B_SPLINE_CURVE_WITH_KNOTS ( ( 4, 4 ),
 ( 0.9074455897393621795, 1.000000000000000000 ),
 .UNSPECIFIED. ) 
 CURVE ( )  GEOMETRIC_REPRESENTATION_ITEM ( )  RATIONAL_B_SPLINE_CURVE ( ( 0.6983129098260796308, 0.7760317562606866559, 0.8765941196519934087, 1.000000000000000000 ) ) 
 REPRESENTATION_ITEM ( '' )  );
#36484 = CARTESIAN_POINT ( 'NONE',  ( -20.49170831689750827, -8.461258797198503601, 63.59649424907591708 ) ) ;
#36485 = ORIENTED_EDGE ( 'NONE', *, *, #42074, .T. ) ;
#36486 = DIRECTION ( 'NONE',  ( 1.000000000000000000, 1.669677910507523057E-21, 6.493791346278465266E-22 ) ) ;
#36487 = CARTESIAN_POINT ( 'NONE',  ( -10.63004074901718532, -12.92571453866564646, 67.75304464120749515 ) ) ;
#36488 = LINE ( 'NONE', #14071, #42129 ) ;
#36489 = CARTESIAN_POINT ( 'NONE',  ( -24.18362101178863455, -17.94180522593430283, 59.18095321646488571 ) ) ;
#36490 = CARTESIAN_POINT ( 'NONE',  ( -24.08517543038346531, -12.49907855475201579, 73.52753481283211556 ) ) ;
#36491 = DIRECTION ( 'NONE',  ( -0.3478314405900309603, -0.9375570856950864451, 0.000000000000000000 ) ) ;
#36492 = VERTEX_POINT ( 'NONE', #19595 ) ;
#36493 = ORIENTED_EDGE ( 'NONE', *, *, #16093, .T. ) ;
#36494 = CARTESIAN_POINT ( 'NONE',  ( -17.57409385541304303, -6.859212275519751323, 50.50378509014259265 ) ) ;
#36495 = ORIENTED_EDGE ( 'NONE', *, *, #38728, .F. ) ;
#36496 = CARTESIAN_POINT ( 'NONE',  ( -13.24492651052040415, -9.193567913827360272, 63.92448906866182767 ) ) ;
#36497 = CARTESIAN_POINT ( 'NONE',  ( -11.68672781637937419, -10.05669048882576533, 67.68392176937598492 ) ) ;
#36498 = EDGE_CURVE ( 'NONE', #32446, #4358, #46578, .T. ) ;
#36499 = CARTESIAN_POINT ( 'NONE',  ( -24.59908880092032035, -12.80353012418438396, 66.49520876175452599 ) ) ;
#36500 = DIRECTION ( 'NONE',  ( 0.4846961512978548159, 0.8746825943832683414, 4.196010046976493442E-08 ) ) ;
#36501 = ORIENTED_EDGE ( 'NONE', *, *, #36262, .F. ) ;
#36502 = EDGE_CURVE ( 'NONE', #14412, #8372, #26984, .T. ) ;
#36503 = DIRECTION ( 'NONE',  ( 0.000000000000000000, 0.000000000000000000, -1.000000000000000000 ) ) ;
#36504 = PLANE ( 'NONE',  #25700 ) ;
#36505 = ORIENTED_EDGE ( 'NONE', *, *, #35921, .F. ) ;
#36506 = DIRECTION ( 'NONE',  ( -3.395770065602591412E-06, -1.105252671792169116E-06, 0.9999999999936236561 ) ) ;
#36507 = VECTOR ( 'NONE', #10020, 1000.000000000000227 ) ;
#36508 = ORIENTED_EDGE ( 'NONE', *, *, #3571, .F. ) ;
#36509 = CARTESIAN_POINT ( 'NONE',  ( -19.44142144650348314, -21.98165757830647138, 62.18158996068683564 ) ) ;
#36510 = CARTESIAN_POINT ( 'NONE',  ( -10.03904597514415009, -13.82694077737217242, 57.56329639008353638 ) ) ;
#36511 = CARTESIAN_POINT ( 'NONE',  ( -14.78754745127378634, -8.270772244812137686, 60.61996282000563241 ) ) ;
#36512 = VERTEX_POINT ( 'NONE', #41513 ) ;
#36513 = CARTESIAN_POINT ( 'NONE',  ( -17.42409385541299471, -14.80920654474435771, 49.52966884056655772 ) ) ;
#36514 = CIRCLE ( 'NONE', #10565, 5.249999999999998224 ) ;
#36515 = CARTESIAN_POINT ( 'NONE',  ( -24.46950595589296285, -14.38832865607273703, 73.26704460715303924 ) ) ;
#36516 = CARTESIAN_POINT ( 'NONE',  ( -24.86288141285521647, -20.97301237610655988, 54.50428052266514101 ) ) ;
#36517 = CARTESIAN_POINT ( 'NONE',  ( -11.04811567812601680, -17.69860408370704263, 71.56718199152911097 ) ) ;
#36518 = ORIENTED_EDGE ( 'NONE', *, *, #30628, .T. ) ;
#36519 = FACE_OUTER_BOUND ( 'NONE', #30075, .T. ) ;
#36520 = CARTESIAN_POINT ( 'NONE',  ( -17.70776835051902864, -22.25388969026799657, 58.52057945155585372 ) ) ;
#36521 = EDGE_CURVE ( 'NONE', #39153, #12742, #35749, .T. ) ;
#36522 = ADVANCED_FACE ( 'NONE', ( #45231 ), #4573, .T. ) ;
#36523 = EDGE_CURVE ( 'NONE', #10364, #17349, #888, .T. ) ;
#36524 = DIRECTION ( 'NONE',  ( -3.413470714839332458E-33, 1.190614954331866791E-16, -1.000000000000000000 ) ) ;
#36525 = EDGE_CURVE ( 'NONE', #48635, #6071, #20057, .T. ) ;
#36526 = CARTESIAN_POINT ( 'NONE',  ( -15.93106588071581697, -7.910958181831522218, 60.35595345230024833 ) ) ;
#36527 = CARTESIAN_POINT ( 'NONE',  ( -23.54569203310520464, -19.05535937789667145, 65.93894149164137275 ) ) ;
#36528 = ORIENTED_EDGE ( 'NONE', *, *, #22288, .T. ) ;
#36529 = CARTESIAN_POINT ( 'NONE',  ( -18.44790534074380517, -7.884421568168953343, 73.85566781112635226 ) ) ;
#36530 = DIRECTION ( 'NONE',  ( -3.071710424422018668E-17, 6.404604876783312462E-16, 1.000000000000000000 ) ) ;
#36531 = CARTESIAN_POINT ( 'NONE',  ( -18.20082364030551503, -7.794104720362528660, 73.99631248270939921 ) ) ;
#36532 = EDGE_LOOP ( 'NONE', ( #29841, #11603, #45158, #32545 ) ) ;
#36533 = DIRECTION ( 'NONE',  ( 0.5097212845717489227, -0.8603395911234855697, 0.000000000000000000 ) ) ;
#36534 = EDGE_LOOP ( 'NONE', ( #38554, #27328, #20081, #14262 ) ) ;
#36535 = ORIENTED_EDGE ( 'NONE', *, *, #37983, .F. ) ;
#36536 = ORIENTED_EDGE ( 'NONE', *, *, #34127, .T. ) ;
#36537 = CARTESIAN_POINT ( 'NONE',  ( -19.82413079548422274, -21.27835043604049048, 75.49999999999994316 ) ) ;
#36538 = FACE_OUTER_BOUND ( 'NONE', #259, .T. ) ;
#36539 = CARTESIAN_POINT ( 'NONE',  ( -15.81235419205221504, -7.945607373518417837, 67.42535135806457447 ) ) ;
#36540 = ORIENTED_EDGE ( 'NONE', *, *, #12934, .T. ) ;
#36541 = ORIENTED_EDGE ( 'NONE', *, *, #36652, .F. ) ;
#36542 = AXIS2_PLACEMENT_3D ( 'NONE', #42394, #8662, #22711 ) ;
#36543 = CARTESIAN_POINT ( 'NONE',  ( -18.73034385650551670, -9.794322478646142471, 51.19202720610083901 ) ) ;
#36544 = EDGE_CURVE ( 'NONE', #30644, #10107, #42065, .T. ) ;
#36545 = AXIS2_PLACEMENT_3D ( 'NONE', #19002, #11608, #26638 ) ;
#36546 = CARTESIAN_POINT ( 'NONE',  ( -10.75396668955334256, -17.10360140286105590, 64.92739389533053895 ) ) ;
#36547 = CARTESIAN_POINT ( 'NONE',  ( -10.86061992081550365, -17.24265423301508449, 61.38416481539552194 ) ) ;
#36548 = CARTESIAN_POINT ( 'NONE',  ( -17.60534385650551670, -8.801233750844183135, 48.81488406609782515 ) ) ;
#36549 = ORIENTED_EDGE ( 'NONE', *, *, #15208, .T. ) ;
#36550 = EDGE_CURVE ( 'NONE', #8569, #18139, #18206, .T. ) ;
#36551 = DIRECTION ( 'NONE',  ( 0.000000000000000000, 0.8949343913984796339, -0.4461977533473615032 ) ) ;
#36552 = EDGE_CURVE ( 'NONE', #20955, #21742, #46277, .T. ) ;
#36553 = CARTESIAN_POINT ( 'NONE',  ( -24.87417962317557496, -14.80849170857717567, 59.42795673386487465 ) ) ;
#36554 = EDGE_LOOP ( 'NONE', ( #7629, #252, #27179, #36324 ) ) ;
#36555 = CYLINDRICAL_SURFACE ( 'NONE', #22662, 0.1499999999999988565 ) ;
#36556 = ORIENTED_EDGE ( 'NONE', *, *, #3440, .F. ) ;
#36557 = CARTESIAN_POINT ( 'NONE',  ( -19.82409385541304303, -9.359200813967568422, 50.49621490985803263 ) ) ;
#36558 = CARTESIAN_POINT ( 'NONE',  ( -24.83666526594744184, -14.06169473043846629, 73.28418025887795295 ) ) ;
#36559 = CARTESIAN_POINT ( 'NONE',  ( -17.40534385541293716, -7.595227055684673267, 51.75156210489613073 ) ) ;
#36560 = ORIENTED_EDGE ( 'NONE', *, *, #35300, .F. ) ;
#36561 = CARTESIAN_POINT ( 'NONE',  ( 18.62590614458706995, 1.890747609047893185, 50.53028072113869484 ) ) ;
#36562 = CARTESIAN_POINT ( 'NONE',  ( -23.12431869989520550, -10.01221758024046338, 66.79828185159925624 ) ) ;
#36563 = CARTESIAN_POINT ( 'NONE',  ( -17.42409385541299471, -14.80920654474434883, 62.02966884056656482 ) ) ;
#36564 = ORIENTED_EDGE ( 'NONE', *, *, #12502, .F. ) ;
#36565 = DIRECTION ( 'NONE',  ( 9.352133743349324758E-06, 6.779811746737758835E-06, 0.9999999999332858103 ) ) ;
#36566 = CARTESIAN_POINT ( 'NONE',  ( -21.64297170217681554, -9.150934564753532285, 73.74561934610416358 ) ) ;
#36567 = CARTESIAN_POINT ( 'NONE',  ( -10.70629277777140942, -11.58826885910880478, 71.28135027068064744 ) ) ;
#36568 = ORIENTED_EDGE ( 'NONE', *, *, #17512, .F. ) ;
#36569 = AXIS2_PLACEMENT_3D ( 'NONE', #12347, #37714, #7954 ) ;
#36570 = CARTESIAN_POINT ( 'NONE',  ( -13.82836502510361854, -20.88256612802230450, 61.67213144371572042 ) ) ;
#36571 = VERTEX_POINT ( 'NONE', #41267 ) ;
#36572 = EDGE_CURVE ( 'NONE', #12722, #8993, #22559, .T. ) ;
#36573 = ADVANCED_FACE ( 'NONE', ( #46910 ), #24568, .T. ) ;
#36574 = FACE_OUTER_BOUND ( 'NONE', #37552, .T. ) ;
#36575 = DIRECTION ( 'NONE',  ( 0.3926557917762824590, -0.9196855055857630079, -5.808111619717073930E-09 ) ) ;
#36576 = LINE ( 'NONE', #17869, #9310 ) ;
#36577 =( REPRESENTATION_RELATIONSHIP ('NONE','NONE', #2768, #11272 ) REPRESENTATION_RELATIONSHIP_WITH_TRANSFORMATION ( #13396 )SHAPE_REPRESENTATION_RELATIONSHIP( ) );
#36578 = CARTESIAN_POINT ( 'NONE',  ( -45.37196614242555626, -14.20920654474410760, 70.56550563755274652 ) ) ;
#36579 = ORIENTED_EDGE ( 'NONE', *, *, #46781, .F. ) ;
#36580 = DIRECTION ( 'NONE',  ( -3.071710424422018668E-17, 6.404604876783312462E-16, 1.000000000000000000 ) ) ;
#36581 =( BOUNDED_CURVE ( )  B_SPLINE_CURVE ( 3, ( #32335, #43169, #35528, #24706 ),
 .UNSPECIFIED., .F., .F. ) 
 B_SPLINE_CURVE_WITH_KNOTS ( ( 4, 4 ),
 ( 0.4074455897393678416, 0.5000000000000000000 ),
 .UNSPECIFIED. ) 
 CURVE ( )  GEOMETRIC_REPRESENTATION_ITEM ( )  RATIONAL_B_SPLINE_CURVE ( ( 0.6983129098260949519, 0.7760317562607005337, 0.8765941196520024015, 1.000000000000001110 ) ) 
 REPRESENTATION_ITEM ( '' )  );
#36582 = FACE_OUTER_BOUND ( 'NONE', #39031, .T. ) ;
#36583 = CARTESIAN_POINT ( 'NONE',  ( -15.41904641700715217, -7.634001813009263060, 74.19490365927923392 ) ) ;
#36584 = ORIENTED_EDGE ( 'NONE', *, *, #39048, .F. ) ;
#36585 = CARTESIAN_POINT ( 'NONE',  ( -10.36617775085144899, -14.83726598580069300, 68.01367321887373407 ) ) ;
#36586 = EDGE_CURVE ( 'NONE', #30331, #35502, #32740, .T. ) ;
#36587 = EDGE_CURVE ( 'NONE', #115, #3383, #20834, .T. ) ;
#36588 = CYLINDRICAL_SURFACE ( 'NONE', #6270, 0.1499999999999999667 ) ;
#36589 = EDGE_LOOP ( 'NONE', ( #42451, #25492, #41888, #39597 ) ) ;
#36590 = ORIENTED_EDGE ( 'NONE', *, *, #9661, .F. ) ;
#36591 = ADVANCED_FACE ( 'NONE', ( #16615 ), #43226, .T. ) ;
#36592 = CARTESIAN_POINT ( 'NONE',  ( -41.80424091423659405, -14.90920654474421170, 67.95882352941174531 ) ) ;
#36593 = CARTESIAN_POINT ( 'NONE',  ( -13.43773910423563400, -20.62433115109003268, 58.33177939114180788 ) ) ;
#36594 = CARTESIAN_POINT ( 'NONE',  ( -11.54557276264065280, -18.70100022596745859, 65.04707046112368118 ) ) ;
#36595 = B_SPLINE_CURVE_WITH_KNOTS ( 'NONE', 1,
 ( #45937, #23780 ),
 .UNSPECIFIED., .F., .F.,
 ( 2, 2 ),
 ( 0.000000000000000000, 1.000000000000000000 ),
 .UNSPECIFIED. ) ;
#36596 = CARTESIAN_POINT ( 'NONE',  ( -12.77796340496265692, -17.75258416873320400, 54.07175714974880520 ) ) ;
#36597 =( BOUNDED_CURVE ( )  B_SPLINE_CURVE ( 3, ( #41012, #18578, #620, #37051 ),
 .UNSPECIFIED., .F., .F. ) 
 B_SPLINE_CURVE_WITH_KNOTS ( ( 4, 4 ),
 ( 1.570796326794896780, 1.780235837034217505 ),
 .UNSPECIFIED. ) 
 CURVE ( )  GEOMETRIC_REPRESENTATION_ITEM ( )  RATIONAL_B_SPLINE_CURVE ( ( 1.000000000000000000, 0.9963479302455154896, 0.9963479302455154896, 1.000000000000000000 ) ) 
 REPRESENTATION_ITEM ( '' )  );
#36598 = CARTESIAN_POINT ( 'NONE',  ( -45.92409385541306222, -14.20920654474410760, 71.05600000000001160 ) ) ;
#36599 = CARTESIAN_POINT ( 'NONE',  ( -22.06352374043166265, -8.980015506435984562, 63.37649162950052784 ) ) ;
#36600 = CARTESIAN_POINT ( 'NONE',  ( -22.73317970229575025, -20.03675580610048712, 72.83055794290764595 ) ) ;
#36601 = ORIENTED_EDGE ( 'NONE', *, *, #27763, .T. ) ;
#36602 = VERTEX_POINT ( 'NONE', #12689 ) ;
#36603 = CARTESIAN_POINT ( 'NONE',  ( -22.92319755143357085, -10.39759026177046763, 63.37185995336191979 ) ) ;
#36604 = EDGE_CURVE ( 'NONE', #14795, #12703, #34775, .T. ) ;
#36605 = B_SPLINE_CURVE_WITH_KNOTS ( 'NONE', 3,
 ( #27203, #42230, #6007, #24968, #21029, #2069, #3028, #32821, #39504, #9950 ),
 .UNSPECIFIED., .F., .F.,
 ( 4, 2, 2, 2, 4 ),
 ( 0.000000000000000000, 0.2500000000000000000, 0.5000000000000000000, 0.7500000000000000000, 1.000000000000000000 ),
 .UNSPECIFIED. ) ;
#36606 = CARTESIAN_POINT ( 'NONE',  ( -21.41863048803932656, -8.999699081277377388, 73.61600897546567523 ) ) ;
#36607 = DIRECTION ( 'NONE',  ( 3.071710424422018668E-17, -6.404604876783312462E-16, -1.000000000000000000 ) ) ;
#36608 = DIRECTION ( 'NONE',  ( -3.071710424422018668E-17, 6.404604876783312462E-16, 1.000000000000000000 ) ) ;
#36609 = DIRECTION ( 'NONE',  ( -2.699622400625883127E-06, 1.161037828378819543E-05, 0.9999999999289554964 ) ) ;
#36610 = ORIENTED_EDGE ( 'NONE', *, *, #27947, .T. ) ;
#36611 = B_SPLINE_CURVE_WITH_KNOTS ( 'NONE', 1,
 ( #6713, #20767 ),
 .UNSPECIFIED., .F., .F.,
 ( 2, 2 ),
 ( 0.000000000000000000, 1.000000000000000000 ),
 .UNSPECIFIED. ) ;
#36612 = CARTESIAN_POINT ( 'NONE',  ( -20.83659385650551599, -6.915538690918074494, 49.31353937987644542 ) ) ;
#36613 =( BOUNDED_CURVE ( )  B_SPLINE_CURVE ( 3, ( #10027, #9797, #6088, #40070 ),
 .UNSPECIFIED., .F., .F. ) 
 B_SPLINE_CURVE_WITH_KNOTS ( ( 4, 4 ),
 ( 0.4074455897393624570, 0.5000000000000000000 ),
 .UNSPECIFIED. ) 
 CURVE ( )  GEOMETRIC_REPRESENTATION_ITEM ( )  RATIONAL_B_SPLINE_CURVE ( ( 0.6983129098260902889, 0.7760317562606902086, 0.8765941196519916323, 0.9999999999999910072 ) ) 
 REPRESENTATION_ITEM ( '' )  );
#36614 = VECTOR ( 'NONE', #9463, 1000.000000000000114 ) ;
#36615 = VERTEX_POINT ( 'NONE', #42499 ) ;
#36616 = CARTESIAN_POINT ( 'NONE',  ( -12.68362485313667598, -20.02768789089244805, 68.63097676073942921 ) ) ;
#36617 = CARTESIAN_POINT ( 'NONE',  ( -11.91452160938943550, -19.82401263394628543, 58.18328287794685139 ) ) ;
#36618 = FACE_OUTER_BOUND ( 'NONE', #26289, .T. ) ;
#36619 = CARTESIAN_POINT ( 'NONE',  ( -10.44503168371052837, -15.82779754136115002, 68.39256704124431963 ) ) ;
#36620 = ORIENTED_EDGE ( 'NONE', *, *, #16330, .F. ) ;
#36621 = DIRECTION ( 'NONE',  ( -0.9990515194385546360, -0.04354378839186318767, 1.103613758316041215E-08 ) ) ;
#36622 = CARTESIAN_POINT ( 'NONE',  ( -17.84735332803204599, -7.371153730986438113, 60.19565454701680807 ) ) ;
#36623 = EDGE_CURVE ( 'NONE', #8715, #241, #19252, .T. ) ;
#36624 = LINE ( 'NONE', #13735, #10225 ) ;
#36625 = ORIENTED_EDGE ( 'NONE', *, *, #9945, .T. ) ;
#36626 = CARTESIAN_POINT ( 'NONE',  ( -14.76715853668754797, -21.76932111121406521, 61.78600440926723536 ) ) ;
#36627 = EDGE_LOOP ( 'NONE', ( #16608, #24251, #5918 ) ) ;
#36628 = CARTESIAN_POINT ( 'NONE',  ( -23.88415222675040184, -17.63235122089636775, 62.47360984996718258 ) ) ;
#36629 = CARTESIAN_POINT ( 'NONE',  ( -41.53953503188365204, -14.80920654474410725, 70.07647058823528141 ) ) ;
#36630 = ORIENTED_EDGE ( 'NONE', *, *, #1641, .F. ) ;
#36631 = EDGE_CURVE ( 'NONE', #8357, #6295, #46771, .T. ) ;
#36632 = CARTESIAN_POINT ( 'NONE',  ( -10.97888661679622047, -11.94317331668165671, 71.08860792922808969 ) ) ;
#36633 = CARTESIAN_POINT ( 'NONE',  ( -12.45502217426375680, -20.36096218193827667, 71.99308960123012469 ) ) ;
#36634 = VERTEX_POINT ( 'NONE', #4826 ) ;
#36635 = LINE ( 'NONE', #39872, #40947 ) ;
#36636 = CARTESIAN_POINT ( 'NONE',  ( -50.42609385541305755, -14.90920654474415841, 62.02941176470587692 ) ) ;
#36637 = CARTESIAN_POINT ( 'NONE',  ( -23.66263630406368534, -11.51900531544784911, 70.30699535439772774 ) ) ;
#36638 = ORIENTED_EDGE ( 'NONE', *, *, #27445, .F. ) ;
#36639 = DIRECTION ( 'NONE',  ( 0.9687793358424821033, -0.2479245821708677133, 0.000000000000000000 ) ) ;
#36640 = CIRCLE ( 'NONE', #2084, 1.350000000000004086 ) ;
#36641 = AXIS2_PLACEMENT_3D ( 'NONE', #30246, #22859, #12238 ) ;
#36642 = EDGE_CURVE ( 'NONE', #36141, #15790, #12896, .T. ) ;
#36643 = CARTESIAN_POINT ( 'NONE',  ( -11.33476867595667770, -19.10151316506851416, 68.40185013497388411 ) ) ;
#36644 = CARTESIAN_POINT ( 'NONE',  ( -23.34092642400682038, -10.28208056094584677, 59.78698708435513254 ) ) ;
#36645 = ORIENTED_EDGE ( 'NONE', *, *, #9469, .F. ) ;
#36646 = ORIENTED_EDGE ( 'NONE', *, *, #37401, .F. ) ;
#36647 = ADVANCED_FACE ( 'NONE', ( #12922 ), #16116, .T. ) ;
#36648 = CARTESIAN_POINT ( 'NONE',  ( -22.67603917253425294, -10.10156321767594179, 73.89649722025401957 ) ) ;
#36649 = CARTESIAN_POINT ( 'NONE',  ( -11.83910118423700553, -10.58927088369822300, 71.15996259575267402 ) ) ;
#36650 = CARTESIAN_POINT ( 'NONE',  ( -13.74654679279883851, -11.90422292133819582, 52.02966884056656482 ) ) ;
#36651 = CARTESIAN_POINT ( 'NONE',  ( -13.89284385759799179, -8.630756214087126565, 51.74842643355248129 ) ) ;
#36652 = EDGE_CURVE ( 'NONE', #35637, #8478, #9248, .T. ) ;
#36653 = DIRECTION ( 'NONE',  ( 0.9840843158728909135, -0.1445225939547943317, 0.1033986416233889927 ) ) ;
#36654 = DIRECTION ( 'NONE',  ( 0.2573866790907599622, 0.9663084897829603559, 6.714855467380900338E-08 ) ) ;
#36655 = CARTESIAN_POINT ( 'NONE',  ( -23.66133310609451712, -18.88359296917171903, 69.40876596050124192 ) ) ;
#36656 = CARTESIAN_POINT ( 'NONE',  ( -13.92409385541305511, -10.10920654474410618, 79.49999999999998579 ) ) ;
#36657 = EDGE_LOOP ( 'NONE', ( #41148, #47287, #34351, #36845 ) ) ;
#36658 = CARTESIAN_POINT ( 'NONE',  ( -10.57110035550071103, -13.38215360593666325, 74.97817647590578360 ) ) ;
#36659 = CARTESIAN_POINT ( 'NONE',  ( -24.87351451566537364, -14.94990356866029657, 59.42955486997114178 ) ) ;
#36660 = EDGE_CURVE ( 'NONE', #2205, #15682, #40600, .T. ) ;
#36661 = ORIENTED_EDGE ( 'NONE', *, *, #36859, .T. ) ;
#36662 = ORIENTED_EDGE ( 'NONE', *, *, #33234, .T. ) ;
#36663 = LINE ( 'NONE', #41122, #39054 ) ;
#36664 = CARTESIAN_POINT ( 'NONE',  ( -23.35152121466412467, -19.32258585407967999, 59.02264109267150616 ) ) ;
#36665 = DIRECTION ( 'NONE',  ( -2.696738946685428783E-06, -1.002714487109772720E-05, -0.9999999999460920108 ) ) ;
#36666 = EDGE_LOOP ( 'NONE', ( #16086, #3862, #47505, #45511, #10756 ) ) ;
#36667 = VECTOR ( 'NONE', #16153, 1000.000000000000114 ) ;
#36668 = CARTESIAN_POINT ( 'NONE',  ( -23.77561729583671379, -17.75197182879437463, 59.30378408728073225 ) ) ;
#36669 = ORIENTED_EDGE ( 'NONE', *, *, #4295, .F. ) ;
#36670 = CARTESIAN_POINT ( 'NONE',  ( -22.34365193135296579, -19.87012687442179981, 62.39006291346853317 ) ) ;
#36671 =( BOUNDED_CURVE ( )  B_SPLINE_CURVE ( 3, ( #37873, #4164, #19165, #3410 ),
 .UNSPECIFIED., .F., .F. ) 
 B_SPLINE_CURVE_WITH_KNOTS ( ( 4, 4 ),
 ( 6.081827386389255352, 6.484543227969919776 ),
 .UNSPECIFIED. ) 
 CURVE ( )  GEOMETRIC_REPRESENTATION_ITEM ( )  RATIONAL_B_SPLINE_CURVE ( ( 1.000000000000000000, 0.9865305980755139093, 0.9865305980755139093, 1.000000000000000000 ) ) 
 REPRESENTATION_ITEM ( '' )  );
#36672 = VECTOR ( 'NONE', #36331, 1000.000000000000000 ) ;
#36673 = CARTESIAN_POINT ( 'NONE',  ( -24.87289997924709439, -14.67112824012948202, 62.82801159608117558 ) ) ;
#36674 = CARTESIAN_POINT ( 'NONE',  ( -19.83890857264518104, -18.82566669410956806, 52.02966884056656482 ) ) ;
#36675 = ADVANCED_FACE ( 'NONE', ( #47406 ), #39655, .T. ) ;
#36676 = ORIENTED_EDGE ( 'NONE', *, *, #41520, .T. ) ;
#36677 = CARTESIAN_POINT ( 'NONE',  ( -20.47136568995129480, -10.23054578351414001, 53.49999999999995026 ) ) ;
#36678 = VERTEX_POINT ( 'NONE', #14109 ) ;
#36679 = DIRECTION ( 'NONE',  ( 0.9687793358424821033, -0.2479245821708680464, 0.000000000000000000 ) ) ;
#36680 = CARTESIAN_POINT ( 'NONE',  ( -17.42409385541300892, -14.80920654474439324, 77.49999999999994316 ) ) ;
#36681 = VERTEX_POINT ( 'NONE', #14582 ) ;
#36682 = CARTESIAN_POINT ( 'NONE',  ( -13.17762867948185601, -11.72213130924974500, 52.02966884056656482 ) ) ;
#36683 = CARTESIAN_POINT ( 'NONE',  ( -19.42896492416523913, -21.56812594671148275, 61.99503644571810668 ) ) ;
#36684 = FACE_OUTER_BOUND ( 'NONE', #25788, .T. ) ;
#36685 = DIRECTION ( 'NONE',  ( 0.000000000000000000, 0.007114381193220334181, -0.9999746924698833528 ) ) ;
#36686 = DIRECTION ( 'NONE',  ( 1.143861049860740968E-05, -2.837703139598260652E-06, 0.9999999999305527743 ) ) ;
#36687 = ORIENTED_EDGE ( 'NONE', *, *, #45166, .T. ) ;
#36688 = CARTESIAN_POINT ( 'NONE',  ( -24.87090184113336733, -14.58551080922006271, 62.85150006646590981 ) ) ;
#36689 = CARTESIAN_POINT ( 'NONE',  ( -9.995738364564658696, -14.24060042610175358, 64.50308557176904856 ) ) ;
#36690 = CARTESIAN_POINT ( 'NONE',  ( -14.47983227664519212, -7.965588925009814858, 63.90483403727078837 ) ) ;
#36691 = CARTESIAN_POINT ( 'NONE',  ( -13.12613380977788147, -20.89454282643029259, 58.16154686733092660 ) ) ;
#36692 = CARTESIAN_POINT ( 'NONE',  ( -16.16221656818315466, -22.15164012088281709, 58.32939616168999208 ) ) ;
#36693 = CARTESIAN_POINT ( 'NONE',  ( -24.21189024148803171, -13.09820213895421759, 62.83264126992417431 ) ) ;
#36694 = ORIENTED_EDGE ( 'NONE', *, *, #8938, .F. ) ;
#36695 = VERTEX_POINT ( 'NONE', #9967 ) ;
#36696 = EDGE_CURVE ( 'NONE', #24126, #41453, #40477, .T. ) ;
#36697 = DIRECTION ( 'NONE',  ( -1.000000000000000000, -1.669677910507523057E-21, -6.493791346278465266E-22 ) ) ;
#36698 = CARTESIAN_POINT ( 'NONE',  ( -20.67810541806404956, -8.031554304750532225, 54.02312124697527196 ) ) ;
#36699 = ORIENTED_EDGE ( 'NONE', *, *, #24832, .T. ) ;
#36701 = DIRECTION ( 'NONE',  ( -0.2479245821708778996, -0.9687793358424794388, 0.000000000000000000 ) ) ;
#36700 = CARTESIAN_POINT ( 'NONE',  ( -23.96044199021409327, -11.23292130238350772, 66.53559200982742539 ) ) ;
#36702 = DIRECTION ( 'NONE',  ( 1.927470528863184130E-16, 1.434740771370715221E-29, -1.000000000000000000 ) ) ;
#36703 = CARTESIAN_POINT ( 'NONE',  ( -10.27345454978659944, -12.71824136398891980, 64.45331520391344782 ) ) ;
#36704 = ADVANCED_FACE ( 'NONE', ( #29646 ), #6026, .T. ) ;
#36705 = CARTESIAN_POINT ( 'NONE',  ( -14.67242798431547968, -21.73322265534233111, 58.27962637798393786 ) ) ;
#36706 = DIRECTION ( 'NONE',  ( -5.731567514496413899E-31, -1.020425574103664789E-16, -1.000000000000000000 ) ) ;
#36707 = CARTESIAN_POINT ( 'NONE',  ( -12.12013830951134885, -9.577504261232970606, 57.18911913778111256 ) ) ;
#36708 = AXIS2_PLACEMENT_3D ( 'NONE', #27481, #27242, #11989 ) ;
#36709 = CARTESIAN_POINT ( 'NONE',  ( -11.44360937317491711, -19.25177985856723595, 71.78662246600895003 ) ) ;
#36710 = AXIS2_PLACEMENT_3D ( 'NONE', #5663, #40345, #25567 ) ;
#36711 = EDGE_CURVE ( 'NONE', #44664, #47803, #16045, .T. ) ;
#36712 = CARTESIAN_POINT ( 'NONE',  ( -23.69410982483307038, -17.92519756231842720, 59.11451459836140288 ) ) ;
#36713 = VERTEX_POINT ( 'NONE', #43961 ) ;
#36714 = FACE_OUTER_BOUND ( 'NONE', #25246, .T. ) ;
#36715 = CARTESIAN_POINT ( 'NONE',  ( -13.18904211892902367, -11.30002761096173280, 53.49899999999994549 ) ) ;
#36716 = AXIS2_PLACEMENT_3D ( 'NONE', #7781, #22800, #4088 ) ;
#36717 = CARTESIAN_POINT ( 'NONE',  ( -24.26595340233995302, -13.32969406988797623, 59.36267925071750540 ) ) ;
#36718 = CARTESIAN_POINT ( 'NONE',  ( -21.08710664733760609, -20.77481365697375182, 69.33833681463573839 ) ) ;
#36719 = ADVANCED_FACE ( 'NONE', ( #18298 ), #33069, .T. ) ;
#36720 = CARTESIAN_POINT ( 'NONE',  ( -17.42409385541300182, -14.80920654474440745, 52.02966884056655061 ) ) ;
#36721 = DIRECTION ( 'NONE',  ( 3.071710424422018668E-17, -6.404604876783312462E-16, -1.000000000000000000 ) ) ;
#36722 = EDGE_CURVE ( 'NONE', #35477, #21919, #21102, .T. ) ;
#36723 = ORIENTED_EDGE ( 'NONE', *, *, #41377, .T. ) ;
#36724 = ORIENTED_EDGE ( 'NONE', *, *, #37955, .F. ) ;
#36725 = CARTESIAN_POINT ( 'NONE',  ( -18.81159385541304374, -8.990409506049200417, 49.61344411288074951 ) ) ;
#36726 = VERTEX_POINT ( 'NONE', #40421 ) ;
#36727 = CARTESIAN_POINT ( 'NONE',  ( -17.05929182965467916, -21.79975568072098469, 72.45077872430272237 ) ) ;
#36728 = CARTESIAN_POINT ( 'NONE',  ( -36.42409385541304800, -8.109206544743658540, 50.50000000000030553 ) ) ;
#36729 = AXIS2_PLACEMENT_3D ( 'NONE', #1177, #17092, #36053 ) ;
#36730 =( BOUNDED_CURVE ( )  B_SPLINE_CURVE ( 3, ( #5944, #12360, #27380, #42416 ),
 .UNSPECIFIED., .F., .F. ) 
 B_SPLINE_CURVE_WITH_KNOTS ( ( 4, 4 ),
 ( 0.000000000000000000, 0.4074455897393696735 ),
 .UNSPECIFIED. ) 
 CURVE ( )  GEOMETRIC_REPRESENTATION_ITEM ( )  RATIONAL_B_SPLINE_CURVE ( ( 1.000000000000000000, 0.4567392136813298587, 0.3561768502900295452, 0.6983129098260991707 ) ) 
 REPRESENTATION_ITEM ( '' )  );
#36731 = CARTESIAN_POINT ( 'NONE',  ( -15.43285674489986903, -7.630071079539528789, 74.21952314256675720 ) ) ;
#36732 = DIRECTION ( 'NONE',  ( -0.3964226963016469485, -0.9180681052388935948, 0.000000000000000000 ) ) ;
#36733 = ORIENTED_EDGE ( 'NONE', *, *, #305, .T. ) ;
#36734 = LINE ( 'NONE', #33789, #42598 ) ;
#36735 = ORIENTED_EDGE ( 'NONE', *, *, #5398, .F. ) ;
#36736 = CARTESIAN_POINT ( 'NONE',  ( -17.97727801652185065, -22.23869005747018335, 61.98197623854611749 ) ) ;
#36737 = EDGE_CURVE ( 'NONE', #31355, #46961, #679, .T. ) ;
#36738 =( BOUNDED_SURFACE ( )  B_SPLINE_SURFACE ( 3, 1, ( 
 ( #41425, #7717 ),
 ( #34520, #22983 ),
 ( #30858, #15303 ),
 ( #37970, #45869 ),
 ( #4256, #19266 ),
 ( #34269, #3840 ),
 ( #14151, #32876 ) ),
 .UNSPECIFIED., .T., .F., .F. ) 
 B_SPLINE_SURFACE_WITH_KNOTS ( ( 4, 3, 4 ),
 ( 2, 2 ),
 ( 0.000000000000000000, 0.5000000000000000000, 1.000000000000000000 ),
 ( 0.000000000000000000, 1.000000000000000000 ),
 .UNSPECIFIED. ) 
 GEOMETRIC_REPRESENTATION_ITEM ( )  RATIONAL_B_SPLINE_SURFACE ( (
 ( 1.000000000000000000, 1.000000000000000000),
 ( 0.3333333333333335369, 0.3333333333333330373),
 ( 0.3333333333333335369, 0.3333333333333330373),
 ( 1.000000000000000000, 1.000000000000000000),
 ( 0.3333333333333333703, 0.3333333333333333703),
 ( 0.3333333333333333703, 0.3333333333333333703),
 ( 1.000000000000000000, 1.000000000000000000) ) ) 
 REPRESENTATION_ITEM ( '' )  SURFACE ( )  );
#36739 = CARTESIAN_POINT ( 'NONE',  ( -20.55534385541303521, -8.623186033802577199, 49.24843789510464376 ) ) ;
#36740 = COLOUR_RGB ( '', 0.31764706, 0.68627451, 0.89019608) ;
#36741 = AXIS2_PLACEMENT_3D ( 'NONE', #19460, #513, #30566 ) ;
#36742 = EDGE_LOOP ( 'NONE', ( #27158, #39920, #41385, #46742, #420 ) ) ;
#36743 = CARTESIAN_POINT ( 'NONE',  ( -10.52422472645684870, -17.61911478008853749, 68.21226617000660042 ) ) ;
#36744 = CARTESIAN_POINT ( 'NONE',  ( -10.72530867274958233, -17.00760959713300480, 57.97288447305808745 ) ) ;
#36745 = CARTESIAN_POINT ( 'NONE',  ( -23.08280660609100465, -10.60377317445056811, 59.61675562601556067 ) ) ;
#36746 = VERTEX_POINT ( 'NONE', #2746 ) ;
#36747 = CARTESIAN_POINT ( 'NONE',  ( -20.12998554757678704, -7.867921253476878540, 73.91370774657193010 ) ) ;
#36748 = CARTESIAN_POINT ( 'NONE',  ( -24.82002243867330549, -13.90704071453223456, 73.23616177064057808 ) ) ;
#36749 = AXIS2_PLACEMENT_3D ( 'NONE', #30140, #22751, #11173 ) ;
#36750 = CARTESIAN_POINT ( 'NONE',  ( -24.38570565625541064, -13.64691002463509939, 59.50701104079105619 ) ) ;
#36751 = CARTESIAN_POINT ( 'NONE',  ( -22.17130319910813085, -20.55096425825585982, 58.87947600183965591 ) ) ;
#36752 = ORIENTED_EDGE ( 'NONE', *, *, #12709, .F. ) ;
#36753 = CYLINDRICAL_SURFACE ( 'NONE', #16404, 0.1499999999999990508 ) ;
#36754 = EDGE_CURVE ( 'NONE', #42831, #21817, #48259, .T. ) ;
#36755 = AXIS2_PLACEMENT_3D ( 'NONE', #42865, #24398, #9136 ) ;
#36756 = CARTESIAN_POINT ( 'NONE',  ( -42.07024770156689897, -25.10920654474410441, 65.83076923076922071 ) ) ;
#36757 = CARTESIAN_POINT ( 'NONE',  ( -23.66133370835450833, -18.88359203746988868, 69.40876704922922613 ) ) ;
#36758 = CARTESIAN_POINT ( 'NONE',  ( -14.25068826455714621, -8.513811653308138716, 70.87957628655816222 ) ) ;
#36759 = CARTESIAN_POINT ( 'NONE',  ( -24.22122181710478017, -12.92668648255967234, 62.71775301689540782 ) ) ;
#36760 = ORIENTED_EDGE ( 'NONE', *, *, #8665, .T. ) ;
#36761 = CARTESIAN_POINT ( 'NONE',  ( -10.70313322336788175, -12.85206431338615118, 64.56836087214048803 ) ) ;
#36762 = DIRECTION ( 'NONE',  ( 1.616182858256118783E-16, 0.003028072113822189229, -0.9999954153791275058 ) ) ;
#36763 = CARTESIAN_POINT ( 'NONE',  ( -10.44916039635137217, -15.83526825291551177, 64.50771589744864798 ) ) ;
#36764 = B_SPLINE_CURVE_WITH_KNOTS ( 'NONE', 1,
 ( #45525, #41824 ),
 .UNSPECIFIED., .F., .F.,
 ( 2, 2 ),
 ( 0.000000000000000000, 1.000000000000000000 ),
 .UNSPECIFIED. ) ;
#36765 = ORIENTED_EDGE ( 'NONE', *, *, #48322, .F. ) ;
#36766 = DIRECTION ( 'NONE',  ( -0.8447509909909768355, 0.5351595679979596065, 0.000000000000000000 ) ) ;
#36767 = EDGE_CURVE ( 'NONE', #18227, #15068, #24713, .T. ) ;
#36768 = VERTEX_POINT ( 'NONE', #3238 ) ;
#36769 = ORIENTED_EDGE ( 'NONE', *, *, #43177, .T. ) ;
#36770 = EDGE_LOOP ( 'NONE', ( #41491, #20628, #17564, #29817, #25820 ) ) ;
#36771 = EDGE_CURVE ( 'NONE', #24008, #19690, #17525, .T. ) ;
#36772 = AXIS2_PLACEMENT_3D ( 'NONE', #14098, #47864, #6509 ) ;
#36773 = EDGE_CURVE ( 'NONE', #18567, #27537, #4719, .T. ) ;
#36774 = CARTESIAN_POINT ( 'NONE',  ( -11.06793303470118950, -10.92167721944563397, 60.86541164553911187 ) ) ;
#36775 = VECTOR ( 'NONE', #35036, 1000.000000000000000 ) ;
#36776 = DIRECTION ( 'NONE',  ( -2.866981220435666553E-17, 1.000000000000000000, 1.190614954331866791E-16 ) ) ;
#36777 = FACE_OUTER_BOUND ( 'NONE', #10277, .T. ) ;
#36778 = AXIS2_PLACEMENT_3D ( 'NONE', #16550, #30633, #19531 ) ;
#36779 = AXIS2_PLACEMENT_3D ( 'NONE', #26075, #37368, #29765 ) ;
#36780 = VERTEX_POINT ( 'NONE', #17752 ) ;
#36781 = VERTEX_POINT ( 'NONE', #32075 ) ;
#36782 = CARTESIAN_POINT ( 'NONE',  ( -18.84284385650551386, -8.811426318492348031, 52.18089403414751359 ) ) ;
#36783 = B_SPLINE_CURVE_WITH_KNOTS ( 'NONE', 3,
 ( #2453, #46309, #24864, #5430, #32007, #39397, #20193, #12565, #35205, #20690 ),
 .UNSPECIFIED., .F., .F.,
 ( 4, 2, 2, 2, 4 ),
 ( 0.1272669073658869721, 0.2522669073439838816, 0.3772669073220807912, 0.5022669073001777562, 0.6272669072782746102 ),
 .UNSPECIFIED. ) ;
#36784 = DIRECTION ( 'NONE',  ( 1.224646799147353207E-16, 1.000000000000000000, -1.912410701131276611E-32 ) ) ;
#36785 = VECTOR ( 'NONE', #12863, 1000.000000000000000 ) ;
#36786 = CYLINDRICAL_SURFACE ( 'NONE', #23713, 1.249999999999999334 ) ;
#36787 = B_SPLINE_CURVE_WITH_KNOTS ( 'NONE', 1,
 ( #12439, #8769 ),
 .UNSPECIFIED., .F., .F.,
 ( 2, 2 ),
 ( 0.000000000000000000, 1.000000000000000000 ),
 .UNSPECIFIED. ) ;
#36789 = EDGE_CURVE ( 'NONE', #33324, #39625, #27993, .T. ) ;
#36788 = CARTESIAN_POINT ( 'NONE',  ( -17.43659385650551741, -6.915538690918075382, 49.31353937987644542 ) ) ;
#36790 = EDGE_CURVE ( 'NONE', #17249, #46845, #1891, .T. ) ;
#36791 = VERTEX_POINT ( 'NONE', #23181 ) ;
#36792 = ADVANCED_FACE ( 'NONE', ( #22442 ), #7931, .T. ) ;
#36793 = EDGE_CURVE ( 'NONE', #34024, #32237, #24241, .T. ) ;
#36794 = EDGE_CURVE ( 'NONE', #48564, #13641, #43, .T. ) ;
#36795 = DIRECTION ( 'NONE',  ( 3.020324423671394676E-15, -0.4461977533473620028, -0.8949343913984795229 ) ) ;
#36796 = CARTESIAN_POINT ( 'NONE',  ( -24.87413924702786971, -14.81707641383176721, 59.34961947317660957 ) ) ;
#36797 = CARTESIAN_POINT ( 'NONE',  ( -8.424093855413060439, -6.859206544744110623, 47.99999999999998579 ) ) ;
#36798 = ORIENTED_EDGE ( 'NONE', *, *, #48071, .F. ) ;
#36799 = CYLINDRICAL_SURFACE ( 'NONE', #43914, 0.1500000000000005218 ) ;
#36800 = ORIENTED_EDGE ( 'NONE', *, *, #32943, .F. ) ;
#36801 = CARTESIAN_POINT ( 'NONE',  ( -22.39330545970614850, -9.879000042779363611, 73.67264350515011984 ) ) ;
#36802 = B_SPLINE_CURVE_WITH_KNOTS ( 'NONE', 3,
 ( #45161, #48336, #3288, #26676, #22995, #44423, #7978, #25940, #11168, #40957 ),
 .UNSPECIFIED., .F., .F.,
 ( 4, 2, 2, 2, 4 ),
 ( 0.000000000000000000, 0.2500000000000000000, 0.5000000000000000000, 0.7500000000000000000, 1.000000000000000000 ),
 .UNSPECIFIED. ) ;
#36803 = CARTESIAN_POINT ( 'NONE',  ( -18.22959801979823879, -21.76314743224078185, 69.09898171275015955 ) ) ;
#36804 = CARTESIAN_POINT ( 'NONE',  ( -10.59051903643958958, -13.04363995460383663, 74.82250634059326444 ) ) ;
#36805 = CARTESIAN_POINT ( 'NONE',  ( -17.29284385541293645, -8.630756214087201172, 51.74842643355267313 ) ) ;
#36806 = ORIENTED_EDGE ( 'NONE', *, *, #18789, .F. ) ;
#36807 = CARTESIAN_POINT ( 'NONE',  ( -19.04074625787506037, -7.997132879027503805, 67.12901749300219478 ) ) ;
#36808 = VECTOR ( 'NONE', #9003, 1000.000000000000000 ) ;
#36809 = CARTESIAN_POINT ( 'NONE',  ( -24.21483728131241975, -11.74476288741533914, 59.62202341653743076 ) ) ;
#36810 = CARTESIAN_POINT ( 'NONE',  ( -19.37484620200115160, -7.619050568204919216, 60.14588398245204814 ) ) ;
#36811 = DIRECTION ( 'NONE',  ( -5.731567514496413899E-31, -1.020425574103664789E-16, -1.000000000000000000 ) ) ;
#36812 = ORIENTED_EDGE ( 'NONE', *, *, #13481, .F. ) ;
#36813 = CARTESIAN_POINT ( 'NONE',  ( -13.07932274695846964, -16.56597809083076100, 52.02966884056656482 ) ) ;
#36814 = CARTESIAN_POINT ( 'NONE',  ( -21.34582186320181307, -20.66775149956831115, 72.82446429489806405 ) ) ;
#36815 = AXIS2_PLACEMENT_3D ( 'NONE', #1418, #27286, #35631 ) ;
#36817 = DIRECTION ( 'NONE',  ( -3.071710424422018668E-17, 6.404604876783312462E-16, 1.000000000000000000 ) ) ;
#36816 = AXIS2_PLACEMENT_3D ( 'NONE', #31654, #46673, #43960 ) ;
#36818 = EDGE_LOOP ( 'NONE', ( #12086, #29289, #31486, #46294 ) ) ;
#36819 = CARTESIAN_POINT ( 'NONE',  ( -13.29845860553889203, -21.01266621750898267, 61.63151044148704472 ) ) ;
#36820 = ORIENTED_EDGE ( 'NONE', *, *, #1151, .T. ) ;
#36821 = CARTESIAN_POINT ( 'NONE',  ( -45.92409385541305511, -15.80920654474410725, 70.50000000000000000 ) ) ;
#36823 = EDGE_CURVE ( 'NONE', #3056, #1995, #6000, .T. ) ;
#36822 = CARTESIAN_POINT ( 'NONE',  ( -23.78500256881436314, -11.88707711785523635, 59.48235732566631384 ) ) ;
#36824 = CARTESIAN_POINT ( 'NONE',  ( -24.08517543038346531, -12.49907855475201579, 73.52753481283211556 ) ) ;
#36825 = CARTESIAN_POINT ( 'NONE',  ( -23.21026474594941291, -18.83721105783783401, 65.82949252296415921 ) ) ;
#36826 = VERTEX_POINT ( 'NONE', #4225 ) ;
#36827 = CARTESIAN_POINT ( 'NONE',  ( -22.06133437076497827, -9.563835992883470638, 59.95001055572075899 ) ) ;
#36828 = AXIS2_PLACEMENT_3D ( 'NONE', #22602, #7356, #48701 ) ;
#36829 = EDGE_LOOP ( 'NONE', ( #28658, #42887, #11903, #29505, #36760 ) ) ;
#36830 = CARTESIAN_POINT ( 'NONE',  ( -14.77006348030517380, -21.34072373105164999, 58.46058126903869834 ) ) ;
#36831 = ORIENTED_EDGE ( 'NONE', *, *, #11817, .T. ) ;
#36832 = CARTESIAN_POINT ( 'NONE',  ( -20.50876352152090121, -19.05741946913900620, 52.02966884056656482 ) ) ;
#36833 = CARTESIAN_POINT ( 'NONE',  ( -11.91307475890685552, -9.794993484201089728, 60.67262835395951015 ) ) ;
#36834 = ORIENTED_EDGE ( 'NONE', *, *, #5110, .T. ) ;
#36835 = ORIENTED_EDGE ( 'NONE', *, *, #12942, .F. ) ;
#36836 = CARTESIAN_POINT ( 'NONE',  ( -14.86359179994916246, -21.80616968373489684, 65.29251951080507865 ) ) ;
#36837 = EDGE_CURVE ( 'NONE', #1662, #15022, #3476, .T. ) ;
#36838 = CARTESIAN_POINT ( 'NONE',  ( -16.50530592306966682, -19.40475993746870387, 52.02966884056656482 ) ) ;
#36839 = CARTESIAN_POINT ( 'NONE',  ( -23.47153285936109413, -19.16039112161479352, 62.47594094552156463 ) ) ;
#36840 = FACE_OUTER_BOUND ( 'NONE', #46644, .T. ) ;
#36841 = DIRECTION ( 'NONE',  ( 1.260386242728853816E-16, 0.9975640502598247528, 0.06975647374411808599 ) ) ;
#36842 = DIRECTION ( 'NONE',  ( -0.8017593358536259096, -0.5976470257363776240, 1.209213344977627713E-07 ) ) ;
#36843 = CARTESIAN_POINT ( 'NONE',  ( -20.57278596605185683, -8.057205637650621810, 66.89608763938375091 ) ) ;
#36844 = ORIENTED_EDGE ( 'NONE', *, *, #39968, .F. ) ;
#36845 = ORIENTED_EDGE ( 'NONE', *, *, #33315, .T. ) ;
#36846 = LINE ( 'NONE', #32915, #30507 ) ;
#36847 = FACE_OUTER_BOUND ( 'NONE', #10783, .T. ) ;
#36848 = VECTOR ( 'NONE', #13268, 1000.000000000000000 ) ;
#36849 = CARTESIAN_POINT ( 'NONE',  ( -21.07890896836238781, -21.30130458668023508, 62.27504751322158683 ) ) ;
#36850 = DIRECTION ( 'NONE',  ( 0.9372362738803844406, 0.3486949482324239735, -5.386914174890154601E-09 ) ) ;
#36851 = CARTESIAN_POINT ( 'NONE',  ( -24.42398663107514523, -15.65075326911586906, 73.01775867260030850 ) ) ;
#36852 = PRODUCT_DEFINITION_FORMATION_WITH_SPECIFIED_SOURCE ( 'ANY', '', #45689, .NOT_KNOWN. ) ;
#36853 = ORIENTED_EDGE ( 'NONE', *, *, #45438, .T. ) ;
#36854 = CARTESIAN_POINT ( 'NONE',  ( -18.30534385650551954, -8.801233750844183135, 48.81488406609782515 ) ) ;
#36855 = VECTOR ( 'NONE', #4224, 1000.000000000000000 ) ;
#36856 = VECTOR ( 'NONE', #7902, 1000.000000000000114 ) ;
#36857 = ORIENTED_EDGE ( 'NONE', *, *, #9392, .F. ) ;
#36858 = EDGE_CURVE ( 'NONE', #26781, #19923, #25565, .T. ) ;
#36859 = EDGE_CURVE ( 'NONE', #24381, #23558, #23634, .T. ) ;
#36860 = CARTESIAN_POINT ( 'NONE',  ( -15.56465948913149333, -7.543361525925791788, 53.27966884056655061 ) ) ;
#36861 = CARTESIAN_POINT ( 'NONE',  ( -10.20197030601470090, -12.78660143320473175, 54.27966884056655061 ) ) ;
#36862 = DIRECTION ( 'NONE',  ( 0.9687793358424821033, -0.2479245821708680464, 0.000000000000000000 ) ) ;
#36863 = CARTESIAN_POINT ( 'NONE',  ( -18.14458250172319609, -22.22429833870308613, 65.44557911879493872 ) ) ;
#36864 = AXIS2_PLACEMENT_3D ( 'NONE', #15265, #31219, #12749 ) ;
#36865 = ORIENTED_EDGE ( 'NONE', *, *, #23010, .F. ) ;
#36866 = EDGE_CURVE ( 'NONE', #2066, #43726, #38777, .T. ) ;
#36867 = EDGE_CURVE ( 'NONE', #5915, #10474, #37636, .T. ) ;
#36868 = FACE_OUTER_BOUND ( 'NONE', #31818, .T. ) ;
#36869 = CARTESIAN_POINT ( 'NONE',  ( -24.23636277187043220, -17.82529184948975498, 62.58865552117998021 ) ) ;
#36870 = ORIENTED_EDGE ( 'NONE', *, *, #27733, .T. ) ;
#36871 = CYLINDRICAL_SURFACE ( 'NONE', #22613, 0.1500000000000060452 ) ;
#36872 =( BOUNDED_CURVE ( )  B_SPLINE_CURVE ( 3, ( #4579, #24274, #5314, #23795 ),
 .UNSPECIFIED., .F., .F. ) 
 B_SPLINE_CURVE_WITH_KNOTS ( ( 4, 4 ),
 ( 0.000000000000000000, 0.4074455897393652326 ),
 .UNSPECIFIED. ) 
 CURVE ( )  GEOMETRIC_REPRESENTATION_ITEM ( )  RATIONAL_B_SPLINE_CURVE ( ( 1.000000000000000000, 0.4567392136813419046, 0.3561768502900339861, 0.6983129098260761891 ) ) 
 REPRESENTATION_ITEM ( '' )  );
#36873 = FACE_OUTER_BOUND ( 'NONE', #31702, .T. ) ;
#36874 = ORIENTED_EDGE ( 'NONE', *, *, #35097, .F. ) ;
#36875 = DIRECTION ( 'NONE',  ( -2.083496777882594458E-06, 1.347747145367441676E-07, 0.9999999999978204102 ) ) ;
#36876 = EDGE_LOOP ( 'NONE', ( #43095, #29627, #32777, #9582, #47743 ) ) ;
#36877 = DIRECTION ( 'NONE',  ( -0.1922068328301544116, -0.9813544382196450755, 7.804899501296266931E-08 ) ) ;
#36878 = CARTESIAN_POINT ( 'NONE',  ( -17.63866254341385442, -7.362211269489866261, 63.66561597723832477 ) ) ;
#36879 = ORIENTED_EDGE ( 'NONE', *, *, #41189, .T. ) ;
#36880 = CARTESIAN_POINT ( 'NONE',  ( -22.42594789675818845, -19.77792426076253918, 69.45945937764655298 ) ) ;
#36881 = EDGE_CURVE ( 'NONE', #33555, #22004, #41154, .T. ) ;
#36882 = CARTESIAN_POINT ( 'NONE',  ( -20.57117620866707242, -8.500566317031267971, 63.31121523393445472 ) ) ;
#36883 = AXIS2_PLACEMENT_3D ( 'NONE', #10084, #44085, #25581 ) ;
#36884 = VERTEX_POINT ( 'NONE', #7436 ) ;
#36885 = CARTESIAN_POINT ( 'NONE',  ( -13.33738394060092070, -12.51528319768659436, 49.52966884056655772 ) ) ;
#36886 = CARTESIAN_POINT ( 'NONE',  ( -11.10019564437503448, -18.74767688259557730, 61.38372506178604482 ) ) ;
#36887 =( BOUNDED_CURVE ( )  B_SPLINE_CURVE ( 3, ( #21172, #43088, #24634, #39636 ),
 .UNSPECIFIED., .F., .F. ) 
 B_SPLINE_CURVE_WITH_KNOTS ( ( 4, 4 ),
 ( 0.4074455897393687853, 0.5000000000000000000 ),
 .UNSPECIFIED. ) 
 CURVE ( )  GEOMETRIC_REPRESENTATION_ITEM ( )  RATIONAL_B_SPLINE_CURVE ( ( 0.6983129098261063872, 0.7760317562606898756, 0.8765941196519819734, 0.9999999999999684697 ) ) 
 REPRESENTATION_ITEM ( '' )  );
#36888 = CARTESIAN_POINT ( 'NONE',  ( -24.86497429546398763, -14.44044012822152467, 66.28318476119724778 ) ) ;
#36889 = EDGE_LOOP ( 'NONE', ( #36026, #35669, #20968, #39546 ) ) ;
#36891 = CYLINDRICAL_SURFACE ( 'NONE', #23971, 0.1500000000000014655 ) ;
#36890 =( BOUNDED_CURVE ( )  B_SPLINE_CURVE ( 3, ( #17560, #3282, #10198, #47619 ),
 .UNSPECIFIED., .F., .F. ) 
 B_SPLINE_CURVE_WITH_KNOTS ( ( 4, 4 ),
 ( 1.570796326794896780, 1.780235837034218616 ),
 .UNSPECIFIED. ) 
 CURVE ( )  GEOMETRIC_REPRESENTATION_ITEM ( )  RATIONAL_B_SPLINE_CURVE ( ( 1.000000000000000000, 0.9963479302455153785, 0.9963479302455153785, 1.000000000000000000 ) ) 
 REPRESENTATION_ITEM ( '' )  );
#36892 = AXIS2_PLACEMENT_3D ( 'NONE', #36904, #48239, #36422 ) ;
#36893 = CIRCLE ( 'NONE', #24345, 2.000000000000001776 ) ;
#36894 = CARTESIAN_POINT ( 'NONE',  ( -11.96004319712522168, -10.43380364626374579, 67.60782902827304497 ) ) ;
#36895 = FACE_OUTER_BOUND ( 'NONE', #459, .T. ) ;
#36896 = ORIENTED_EDGE ( 'NONE', *, *, #8960, .T. ) ;
#36897 = ORIENTED_EDGE ( 'NONE', *, *, #31680, .F. ) ;
#36898 = CARTESIAN_POINT ( 'NONE',  ( -22.54258147833521875, -19.66265161326780486, 69.17418017405046271 ) ) ;
#36899 = DIRECTION ( 'NONE',  ( -1.568615307090388417E-06, -3.599470258889626763E-09, 0.9999999999987696508 ) ) ;
#36900 = CARTESIAN_POINT ( 'NONE',  ( -19.20719371956520050, -7.575738887753711737, 63.58089232527501622 ) ) ;
#36901 = AXIS2_PLACEMENT_3D ( 'NONE', #43227, #9502, #2090 ) ;
#36902 = CARTESIAN_POINT ( 'NONE',  ( -16.08659385759798965, -7.222650657624104298, 49.61879703869476543 ) ) ;
#36903 = FACE_OUTER_BOUND ( 'NONE', #1985, .T. ) ;
#36904 = CARTESIAN_POINT ( 'NONE',  ( -17.42409385541299471, -14.80920654474435771, 49.52966884056655772 ) ) ;
#36905 = CARTESIAN_POINT ( 'NONE',  ( -15.48563737764182591, -8.027819004131977465, 70.49500973495348433 ) ) ;
#36906 =( BOUNDED_CURVE ( )  B_SPLINE_CURVE ( 3, ( #43880, #26358, #41368, #26861 ),
 .UNSPECIFIED., .F., .F. ) 
 B_SPLINE_CURVE_WITH_KNOTS ( ( 4, 4 ),
 ( 0.9074455897393596260, 1.000000000000000000 ),
 .UNSPECIFIED. ) 
 CURVE ( )  GEOMETRIC_REPRESENTATION_ITEM ( )  RATIONAL_B_SPLINE_CURVE ( ( 0.6983129098260846268, 0.7760317562606909858, 0.8765941196519960732, 1.000000000000000000 ) ) 
 REPRESENTATION_ITEM ( '' )  );
#36907 = CARTESIAN_POINT ( 'NONE',  ( -16.57554889599778747, -22.21081103083016117, 65.41059783760971413 ) ) ;
#36908 = ORIENTED_EDGE ( 'NONE', *, *, #23834, .F. ) ;
#36909 = CARTESIAN_POINT ( 'NONE',  ( -10.54472383408941205, -13.51494001709767723, 74.90490956355360197 ) ) ;
#36910 = CARTESIAN_POINT ( 'NONE',  ( -17.39742520082695165, -7.759256980592265762, 67.17039592192074338 ) ) ;
#36911 = DIRECTION ( 'NONE',  ( -3.071710424422018668E-17, 6.404604876783312462E-16, 1.000000000000000000 ) ) ;
#36912 = CARTESIAN_POINT ( 'NONE',  ( -17.42409385541299471, -14.80920654474435771, 49.52966884056655772 ) ) ;
#36913 = ORIENTED_EDGE ( 'NONE', *, *, #10375, .F. ) ;
#36914 = ORIENTED_EDGE ( 'NONE', *, *, #44929, .F. ) ;
#36915 = EDGE_CURVE ( 'NONE', #20377, #7647, #28231, .T. ) ;
#36916 = CARTESIAN_POINT ( 'NONE',  ( -18.55662820153069248, -10.26160847489872374, 49.52966884056655772 ) ) ;
#36917 = CARTESIAN_POINT ( 'NONE',  ( -24.44757306576362410, -14.11227934896924374, 66.33859978849633876 ) ) ;
#36918 = VECTOR ( 'NONE', #40571, 1000.000000000000000 ) ;
#36919 = DIRECTION ( 'NONE',  ( -0.2737502900231350011, -0.9618007999124593699, 5.400150802763565900E-08 ) ) ;
#36920 = DIRECTION ( 'NONE',  ( -0.6205284308219183309, -0.7841839494287597967, -1.702810348471078804E-17 ) ) ;
#36921 = ORIENTED_EDGE ( 'NONE', *, *, #40487, .T. ) ;
#36922 = AXIS2_PLACEMENT_3D ( 'NONE', #21323, #17596, #43491 ) ;
#36923 = CARTESIAN_POINT ( 'NONE',  ( -13.60238289842205894, -8.884932333444998775, 57.26967755503795132 ) ) ;
#36924 = EDGE_CURVE ( 'NONE', #36746, #42977, #35289, .T. ) ;
#36925 = CARTESIAN_POINT ( 'NONE',  ( -12.52591726580351228, -9.195683270288645517, 74.50418291613799227 ) ) ;
#36926 = ORIENTED_EDGE ( 'NONE', *, *, #336, .F. ) ;
#36927 = ADVANCED_FACE ( 'NONE', ( #19966 ), #42380, .T. ) ;
#36928 = CARTESIAN_POINT ( 'NONE',  ( -13.71293426195967413, -21.26916566922604801, 68.64120525947689089 ) ) ;
#36929 = CARTESIAN_POINT ( 'NONE',  ( -24.87123163304818974, -14.59964195235338735, 62.89791815715346956 ) ) ;
#36930 = ADVANCED_FACE ( 'NONE', ( #4957 ), #30821, .F. ) ;
#36931 = ORIENTED_EDGE ( 'NONE', *, *, #7541, .T. ) ;
#36932 = FACE_OUTER_BOUND ( 'NONE', #33865, .T. ) ;
#36933 = VERTEX_POINT ( 'NONE', #20200 ) ;
#36934 = CARTESIAN_POINT ( 'NONE',  ( -23.78676187654788521, -10.93361199230012559, 73.54688693628270357 ) ) ;
#36935 = FACE_OUTER_BOUND ( 'NONE', #36100, .T. ) ;
#36936 = VERTEX_POINT ( 'NONE', #42631 ) ;
#36937 = CARTESIAN_POINT ( 'NONE',  ( -24.16075099676623950, -17.99041029048389717, 59.20389616614811956 ) ) ;
#36938 = LINE ( 'NONE', #32998, #4541 ) ;
#36939 = EDGE_CURVE ( 'NONE', #14865, #8232, #8649, .T. ) ;
#36940 = CARTESIAN_POINT ( 'NONE',  ( -22.27409385650551243, -9.792211528768504536, 50.49490371617623197 ) ) ;
#36941 = CARTESIAN_POINT ( 'NONE',  ( -12.21634942047498384, -14.14445252980938861, 50.77966884056655772 ) ) ;
#36942 = CARTESIAN_POINT ( 'NONE',  ( -10.76587724080305541, -16.97019452347059953, 57.98760522221959945 ) ) ;
#36943 = CARTESIAN_POINT ( 'NONE',  ( -16.50258162057404832, -20.23145840177225452, 54.07175714974879099 ) ) ;
#36944 = ORIENTED_EDGE ( 'NONE', *, *, #19563, .T. ) ;
#36945 = CARTESIAN_POINT ( 'NONE',  ( -24.87290000513101873, -14.67112934921935974, 62.82801050733710468 ) ) ;
#36946 = CARTESIAN_POINT ( 'NONE',  ( -22.98355915621633372, -9.849807724373423667, 70.11904361266189767 ) ) ;
#36947 = LINE ( 'NONE', #24924, #26596 ) ;
#36948 = DIRECTION ( 'NONE',  ( -0.8459089628457130416, -0.5333273165489313961, 7.771812504399801304E-08 ) ) ;
#36949 = CARTESIAN_POINT ( 'NONE',  ( -13.58034385650551812, -6.424090610841176385, 49.80797279389978627 ) ) ;
#36950 = ORIENTED_EDGE ( 'NONE', *, *, #7011, .F. ) ;
#36951 = ORIENTED_EDGE ( 'NONE', *, *, #7644, .T. ) ;
#36952 = VECTOR ( 'NONE', #42300, 1000.000000000000000 ) ;
#36953 = CARTESIAN_POINT ( 'NONE',  ( -11.24997143734453076, -18.22902874506724302, 61.42143955951387113 ) ) ;
#36954 = CARTESIAN_POINT ( 'NONE',  ( -21.14277848257653503, -8.274947154434103780, 53.76227901944321275 ) ) ;
#36955 = VERTEX_POINT ( 'NONE', #16498 ) ;
#36957 = DIRECTION ( 'NONE',  ( 5.410999918679618404E-17, 0.000000000000000000, 1.000000000000000000 ) ) ;
#36956 = CARTESIAN_POINT ( 'NONE',  ( -19.30128557755455532, -21.60500301973953086, 58.81035253397666196 ) ) ;
#36958 = CARTESIAN_POINT ( 'NONE',  ( -11.29272682956604967, -18.18986319395907714, 57.99641719428725395 ) ) ;
#36959 = AXIS2_PLACEMENT_3D ( 'NONE', #23405, #12077, #35196 ) ;
#36960 = CARTESIAN_POINT ( 'NONE',  ( -12.55420354710856223, -9.778633195358828800, 57.20008522322477518 ) ) ;
#36961 = DIRECTION ( 'NONE',  ( 3.413470714839332458E-33, -1.190614954331866791E-16, 1.000000000000000000 ) ) ;
#36962 = CARTESIAN_POINT ( 'NONE',  ( -24.74075702715665770, -16.21285080831185965, 62.77823949964436423 ) ) ;
#36963 = LINE ( 'NONE', #10167, #43614 ) ;
#36964 = AXIS2_PLACEMENT_3D ( 'NONE', #27494, #20352, #9522 ) ;
#36965 = CARTESIAN_POINT ( 'NONE',  ( -23.44980453451080749, -18.46889374286061525, 73.06368236440982855 ) ) ;
#36966 = DIRECTION ( 'NONE',  ( 2.231660450020913271E-16, 0.9999954153791273948, 0.003028072113822188795 ) ) ;
#36967 = ORIENTED_EDGE ( 'NONE', *, *, #25778, .F. ) ;
#36968 = DIRECTION ( 'NONE',  ( 0.1186632576870824268, -0.9929345553837299887, -6.051931680293946494E-08 ) ) ;
#36969 = LINE ( 'NONE', #36715, #22732 ) ;
#36970 = CARTESIAN_POINT ( 'NONE',  ( -15.35534385759799036, -8.623186033802571870, 49.24843789510467218 ) ) ;
#36971 = FACE_OUTER_BOUND ( 'NONE', #15422, .T. ) ;
#36972 = CARTESIAN_POINT ( 'NONE',  ( -21.28659385541298121, -7.222650657624032355, 49.61879703869470148 ) ) ;
#36973 = ADVANCED_FACE ( 'NONE', ( #12327 ), #33005, .T. ) ;
#36974 = CARTESIAN_POINT ( 'NONE',  ( -13.71293330176565384, -21.26916511146244915, 68.64120417180296840 ) ) ;
#36975 = DIRECTION ( 'NONE',  ( -1.184681380772507928E-05, -1.827615836447136132E-06, 0.9999999999281563579 ) ) ;
#36976 = ORIENTED_EDGE ( 'NONE', *, *, #45538, .T. ) ;
#36977 = ORIENTED_EDGE ( 'NONE', *, *, #30706, .T. ) ;
#36978 = CARTESIAN_POINT ( 'NONE',  ( -15.15534385541304552, -8.623186033802571870, 49.24843789510467218 ) ) ;
#36979 = ORIENTED_EDGE ( 'NONE', *, *, #18327, .T. ) ;
#36980 = EDGE_CURVE ( 'NONE', #3895, #7661, #1236, .T. ) ;
#36981 = CARTESIAN_POINT ( 'NONE',  ( -17.34602462345121410, -7.359448551298330088, 67.15893111912230040 ) ) ;
#36982 = B_SPLINE_CURVE_WITH_KNOTS ( 'NONE', 1,
 ( #21084, #36079 ),
 .UNSPECIFIED., .F., .F.,
 ( 2, 2 ),
 ( 0.000000000000000000, 1.000000000000000000 ),
 .UNSPECIFIED. ) ;
#36983 = CARTESIAN_POINT ( 'NONE',  ( -18.97210877009940688, -7.521729958488855061, 66.94425830142937173 ) ) ;
#36984 =( BOUNDED_CURVE ( )  B_SPLINE_CURVE ( 3, ( #47106, #20999, #39955, #35281 ),
 .UNSPECIFIED., .F., .F. ) 
 B_SPLINE_CURVE_WITH_KNOTS ( ( 4, 4 ),
 ( 0.9074455897393605142, 1.000000000000000000 ),
 .UNSPECIFIED. ) 
 CURVE ( )  GEOMETRIC_REPRESENTATION_ITEM ( )  RATIONAL_B_SPLINE_CURVE ( ( 0.6983129098260913992, 0.7760317562606968700, 0.8765941196519997369, 1.000000000000000000 ) ) 
 REPRESENTATION_ITEM ( '' )  );
#36985 = CARTESIAN_POINT ( 'NONE',  ( -22.75923480142028055, -10.27751027444597653, 66.84182257657300852 ) ) ;
#36986 = CARTESIAN_POINT ( 'NONE',  ( -9.975950761882481643, -15.00625170120774321, 74.91123542948268721 ) ) ;
#36987 = ORIENTED_EDGE ( 'NONE', *, *, #6979, .T. ) ;
#36988 = EDGE_CURVE ( 'NONE', #9191, #42180, #43503, .T. ) ;
#36989 = AXIS2_PLACEMENT_3D ( 'NONE', #25752, #37806, #14634 ) ;
#36990 = CARTESIAN_POINT ( 'NONE',  ( -17.42409385541300182, -14.80920654474440745, 53.27966884056655061 ) ) ;
#36991 = DIRECTION ( 'NONE',  ( -1.224646799147353207E-16, -1.000000000000000000, 1.912410701131276611E-32 ) ) ;
#36992 = ADVANCED_FACE ( 'NONE', ( #24393 ), #4454, .T. ) ;
#36993 = ORIENTED_EDGE ( 'NONE', *, *, #14251, .F. ) ;
#36994 = CARTESIAN_POINT ( 'NONE',  ( -14.83720200468841810, -10.88702015217558206, 49.52966884056655772 ) ) ;
#36995 = AXIS2_PLACEMENT_3D ( 'NONE', #680, #38089, #15190 ) ;
#36996 = CARTESIAN_POINT ( 'NONE',  ( -20.66784385541298263, -9.357632978295557180, 49.97845033065652842 ) ) ;
#36997 = ORIENTED_EDGE ( 'NONE', *, *, #15489, .T. ) ;
#36998 = ADVANCED_FACE ( 'NONE', ( #19727 ), #16006, .T. ) ;
#36999 = CYLINDRICAL_SURFACE ( 'NONE', #4014, 0.1500000000000050460 ) ;
#37000 = CARTESIAN_POINT ( 'NONE',  ( -21.23484681875272884, -20.74088929683185611, 69.33978048267414351 ) ) ;
#37001 = CARTESIAN_POINT ( 'NONE',  ( -23.34092642400682038, -10.28208056094584677, 59.78698708435513254 ) ) ;
#37002 = EDGE_LOOP ( 'NONE', ( #48227, #22478, #46829, #18130, #19644 ) ) ;
#37003 = CARTESIAN_POINT ( 'NONE',  ( -11.96697528417469236, -19.88111336767673976, 58.10399280105138331 ) ) ;
#37004 = LINE ( 'NONE', #13387, #24217 ) ;
#37005 = AXIS2_PLACEMENT_3D ( 'NONE', #3888, #15178, #42279 ) ;
#37006 = ADVANCED_FACE ( 'NONE', ( #28567 ), #10576, .T. ) ;
#37007 = CARTESIAN_POINT ( 'NONE',  ( -14.98563576580806789, -21.37212005543727855, 65.33426489834504025 ) ) ;
#37008 = CARTESIAN_POINT ( 'NONE',  ( -23.96921983750137031, -17.29140838963852289, 66.13460527988867454 ) ) ;
#37009 = VERTEX_POINT ( 'NONE', #6155 ) ;
#37010 = PLANE ( 'NONE',  #32878 ) ;
#37011 = DIRECTION ( 'NONE',  ( -0.4780674886490097197, 0.8783231047267436864, 5.292596395488306339E-08 ) ) ;
#37012 = DIRECTION ( 'NONE',  ( -7.381188794381864007E-06, -5.670466972807880762E-06, -0.9999999999566818731 ) ) ;
#37013 = DIRECTION ( 'NONE',  ( 2.210955087992717862E-06, -1.097707075699772489E-06, 0.9999999999969533260 ) ) ;
#37014 = AXIS2_PLACEMENT_3D ( 'NONE', #15135, #33598, #37538 ) ;
#37015 = ORIENTED_EDGE ( 'NONE', *, *, #30763, .T. ) ;
#37016 = CARTESIAN_POINT ( 'NONE',  ( -24.65023673758593148, -12.99629830290576038, 63.01759453279318279 ) ) ;
#37017 = CARTESIAN_POINT ( 'NONE',  ( -20.92409385541305511, -10.60920654474410618, 81.99999999999998579 ) ) ;
#37018 = ORIENTED_EDGE ( 'NONE', *, *, #27685, .F. ) ;
#37019 = CARTESIAN_POINT ( 'NONE',  ( -11.34285589096144697, -19.11310387458220816, 68.35543075210530617 ) ) ;
#37020 = DIRECTION ( 'NONE',  ( 0.3688590060343663324, -0.9294853595766526810, 9.484706316669550371E-17 ) ) ;
#37021 = EDGE_LOOP ( 'NONE', ( #48510, #13894, #40172, #40636, #8106 ) ) ;
#37022 = DIRECTION ( 'NONE',  ( -0.1240347345892086062, 1.145860353393066553E-16, -0.9922778767136676281 ) ) ;
#37023 = CIRCLE ( 'NONE', #26834, 1.249999999999999334 ) ;
#37024 = ORIENTED_EDGE ( 'NONE', *, *, #39616, .F. ) ;
#37025 = EDGE_LOOP ( 'NONE', ( #47235, #8802, #3730, #13435, #45209 ) ) ;
#37026 = ORIENTED_EDGE ( 'NONE', *, *, #45902, .T. ) ;
#37027 = CARTESIAN_POINT ( 'NONE',  ( -16.11159385650551457, -6.922745924619793101, 51.69366785382590024 ) ) ;
#37028 = CARTESIAN_POINT ( 'NONE',  ( -14.30826096781649426, -8.540783494585491908, 71.02957638424210529 ) ) ;
#37029 = CARTESIAN_POINT ( 'NONE',  ( -11.77169895589660520, -10.59578386207264700, 74.43885051664024388 ) ) ;
#37030 =( BOUNDED_CURVE ( )  B_SPLINE_CURVE ( 3, ( #26158, #33029, #40923, #18504 ),
 .UNSPECIFIED., .F., .F. ) 
 B_SPLINE_CURVE_WITH_KNOTS ( ( 4, 4 ),
 ( 0.000000000000000000, 0.4074455897393634562 ),
 .UNSPECIFIED. ) 
 CURVE ( )  GEOMETRIC_REPRESENTATION_ITEM ( )  RATIONAL_B_SPLINE_CURVE ( ( 1.000000000000000000, 0.4567392136813276937, 0.3561768502900287126, 0.6983129098261030565 ) ) 
 REPRESENTATION_ITEM ( '' )  );
#37031 = EDGE_CURVE ( 'NONE', #35003, #205, #44322, .T. ) ;
#37032 = CARTESIAN_POINT ( 'NONE',  ( -14.10256395084115866, -8.140532207465255965, 70.84462205307964666 ) ) ;
#37033 = CARTESIAN_POINT ( 'NONE',  ( -13.49267557974227394, -8.956801037788498121, 60.45422421514565059 ) ) ;
#37034 = CIRCLE ( 'NONE', #40996, 5.249999999999998224 ) ;
#37035 = ORIENTED_EDGE ( 'NONE', *, *, #31774, .F. ) ;
#37036 = ORIENTED_EDGE ( 'NONE', *, *, #30819, .T. ) ;
#37037 = CARTESIAN_POINT ( 'NONE',  ( -13.89284385650552167, -7.406986770994973490, 48.81910596585309747 ) ) ;
#37038 = CARTESIAN_POINT ( 'NONE',  ( -11.42962470904260464, -10.38539412368214521, 74.62380407152070916 ) ) ;
#37039 = VECTOR ( 'NONE', #16090, 1000.000000000000227 ) ;
#37040 = LINE ( 'NONE', #48375, #5645 ) ;
#37041 = CARTESIAN_POINT ( 'NONE',  ( -18.56159385650551741, -9.295667164867525756, 49.30633214617472504 ) ) ;
#37042 = ADVANCED_FACE ( 'NONE', ( #21654 ), #47285, .T. ) ;
#37043 =( BOUNDED_CURVE ( )  B_SPLINE_CURVE ( 3, ( #14507, #10852, #14038, #33477 ),
 .UNSPECIFIED., .F., .F. ) 
 B_SPLINE_CURVE_WITH_KNOTS ( ( 4, 4 ),
 ( 0.9074455897393643999, 1.000000000000000000 ),
 .UNSPECIFIED. ) 
 CURVE ( )  GEOMETRIC_REPRESENTATION_ITEM ( )  RATIONAL_B_SPLINE_CURVE ( ( 0.6983129098261049439, 0.7760317562607085273, 0.8765941196520068424, 1.000000000000000000 ) ) 
 REPRESENTATION_ITEM ( '' )  );
#37044 = ORIENTED_EDGE ( 'NONE', *, *, #25231, .T. ) ;
#37045 = LINE ( 'NONE', #40508, #46552 ) ;
#37046 = CIRCLE ( 'NONE', #39431, 2.500000000000002220 ) ;
#37047 = EDGE_CURVE ( 'NONE', #19438, #5607, #19279, .T. ) ;
#37048 = CARTESIAN_POINT ( 'NONE',  ( -10.49189908542464522, -16.09426454567519116, 68.26295692486267797 ) ) ;
#37049 = CARTESIAN_POINT ( 'NONE',  ( -16.26195973558533581, -21.76306465430365122, 58.57113428431811997 ) ) ;
#37050 = EDGE_LOOP ( 'NONE', ( #46694, #8539, #11986, #39434, #20820 ) ) ;
#37051 = CARTESIAN_POINT ( 'NONE',  ( -10.00368807899092971, -15.89896712085359098, 54.27966884056655061 ) ) ;
#37052 = ORIENTED_EDGE ( 'NONE', *, *, #2479, .T. ) ;
#37053 = ADVANCED_FACE ( 'NONE', ( #28802 ), #48135, .T. ) ;
#37054 = VECTOR ( 'NONE', #36432, 1000.000000000000000 ) ;
#37055 = DIRECTION ( 'NONE',  ( 0.9687793358424821033, -0.2479245821708677133, 0.000000000000000000 ) ) ;
#37056 = CARTESIAN_POINT ( 'NONE',  ( -24.83515304063678286, -14.04764234229505959, 73.23776096988058271 ) ) ;
#37057 = SURFACE_SIDE_STYLE ('',( #35906 ) ) ;
#37058 = CARTESIAN_POINT ( 'NONE',  ( -10.39648919455610709, -12.33579563135258361, 57.46710844504804072 ) ) ;
#37059 = CIRCLE ( 'NONE', #41018, 2.000000000000001776 ) ;
#37060 = ORIENTED_EDGE ( 'NONE', *, *, #32584, .T. ) ;
#37061 = CARTESIAN_POINT ( 'NONE',  ( -11.14114473067313682, -10.80566704772025233, 57.32407823191172014 ) ) ;
#37062 = CARTESIAN_POINT ( 'NONE',  ( -11.77169715766437008, -10.59578624409953207, 74.58885051661056309 ) ) ;
#37063 = EDGE_CURVE ( 'NONE', #37232, #38712, #43840, .T. ) ;
#37064 = CARTESIAN_POINT ( 'NONE',  ( -12.21606489183646715, -19.56099602313843988, 57.92682377985823194 ) ) ;
#37065 = CARTESIAN_POINT ( 'NONE',  ( -11.02242957576233451, -11.85532881267382166, 74.57312195644870201 ) ) ;
#37066 = VERTEX_POINT ( 'NONE', #6398 ) ;
#37067 = DIRECTION ( 'NONE',  ( -0.1648596854219664953, -0.9863170302304249404, 7.074492695208252801E-08 ) ) ;
#37068 = ORIENTED_EDGE ( 'NONE', *, *, #34342, .F. ) ;
#37069 = FACE_BOUND ( 'NONE', #15241, .T. ) ;
#37070 = B_SPLINE_CURVE_WITH_KNOTS ( 'NONE', 3,
 ( #32786, #2522, #29101, #28394, #9684, #2034, #9193, #47584, #24210, #20519 ),
 .UNSPECIFIED., .F., .F.,
 ( 4, 2, 2, 2, 4 ),
 ( 0.000000000000000000, 0.2500000000000000000, 0.5000000000000000000, 0.7500000000000000000, 1.000000000000000000 ),
 .UNSPECIFIED. ) ;
#37071 = ORIENTED_EDGE ( 'NONE', *, *, #32121, .T. ) ;
#37072 = CARTESIAN_POINT ( 'NONE',  ( -13.12613380977788147, -20.89454282643029259, 58.16154686733092660 ) ) ;
#37073 = CARTESIAN_POINT ( 'NONE',  ( -14.17292126938155761, -21.07377676424729884, 68.61192020317307083 ) ) ;
#37074 = DIRECTION ( 'NONE',  ( -0.1240347345892086200, 1.145860353393066553E-16, -0.9922778767136676281 ) ) ;
#37075 = EDGE_LOOP ( 'NONE', ( #36977, #12728, #45049, #17827 ) ) ;
#37076 = DIRECTION ( 'NONE',  ( 0.9968684284758859704, -0.07907803935364898784, 1.831731161803828914E-08 ) ) ;
#37077 = AXIS2_PLACEMENT_3D ( 'NONE', #9942, #1825, #24731 ) ;
#37078 = ORIENTED_EDGE ( 'NONE', *, *, #6334, .T. ) ;
#37079 = DIRECTION ( 'NONE',  ( -1.205044182522204318E-05, -2.694341353802685858E-06, -0.9999999999237636494 ) ) ;
#37081 = EDGE_CURVE ( 'NONE', #27443, #47374, #39626, .T. ) ;
#37080 = CARTESIAN_POINT ( 'NONE',  ( -15.81671074304997582, -7.936704070960259649, 74.22418700304095296 ) ) ;
#37082 = ORIENTED_EDGE ( 'NONE', *, *, #16821, .T. ) ;
#37083 = CARTESIAN_POINT ( 'NONE',  ( -10.37182134788606369, -14.70778158825885207, 67.74311464738552502 ) ) ;
#37084 = ADVANCED_FACE ( 'NONE', ( #47999 ), #2693, .T. ) ;
#37085 = CARTESIAN_POINT ( 'NONE',  ( -16.98261326800368209, -21.79527086262147861, 72.16543221550985265 ) ) ;
#37086 = EDGE_CURVE ( 'NONE', #33080, #19972, #16970, .T. ) ;
#37087 = EDGE_LOOP ( 'NONE', ( #36806, #952 ) ) ;
#37088 = ORIENTED_EDGE ( 'NONE', *, *, #41730, .F. ) ;
#37089 = DIRECTION ( 'NONE',  ( 0.9757441136919973168, 0.2189141945955502822, 0.000000000000000000 ) ) ;
#37090 = CARTESIAN_POINT ( 'NONE',  ( -20.06838235508133650, -8.265300555148282768, 66.93671294127740623 ) ) ;
#37091 = CARTESIAN_POINT ( 'NONE',  ( -20.19231670334047735, -8.325423520194950910, 70.40100341277891971 ) ) ;
#37092 = CARTESIAN_POINT ( 'NONE',  ( -10.60168030567061415, -13.23530239299793365, 74.78890765637994775 ) ) ;
#37093 = CARTESIAN_POINT ( 'NONE',  ( -50.42609385541305755, -14.80920654474412679, 59.91176470588234793 ) ) ;
#37094 = CARTESIAN_POINT ( 'NONE',  ( -14.21691894016960411, -8.585707489940052284, 74.42784435416010069 ) ) ;
#37095 = CARTESIAN_POINT ( 'NONE',  ( -14.80708969572697775, -21.78456432865329973, 61.75787710153574039 ) ) ;
#37096 = VERTEX_POINT ( 'NONE', #13274 ) ;
#37097 = ORIENTED_EDGE ( 'NONE', *, *, #39826, .F. ) ;
#37098 = LINE ( 'NONE', #7830, #9264 ) ;
#37099 = AXIS2_PLACEMENT_3D ( 'NONE', #36428, #20712, #28347 ) ;
#37100 = DIRECTION ( 'NONE',  ( 2.866981220435666553E-17, -1.000000000000000000, -1.190614954331866791E-16 ) ) ;
#37101 = CARTESIAN_POINT ( 'NONE',  ( -42.93585856129541156, -14.80920654474411613, 58.90588235294116970 ) ) ;
#37102 = DIRECTION ( 'NONE',  ( -0.8949343913984795229, -0.4461977533473618918, 4.967883834297468681E-17 ) ) ;
#37103 = VERTEX_POINT ( 'NONE', #43354 ) ;
#37104 = CARTESIAN_POINT ( 'NONE',  ( -18.02409385650551599, -6.426201560718813433, 50.50509628382439331 ) ) ;
#37105 = EDGE_LOOP ( 'NONE', ( #34862, #39680, #13469, #23357, #13699 ) ) ;
#37106 = CARTESIAN_POINT ( 'NONE',  ( -16.97946104448713101, -21.84517140583366057, 72.46543221429990922 ) ) ;
#37107 = PLANE ( 'NONE',  #5670 ) ;
#37108 = DIRECTION ( 'NONE',  ( -3.071710424422018668E-17, 6.404604876783312462E-16, 1.000000000000000000 ) ) ;
#37109 = ORIENTED_EDGE ( 'NONE', *, *, #15376, .F. ) ;
#37110 = ADVANCED_FACE ( 'NONE', ( #24871 ), #32498, .T. ) ;
#37111 = CARTESIAN_POINT ( 'NONE',  ( -24.82475127085388422, -15.66597259679895693, 73.11808347143848152 ) ) ;
#37112 = CARTESIAN_POINT ( 'NONE',  ( -21.59336496936327165, -9.186214804599407202, 66.94684602522839612 ) ) ;
#37113 = ORIENTED_EDGE ( 'NONE', *, *, #16079, .T. ) ;
#37114 = CARTESIAN_POINT ( 'NONE',  ( -17.66159697976433307, -21.85550285805611637, 58.42025434932890704 ) ) ;
#37115 = CARTESIAN_POINT ( 'NONE',  ( -10.11824970337647223, -16.26811690260224452, 71.56254994910038647 ) ) ;
#37116 = ORIENTED_EDGE ( 'NONE', *, *, #32978, .F. ) ;
#37117 = CARTESIAN_POINT ( 'NONE',  ( -24.77132058643702450, -16.04239701017138131, 66.21324923524157668 ) ) ;
#37118 = ORIENTED_EDGE ( 'NONE', *, *, #35239, .F. ) ;
#37119 = CARTESIAN_POINT ( 'NONE',  ( -24.45577199812615632, -12.20047074031916168, 54.27966884056650088 ) ) ;
#37120 = CARTESIAN_POINT ( 'NONE',  ( -11.55269001482513325, -18.62078876646939563, 65.04707126775019788 ) ) ;
#37121 = ORIENTED_EDGE ( 'NONE', *, *, #21406, .T. ) ;
#37122 = CARTESIAN_POINT ( 'NONE',  ( -13.06813783877040969, -9.265530354883374287, 67.66470656304637998 ) ) ;
#37123 = CARTESIAN_POINT ( 'NONE',  ( -20.17268404433175633, -8.371407854712250796, 70.55100341248845552 ) ) ;
#37124 = VERTEX_POINT ( 'NONE', #39642 ) ;
#37125 = DIRECTION ( 'NONE',  ( -1.070267892829395584E-05, -6.715522050485540099E-06, 0.9999999999201771850 ) ) ;
#37126 = CARTESIAN_POINT ( 'NONE',  ( -11.06712629860931152, -18.69414434431124761, 61.39215439313597500 ) ) ;
#37127 = LINE ( 'NONE', #3174, #21974 ) ;
#37128 = ORIENTED_EDGE ( 'NONE', *, *, #8088, .T. ) ;
#37129 = DIRECTION ( 'NONE',  ( 1.474291235753705251E-06, 1.298191845539703006E-06, -0.9999999999980705434 ) ) ;
#37130 = ADVANCED_FACE ( 'NONE', ( #20933 ), #35934, .T. ) ;
#37131 = PLANE ( 'NONE',  #16449 ) ;
#37132 = CARTESIAN_POINT ( 'NONE',  ( -13.16616306552584525, -16.76709000361798729, 49.52966884056655772 ) ) ;
#37133 = ADVANCED_FACE ( 'NONE', ( #7133 ), #3666, .T. ) ;
#37134 = EDGE_CURVE ( 'NONE', #4687, #9150, #22383, .T. ) ;
#37135 = EDGE_LOOP ( 'NONE', ( #47987, #8259, #39287, #23868, #3433 ) ) ;
#37136 = ORIENTED_EDGE ( 'NONE', *, *, #38457, .F. ) ;
#37137 = DIRECTION ( 'NONE',  ( -0.4749924142254752235, -0.8799898899579782219, -8.916637576350563827E-09 ) ) ;
#37138 = CARTESIAN_POINT ( 'NONE',  ( -24.31477923169101629, -16.30090137217950641, 59.40860294853779777 ) ) ;
#37139 = CYLINDRICAL_SURFACE ( 'NONE', #11542, 0.1499999999999998834 ) ;
#37140 = CARTESIAN_POINT ( 'NONE',  ( -15.86159385759799001, -7.228003583438117552, 51.38655588711986155 ) ) ;
#37141 = DIRECTION ( 'NONE',  ( 0.6990986543038555379, 0.7150252244155714809, 2.907955489811387718E-17 ) ) ;
#37142 = CARTESIAN_POINT ( 'NONE',  ( -14.11063322135152909, -21.03236308526469855, 72.21135587486895702 ) ) ;
#37143 = CARTESIAN_POINT ( 'NONE',  ( -24.37121093718953446, -17.50201705633955740, 66.05701994492248730 ) ) ;
#37144 = CARTESIAN_POINT ( 'NONE',  ( -14.69865306246719960, -8.361098061448752006, 64.07362231527311280 ) ) ;
#37145 = EDGE_LOOP ( 'NONE', ( #15488, #17687, #32625, #24417, #11330 ) ) ;
#37146 = DIRECTION ( 'NONE',  ( 1.000000000000000000, 0.000000000000000000, 8.260587980841940012E-17 ) ) ;
#37147 = DIRECTION ( 'NONE',  ( -0.1240347345892086062, 1.145860353393066553E-16, -0.9922778767136676281 ) ) ;
#37148 = CARTESIAN_POINT ( 'NONE',  ( -18.24929096724884658, -21.81104555038653103, 68.82986815895560540 ) ) ;
#37149 = CYLINDRICAL_SURFACE ( 'NONE', #24488, 0.1500000000000020206 ) ;
#37150 = ORIENTED_EDGE ( 'NONE', *, *, #48159, .T. ) ;
#37151 = EDGE_LOOP ( 'NONE', ( #32668, #7032 ) ) ;
#37152 = EDGE_CURVE ( 'NONE', #29452, #37416, #1249, .T. ) ;
#37153 = CARTESIAN_POINT ( 'NONE',  ( -17.03030002819346933, -7.369452674228779365, 74.09984905828893886 ) ) ;
#37154 = CARTESIAN_POINT ( 'NONE',  ( -18.89533436007378597, -9.769568524266553311, 50.77966884056655772 ) ) ;
#37155 = CARTESIAN_POINT ( 'NONE',  ( -15.71420658305500240, -7.965879067615756703, 74.37985862309683682 ) ) ;
#37156 = CARTESIAN_POINT ( 'NONE',  ( -23.16117746674104438, -18.90708040007733359, 62.63934749780565880 ) ) ;
#37157 =( BOUNDED_CURVE ( )  B_SPLINE_CURVE ( 3, ( #33025, #18007, #3251, #48067 ),
 .UNSPECIFIED., .F., .F. ) 
 B_SPLINE_CURVE_WITH_KNOTS ( ( 4, 4 ),
 ( 0.5000000000000000000, 0.9074455897393687298 ),
 .UNSPECIFIED. ) 
 CURVE ( )  GEOMETRIC_REPRESENTATION_ITEM ( )  RATIONAL_B_SPLINE_CURVE ( ( 0.9999999999999878986, 0.4567392136813231973, 0.3561768502900354294, 0.6983129098261112722 ) ) 
 REPRESENTATION_ITEM ( '' )  );
#37158 = ORIENTED_EDGE ( 'NONE', *, *, #21050, .F. ) ;
#37159 = CARTESIAN_POINT ( 'NONE',  ( -24.31126627854681743, -17.82450373576648417, 53.76227901944321275 ) ) ;
#37160 = CARTESIAN_POINT ( 'NONE',  ( -13.88293547364789404, -20.90532801101632643, 68.75625136993008368 ) ) ;
#37161 = ORIENTED_EDGE ( 'NONE', *, *, #40346, .T. ) ;
#37162 = LINE ( 'NONE', #44841, #38635 ) ;
#37163 = EDGE_CURVE ( 'NONE', #41134, #45644, #9868, .T. ) ;
#37164 = CARTESIAN_POINT ( 'NONE',  ( -35.32409385541306079, -6.359206544744109735, 48.79999999999998295 ) ) ;
#37165 = LINE ( 'NONE', #45326, #28102 ) ;
#37166 =( BOUNDED_CURVE ( )  B_SPLINE_CURVE ( 2, ( #6454, #21474, #15020, #33241, #44367, #2738, #21702, #37180, #41146 ),
 .UNSPECIFIED., .F., .F. ) 
 B_SPLINE_CURVE_WITH_KNOTS ( ( 3, 2, 2, 2, 3 ),
 ( 0.7916666666666667407, 0.8020833333333334814, 0.8125000000000001110, 0.8229166666666667407, 0.8333333333333334814 ),
 .UNSPECIFIED. ) 
 CURVE ( )  GEOMETRIC_REPRESENTATION_ITEM ( )  RATIONAL_B_SPLINE_CURVE ( ( 0.9999999999999992228, 0.9238795325112875156, 1.000000000000000000, 0.9238795325112867385, 1.000000000000000000, 0.9238795325112867385, 1.000000000000000000, 0.9238795325112859613, 1.000000000000000888 ) ) 
 REPRESENTATION_ITEM ( '' )  );
#37167 = ORIENTED_EDGE ( 'NONE', *, *, #7034, .T. ) ;
#37168 =( BOUNDED_SURFACE ( )  B_SPLINE_SURFACE ( 3, 1, ( 
 ( #23698, #12828 ),
 ( #38932, #20710 ),
 ( #16984, #19982 ),
 ( #12346, #16259 ),
 ( #46334, #27366 ),
 ( #1027, #5458 ),
 ( #13055, #38691 ) ),
 .UNSPECIFIED., .T., .F., .F. ) 
 B_SPLINE_SURFACE_WITH_KNOTS ( ( 4, 3, 4 ),
 ( 2, 2 ),
 ( 0.000000000000000000, 0.5000000000000000000, 1.000000000000000000 ),
 ( 0.000000000000000000, 1.000000000000000000 ),
 .UNSPECIFIED. ) 
 GEOMETRIC_REPRESENTATION_ITEM ( )  RATIONAL_B_SPLINE_SURFACE ( (
 ( 1.000000000000000000, 1.000000000000000000),
 ( 0.3333333333333335369, 0.3333333333333330373),
 ( 0.3333333333333335369, 0.3333333333333330373),
 ( 1.000000000000000000, 1.000000000000000000),
 ( 0.3333333333333333703, 0.3333333333333333703),
 ( 0.3333333333333333703, 0.3333333333333333703),
 ( 1.000000000000000000, 1.000000000000000000) ) ) 
 REPRESENTATION_ITEM ( '' )  SURFACE ( )  );
#37169 = CARTESIAN_POINT ( 'NONE',  ( -12.55411140858086760, -19.90724249994213935, 65.15202838036978505 ) ) ;
#37170 = VERTEX_POINT ( 'NONE', #14706 ) ;
#37171 = CARTESIAN_POINT ( 'NONE',  ( -10.45785868539726593, -17.45007275320745421, 64.82750577911360779 ) ) ;
#37172 = CARTESIAN_POINT ( 'NONE',  ( -23.68653687815194786, -11.57061008776568123, 66.43686604568146947 ) ) ;
#37173 = EDGE_LOOP ( 'NONE', ( #35613, #19173, #25385, #37926 ) ) ;
#37174 = CARTESIAN_POINT ( 'NONE',  ( 18.57590614458695200, 1.644564126066233145, 49.26952947973238395 ) ) ;
#37175 = CYLINDRICAL_SURFACE ( 'NONE', #16338, 0.1500000000000063782 ) ;
#37176 = CIRCLE ( 'NONE', #45076, 0.4000000000000006883 ) ;
#37177 = CARTESIAN_POINT ( 'NONE',  ( -20.41784385650551314, -9.790100578890868377, 49.79778022625163203 ) ) ;
#37178 = DIRECTION ( 'NONE',  ( 1.000000000000000000, 2.866981220435666553E-17, 0.000000000000000000 ) ) ;
#37179 = CARTESIAN_POINT ( 'NONE',  ( -10.77693834736609979, -17.00378654741047413, 57.97295180822617056 ) ) ;
#37180 = CARTESIAN_POINT ( 'NONE',  ( -13.78034385759798752, -9.360768649639306105, 51.01397948905921709 ) ) ;
#37181 = CARTESIAN_POINT ( 'NONE',  ( -27.42409385541305511, -15.80920654474410725, 63.99999999999998579 ) ) ;
#37182 = ORIENTED_EDGE ( 'NONE', *, *, #2469, .F. ) ;
#37183 = CARTESIAN_POINT ( 'NONE',  ( -16.91157668238500733, -22.24167941632281753, 72.34355973887613800 ) ) ;
#37184 =( BOUNDED_CURVE ( )  B_SPLINE_CURVE ( 3, ( #38214, #42904, #5484, #45648 ),
 .UNSPECIFIED., .F., .F. ) 
 B_SPLINE_CURVE_WITH_KNOTS ( ( 4, 4 ),
 ( 0.5000000000000000000, 0.9074455897393647330 ),
 .UNSPECIFIED. ) 
 CURVE ( )  GEOMETRIC_REPRESENTATION_ITEM ( )  RATIONAL_B_SPLINE_CURVE ( ( 1.000000000000008882, 0.4567392136813313019, 0.3561768502900237165, 0.6983129098260958401 ) ) 
 REPRESENTATION_ITEM ( '' )  );
#37185 = CARTESIAN_POINT ( 'NONE',  ( -10.38752013045322009, -14.36951432065623635, 64.67331771650336236 ) ) ;
#37186 = CARTESIAN_POINT ( 'NONE',  ( -22.93125612490430143, -9.791620008186384894, 70.17211892575356558 ) ) ;
#37187 = CARTESIAN_POINT ( 'NONE',  ( -11.93195840498443516, -10.38844327383712773, 70.98365212470247343 ) ) ;
#37188 = CARTESIAN_POINT ( 'NONE',  ( -10.78527694652531288, -12.58937498152797474, 61.09853578751868497 ) ) ;
#37189 = CARTESIAN_POINT ( 'NONE',  ( -17.05117351117937474, -7.819147136050148994, 70.68139120385312424 ) ) ;
#37190 = EDGE_CURVE ( 'NONE', #35176, #33854, #44701, .T. ) ;
#37191 = ORIENTED_EDGE ( 'NONE', *, *, #30494, .T. ) ;
#37192 = ORIENTED_EDGE ( 'NONE', *, *, #33591, .F. ) ;
#37193 = CARTESIAN_POINT ( 'NONE',  ( -9.974576530078440584, -14.71985993733158793, 71.52056861311223201 ) ) ;
#37194 = ORIENTED_EDGE ( 'NONE', *, *, #31080, .F. ) ;
#37196 = CARTESIAN_POINT ( 'NONE',  ( -14.07466585761016198, -21.01278620474601411, 72.22607682806530249 ) ) ;
#37195 = CARTESIAN_POINT ( 'NONE',  ( -19.26171524298325011, -21.61554300578126231, 58.82507358300556888 ) ) ;
#37197 = LINE ( 'NONE', #33500, #22407 ) ;
#37198 = CARTESIAN_POINT ( 'NONE',  ( -12.28060247932822691, -9.983304365141403736, 64.44402973226354447 ) ) ;
#37199 = CARTESIAN_POINT ( 'NONE',  ( -10.16748990304072464, -13.12235252378331651, 71.39323974795351546 ) ) ;
#37200 = B_SPLINE_CURVE_WITH_KNOTS ( 'NONE', 3,
 ( #22826, #15391, #7319, #22319, #33370, #23067, #3602, #18605, #37821, #14901 ),
 .UNSPECIFIED., .F., .F.,
 ( 4, 2, 2, 2, 4 ),
 ( 0.000000000000000000, 0.2500000000000000000, 0.5000000000000000000, 0.7500000000000000000, 1.000000000000000000 ),
 .UNSPECIFIED. ) ;
#37201 = FACE_BOUND ( 'NONE', #13170, .T. ) ;
#37202 = CARTESIAN_POINT ( 'NONE',  ( -10.79646186035629540, -11.40653701787342200, 67.66218675276181216 ) ) ;
#37203 = FACE_OUTER_BOUND ( 'NONE', #26748, .T. ) ;
#37204 = EDGE_CURVE ( 'NONE', #3868, #36187, #2420, .T. ) ;
#37205 = ADVANCED_FACE ( 'NONE', ( #36895 ), #16126, .T. ) ;
#37206 = CARTESIAN_POINT ( 'NONE',  ( -10.20197030601470090, -12.78660143320473352, 47.99999999999994316 ) ) ;
#37207 = VERTEX_POINT ( 'NONE', #3178 ) ;
#37208 = CARTESIAN_POINT ( 'NONE',  ( -14.04913797814320375, -8.615409903819811532, 70.93777579550457801 ) ) ;
#37209 = CARTESIAN_POINT ( 'NONE',  ( -10.52668521080748398, -13.31230368787681506, 67.89399308012602319 ) ) ;
#37210 = EDGE_CURVE ( 'NONE', #19709, #13051, #421, .T. ) ;
#37211 = CARTESIAN_POINT ( 'NONE',  ( -17.31415506352089650, -21.86632207739205569, 72.32110344861041540 ) ) ;
#37212 = EDGE_CURVE ( 'NONE', #1174, #45729, #41336, .T. ) ;
#37213 = DIRECTION ( 'NONE',  ( -0.9584484254710481377, -0.2852658684667118139, 3.516456354099036190E-08 ) ) ;
#37214 = CARTESIAN_POINT ( 'NONE',  ( -24.61605428079846547, -12.86511719609775284, 66.41751453275240635 ) ) ;
#37215 = CARTESIAN_POINT ( 'NONE',  ( -50.42609385541305755, -14.80920654474420139, 66.05294117647058272 ) ) ;
#37216 = CARTESIAN_POINT ( 'NONE',  ( -18.18338144371267617, -21.81849904615365432, 65.63060065626805795 ) ) ;
#37217 = ORIENTED_EDGE ( 'NONE', *, *, #38120, .T. ) ;
#37218 = VERTEX_POINT ( 'NONE', #33197 ) ;
#37219 = CARTESIAN_POINT ( 'NONE',  ( -14.08659385541304410, -7.222650657624104298, 49.61879703869476543 ) ) ;
#37220 = VERTEX_POINT ( 'NONE', #48475 ) ;
#37221 = B_SPLINE_CURVE_WITH_KNOTS ( 'NONE', 3,
 ( #37722, #3272, #3505, #11387, #18026, #26410, #22473, #14323, #48568, #37466 ),
 .UNSPECIFIED., .F., .F.,
 ( 4, 2, 2, 2, 4 ),
 ( 0.1272669073657611005, 0.2522669073438869036, 0.3772669073220126235, 0.5022669073001384543, 0.6272669072782641742 ),
 .UNSPECIFIED. ) ;
#37222 = ADVANCED_FACE ( 'NONE', ( #18673 ), #26320, .T. ) ;
#37223 = CARTESIAN_POINT ( 'NONE',  ( -17.02395368709362344, -21.79788336522463155, 72.16543205089590174 ) ) ;
#37224 = VECTOR ( 'NONE', #22070, 1000.000000000000000 ) ;
#37225 = CARTESIAN_POINT ( 'NONE',  ( -11.68775437312510235, -10.05546324315060858, 67.54250946422081370 ) ) ;
#37226 = B_SPLINE_CURVE_WITH_KNOTS ( 'NONE', 3,
 ( #6527, #9742, #39525, #9505, #47643, #40014, #32145, #28457, #5806, #13404 ),
 .UNSPECIFIED., .F., .F.,
 ( 4, 2, 2, 2, 4 ),
 ( 0.1272669073658128924, 0.2522669073463100209, 0.3772669073268071216, 0.5022669073073042778, 0.6272669072878014340 ),
 .UNSPECIFIED. ) ;
#37227 = CARTESIAN_POINT ( 'NONE',  ( -20.30534385759798965, -7.595227055684746986, 51.75156210489594599 ) ) ;
#37228 = CARTESIAN_POINT ( 'NONE',  ( -16.09337608010665477, -22.13948405174236811, 58.40090292489767876 ) ) ;
#37229 = ORIENTED_EDGE ( 'NONE', *, *, #38895, .F. ) ;
#37230 = FACE_OUTER_BOUND ( 'NONE', #17257, .T. ) ;
#37231 = CARTESIAN_POINT ( 'NONE',  ( -18.83586040784625126, -7.494106175837369044, 70.48572642001049360 ) ) ;
#37232 = VERTEX_POINT ( 'NONE', #33680 ) ;
#37233 = CARTESIAN_POINT ( 'NONE',  ( -23.82366785274684418, -10.99486113721019009, 73.47697904737684382 ) ) ;
#37234 = VERTEX_POINT ( 'NONE', #37629 ) ;
#37235 = DIRECTION ( 'NONE',  ( 1.000000000000000000, 1.669677910507523057E-21, 6.493791346278465266E-22 ) ) ;
#37236 = LINE ( 'NONE', #18534, #46411 ) ;
#37237 = DIRECTION ( 'NONE',  ( 0.9687793358424821033, -0.2479245821708677133, 0.000000000000000000 ) ) ;
#37238 = VERTEX_POINT ( 'NONE', #14967 ) ;
#37239 = CARTESIAN_POINT ( 'NONE',  ( -10.67250920137991521, -11.65805311173287961, 71.20205571017048385 ) ) ;
#37240 = CARTESIAN_POINT ( 'NONE',  ( -23.01899735208242248, -19.09874304491667019, 59.18410621858622278 ) ) ;
#37241 = ADVANCED_FACE ( 'NONE', ( #22149 ), #29526, .F. ) ;
#37242 = CARTESIAN_POINT ( 'NONE',  ( -14.98563567286690379, -21.37212002227751029, 65.17766890071607122 ) ) ;
#37243 = CARTESIAN_POINT ( 'NONE',  ( -21.65477688667505518, -9.232350752012335349, 66.66149992610201025 ) ) ;
#37244 = ORIENTED_EDGE ( 'NONE', *, *, #31712, .T. ) ;
#37245 = CARTESIAN_POINT ( 'NONE',  ( -11.79630000206883977, -19.05592701419838519, 71.97213747039440079 ) ) ;
#37246 = DIRECTION ( 'NONE',  ( 2.866981220435666553E-17, -1.000000000000000000, -1.190614954331866791E-16 ) ) ;
#37247 = CARTESIAN_POINT ( 'NONE',  ( -16.23116076413911557, -7.455249184188991407, 60.31533086125586607 ) ) ;
#37248 = CARTESIAN_POINT ( 'NONE',  ( -10.39060893342343839, -14.27672657784476584, 67.94980160461363994 ) ) ;
#37249 = VECTOR ( 'NONE', #27832, 1000.000000000000227 ) ;
#37250 = CARTESIAN_POINT ( 'NONE',  ( -20.83659385650551599, -6.915538690918074494, 49.31353937987644542 ) ) ;
#37251 = EDGE_CURVE ( 'NONE', #38159, #31450, #34063, .T. ) ;
#37252 = AXIS2_PLACEMENT_3D ( 'NONE', #4278, #15329, #5010 ) ;
#37253 = ORIENTED_EDGE ( 'NONE', *, *, #38937, .F. ) ;
#37254 = CARTESIAN_POINT ( 'NONE',  ( -24.25486363958986757, -13.06355980472538292, 63.11792038370487035 ) ) ;
#37255 = CYLINDRICAL_SURFACE ( 'NONE', #37533, 0.1500000000000022704 ) ;
#37256 = ORIENTED_EDGE ( 'NONE', *, *, #40704, .F. ) ;
#37257 = CARTESIAN_POINT ( 'NONE',  ( -11.29385027892729987, -19.04286830487734861, 68.33194243210506613 ) ) ;
#37258 = CARTESIAN_POINT ( 'NONE',  ( -22.60138648290591235, -10.09559422629491898, 73.59234105511633572 ) ) ;
#37259 = CARTESIAN_POINT ( 'NONE',  ( -10.57110035550071103, -13.38215360593666325, 74.97817647590578360 ) ) ;
#37260 = ORIENTED_EDGE ( 'NONE', *, *, #45027, .T. ) ;
#37261 = DIRECTION ( 'NONE',  ( 1.000000000000000000, 1.669677910507523057E-21, 6.493791346278465266E-22 ) ) ;
#37262 = FACE_OUTER_BOUND ( 'NONE', #42303, .T. ) ;
#37263 = ORIENTED_EDGE ( 'NONE', *, *, #40257, .F. ) ;
#37264 = ORIENTED_EDGE ( 'NONE', *, *, #9282, .T. ) ;
#37265 = CARTESIAN_POINT ( 'NONE',  ( -14.19909385650551847, -8.114302828567740988, 52.18300498402516041 ) ) ;
#37266 = EDGE_CURVE ( 'NONE', #11402, #978, #12973, .T. ) ;
#37267 =( BOUNDED_CURVE ( )  B_SPLINE_CURVE ( 2, ( #23707, #16270, #796, #34027, #15300, #30364, #11629, #26655, #41676 ),
 .UNSPECIFIED., .F., .F. ) 
 B_SPLINE_CURVE_WITH_KNOTS ( ( 3, 2, 2, 2, 3 ),
 ( 3.223963992799358462E-49, 0.0009834168075315858487, 0.001966833615063171697, 0.002950250422594757546, 0.003933667230126343395 ),
 .UNSPECIFIED. ) 
 CURVE ( )  GEOMETRIC_REPRESENTATION_ITEM ( )  RATIONAL_B_SPLINE_CURVE ( ( 1.000000000000000000, 0.9238795325112867385, 1.000000000000000000, 0.9238795325112867385, 1.000000000000000000, 0.9238795325112867385, 1.000000000000000000, 0.9238795325113238199, 0.9999999999999629186 ) ) 
 REPRESENTATION_ITEM ( '' )  );
#37268 = EDGE_CURVE ( 'NONE', #11974, #35003, #1125, .T. ) ;
#37269 = CARTESIAN_POINT ( 'NONE',  ( -22.78678303852979425, -9.565966637465477262, 54.27966884056655061 ) ) ;
#37270 = DIRECTION ( 'NONE',  ( 0.9687793358424817702, -0.2479245821708684905, 0.000000000000000000 ) ) ;
#37271 = CARTESIAN_POINT ( 'NONE',  ( -45.85858821786293049, -14.20920654474410760, 69.94787228701220272 ) ) ;
#37272 = CARTESIAN_POINT ( 'NONE',  ( -17.42409385541305511, -14.80920654474411080, 47.99999999999997868 ) ) ;
#37273 = ORIENTED_EDGE ( 'NONE', *, *, #14473, .T. ) ;
#37274 = VERTEX_POINT ( 'NONE', #44554 ) ;
#37275 = CARTESIAN_POINT ( 'NONE',  ( -16.36784385650551954, -6.428312510596451368, 51.20221977374900035 ) ) ;
#37276 = CARTESIAN_POINT ( 'NONE',  ( -10.02191625022346955, -15.65273779443635327, 61.15293638507743168 ) ) ;
#37277 = DIRECTION ( 'NONE',  ( -0.9848822020395749943, 0.1732254256905498002, 7.367703375004543066E-08 ) ) ;
#37278 = EDGE_CURVE ( 'NONE', #33406, #7220, #25265, .T. ) ;
#37279 = CARTESIAN_POINT ( 'NONE',  ( -14.79284385650551670, -7.406986770994973490, 48.81910596585309747 ) ) ;
#37280 = AXIS2_PLACEMENT_3D ( 'NONE', #28686, #6286, #32621 ) ;
#37281 = VERTEX_POINT ( 'NONE', #37132 ) ;
#37282 = DIRECTION ( 'NONE',  ( -0.9959323210854038599, 0.09010444948746665350, 2.601165157765156148E-08 ) ) ;
#37283 = PRODUCT_DEFINITION ( 'UNKNOWN', '', #15628, #17406 ) ;
#37284 = AXIS2_PLACEMENT_3D ( 'NONE', #9799, #29469, #18124 ) ;
#37285 = CARTESIAN_POINT ( 'NONE',  ( -22.21713244587612834, -19.98430316242970406, 69.47417961646398510 ) ) ;
#37286 = CARTESIAN_POINT ( 'NONE',  ( -11.71665266943325534, -18.96132379659194100, 64.90273906658698877 ) ) ;
#37287 = VERTEX_POINT ( 'NONE', #3420 ) ;
#37288 = CARTESIAN_POINT ( 'NONE',  ( -21.77108044372514684, -13.02615771018284363, 52.02966884056656482 ) ) ;
#37289 = ORIENTED_EDGE ( 'NONE', *, *, #32703, .T. ) ;
#37290 = CARTESIAN_POINT ( 'NONE',  ( -13.54893327507986456, -8.910214905335239521, 64.05379690000981441 ) ) ;
#37291 = FACE_OUTER_BOUND ( 'NONE', #6184, .T. ) ;
#37292 = DIRECTION ( 'NONE',  ( 0.8967515337576290602, -0.4425343904188011046, 9.546469656967254525E-09 ) ) ;
#37293 = ORIENTED_EDGE ( 'NONE', *, *, #43461, .T. ) ;
#37294 = CARTESIAN_POINT ( 'NONE',  ( -10.37840828709523322, -12.38598989307629061, 60.98508858522948373 ) ) ;
#37295 = CARTESIAN_POINT ( 'NONE',  ( -22.78745088117329942, -19.98005169855493079, 72.83738836787418336 ) ) ;
#37296 = ADVANCED_FACE ( 'NONE', ( #20088 ), #23799, .F. ) ;
#37297 = DIRECTION ( 'NONE',  ( -3.071710424422018668E-17, 6.404604876783312462E-16, 1.000000000000000000 ) ) ;
#37298 = CYLINDRICAL_SURFACE ( 'NONE', #5633, 0.1500000000000032419 ) ;
#37299 = ORIENTED_EDGE ( 'NONE', *, *, #10485, .F. ) ;
#37300 = CARTESIAN_POINT ( 'NONE',  ( -19.50174133129179666, -21.96376507711987003, 62.17316415538206087 ) ) ;
#37301 = CARTESIAN_POINT ( 'NONE',  ( -17.17470792286161441, -7.363371476440942587, 70.59012221026488021 ) ) ;
#37302 = CARTESIAN_POINT ( 'NONE',  ( -22.37985683132060188, -19.82347751554591397, 69.47417989525710880 ) ) ;
#37303 = VERTEX_POINT ( 'NONE', #1614 ) ;
#37304 = FACE_BOUND ( 'NONE', #1119, .T. ) ;
#37305 = ORIENTED_EDGE ( 'NONE', *, *, #31293, .F. ) ;
#37306 = B_SPLINE_CURVE_WITH_KNOTS ( 'NONE', 3,
 ( #10772, #40329, #18391, #29251, #29737, #25075, #13720, #2422, #40096, #17433 ),
 .UNSPECIFIED., .F., .F.,
 ( 4, 2, 2, 2, 4 ),
 ( 0.000000000000000000, 0.2500000000000000000, 0.5000000000000000000, 0.7500000000000000000, 1.000000000000000000 ),
 .UNSPECIFIED. ) ;
#37307 = CARTESIAN_POINT ( 'NONE',  ( 18.57132275349405148, 1.810087817303917657, 49.27149739157786712 ) ) ;
#37308 = DIRECTION ( 'NONE',  ( 6.516572649233546247E-06, -8.834921932032007089E-06, -0.9999999999397393147 ) ) ;
#37309 = DIRECTION ( 'NONE',  ( 0.9687793358424821033, -0.2479245821708680464, 0.000000000000000000 ) ) ;
#37310 = B_SPLINE_CURVE_WITH_KNOTS ( 'NONE', 3,
 ( #48059, #18742, #29587, #14297, #33753, #48293, #10637, #44618, #37193, #44381 ),
 .UNSPECIFIED., .F., .F.,
 ( 4, 2, 2, 2, 4 ),
 ( 0.1272669073657781147, 0.2522669073462887601, 0.3772669073267994611, 0.5022669073073100510, 0.6272669072878207519 ),
 .UNSPECIFIED. ) ;
#37311 = CARTESIAN_POINT ( 'NONE',  ( -21.55884032038934350, -8.611816057827914150, 73.78624026056009200 ) ) ;
#37312 = VERTEX_POINT ( 'NONE', #35093 ) ;
#37313 = CARTESIAN_POINT ( 'NONE',  ( -10.45004451964941872, -15.89438299218807771, 71.59183561948579211 ) ) ;
#37314 = ORIENTED_EDGE ( 'NONE', *, *, #18088, .T. ) ;
#37315 = CARTESIAN_POINT ( 'NONE',  ( -10.70566809389435647, -16.94585225683366048, 57.68760548748760186 ) ) ;
#37316 = CARTESIAN_POINT ( 'NONE',  ( -17.15134141312287852, -7.364115244199362920, 70.67531166753866501 ) ) ;
#37317 =( BOUNDED_SURFACE ( )  B_SPLINE_SURFACE ( 3, 1, ( 
 ( #10346, #44557 ),
 ( #3669, #10813 ),
 ( #11068, #18428 ),
 ( #44326, #25833 ),
 ( #7136, #41339 ),
 ( #36648, #25588 ),
 ( #10579, #22153 ) ),
 .UNSPECIFIED., .T., .F., .F. ) 
 B_SPLINE_SURFACE_WITH_KNOTS ( ( 4, 3, 4 ),
 ( 2, 2 ),
 ( 0.000000000000000000, 0.5000000000000000000, 1.000000000000000000 ),
 ( 0.000000000000000000, 1.000000000000000000 ),
 .UNSPECIFIED. ) 
 GEOMETRIC_REPRESENTATION_ITEM ( )  RATIONAL_B_SPLINE_SURFACE ( (
 ( 1.000000000000000000, 1.000000000000000000),
 ( 0.3333333333333335369, 0.3333333333333330373),
 ( 0.3333333333333335369, 0.3333333333333330373),
 ( 1.000000000000000000, 1.000000000000000000),
 ( 0.3333333333333333703, 0.3333333333333333703),
 ( 0.3333333333333333703, 0.3333333333333333703),
 ( 1.000000000000000000, 1.000000000000000000) ) ) 
 REPRESENTATION_ITEM ( '' )  SURFACE ( )  );
#37318 = CARTESIAN_POINT ( 'NONE',  ( -50.42509385541305988, -8.109206544744111511, 51.54999999999998295 ) ) ;
#37319 = ORIENTED_EDGE ( 'NONE', *, *, #28984, .F. ) ;
#37320 = CARTESIAN_POINT ( 'NONE',  ( -16.10088536661951153, -22.14081006509091054, 58.39311438780030983 ) ) ;
#37321 = VECTOR ( 'NONE', #30985, 1000.000000000000000 ) ;
#37322 = CARTESIAN_POINT ( 'NONE',  ( -18.31433346867779832, -22.20599535381256118, 68.95481354857830070 ) ) ;
#37323 = ORIENTED_EDGE ( 'NONE', *, *, #45395, .T. ) ;
#37324 = AXIS2_PLACEMENT_3D ( 'NONE', #32274, #32021, #43102 ) ;
#37325 = ORIENTED_EDGE ( 'NONE', *, *, #9046, .T. ) ;
#37326 = ORIENTED_EDGE ( 'NONE', *, *, #13927, .T. ) ;
#37327 = DIRECTION ( 'NONE',  ( -0.000000000000000000, 0.000000000000000000, 1.000000000000000000 ) ) ;
#37328 = EDGE_CURVE ( 'NONE', #5083, #35202, #30607, .T. ) ;
#37329 = CARTESIAN_POINT ( 'NONE',  ( -21.18844016355402715, -20.71102104569741087, 69.35450135975200681 ) ) ;
#37330 = EDGE_CURVE ( 'NONE', #19106, #13753, #16626, .T. ) ;
#37331 = CARTESIAN_POINT ( 'NONE',  ( -20.69652669518947263, -8.116311108972663391, 63.35475588450814399 ) ) ;
#37332 = CARTESIAN_POINT ( 'NONE',  ( -10.39374096550114857, -17.27431698850577391, 61.35731899298346548 ) ) ;
#37333 = FACE_OUTER_BOUND ( 'NONE', #37145, .T. ) ;
#37334 = CARTESIAN_POINT ( 'NONE',  ( -14.81376595223554737, -21.78711290537215461, 61.77453959052536447 ) ) ;
#37335 =( BOUNDED_CURVE ( )  B_SPLINE_CURVE ( 3, ( #8447, #45888, #27402, #39211 ),
 .UNSPECIFIED., .F., .F. ) 
 B_SPLINE_CURVE_WITH_KNOTS ( ( 4, 4 ),
 ( 0.4074455897393666204, 0.5000000000000000000 ),
 .UNSPECIFIED. ) 
 CURVE ( )  GEOMETRIC_REPRESENTATION_ITEM ( )  RATIONAL_B_SPLINE_CURVE ( ( 0.6983129098261150469, 0.7760317562607207398, 0.8765941196520169454, 1.000000000000005773 ) ) 
 REPRESENTATION_ITEM ( '' )  );
#37336 = ORIENTED_EDGE ( 'NONE', *, *, #15112, .F. ) ;
#37337 = ORIENTED_EDGE ( 'NONE', *, *, #9683, .T. ) ;
#37338 = EDGE_CURVE ( 'NONE', #10974, #28161, #1989, .T. ) ;
#37339 = CARTESIAN_POINT ( 'NONE',  ( -16.05890242020153380, -7.889590739215661230, 60.08539615417584656 ) ) ;
#37340 = CARTESIAN_POINT ( 'NONE',  ( -13.75230030363714206, -20.82772173381313863, 65.28069058648037526 ) ) ;
#37341 = DIRECTION ( 'NONE',  ( -0.7847243476406478013, -0.6198448985189424221, 4.433022207822356401E-08 ) ) ;
#37342 = EDGE_CURVE ( 'NONE', #36361, #33881, #7523, .T. ) ;
#37343 = DIRECTION ( 'NONE',  ( 1.000000000000000000, -4.164305804376849788E-17, 1.614929280266638808E-16 ) ) ;
#37344 = VERTEX_POINT ( 'NONE', #28460 ) ;
#37345 = CARTESIAN_POINT ( 'NONE',  ( -14.98659385650551457, -9.302874398569244363, 51.68646062012417985 ) ) ;
#37346 = ORIENTED_EDGE ( 'NONE', *, *, #33642, .F. ) ;
#37347 = CARTESIAN_POINT ( 'NONE',  ( -22.17130234749883044, -20.55096496926394778, 58.87947491310501391 ) ) ;
#37348 = CARTESIAN_POINT ( 'NONE',  ( -13.54792730259346456, -8.920061342218058797, 57.25495614889487683 ) ) ;
#37349 = CARTESIAN_POINT ( 'NONE',  ( -15.15518219298508740, -21.43299249554696218, 68.68665981031909951 ) ) ;
#37350 = B_SPLINE_CURVE_WITH_KNOTS ( 'NONE', 1,
 ( #2249, #13789 ),
 .UNSPECIFIED., .F., .F.,
 ( 2, 2 ),
 ( 0.000000000000000000, 1.000000000000000000 ),
 .UNSPECIFIED. ) ;
#37351 = EDGE_CURVE ( 'NONE', #47871, #1499, #38800, .T. ) ;
#37352 = ORIENTED_EDGE ( 'NONE', *, *, #6886, .F. ) ;
#37353 = CARTESIAN_POINT ( 'NONE',  ( -17.56955047399654646, -7.310617185930959216, 53.27966884056655061 ) ) ;
#37354 = EDGE_CURVE ( 'NONE', #40867, #25757, #39394, .T. ) ;
#37355 = CARTESIAN_POINT ( 'NONE',  ( -15.75283589881223278, -7.548994832054173543, 67.32502661251716347 ) ) ;
#37356 = AXIS2_PLACEMENT_3D ( 'NONE', #44809, #40594, #29777 ) ;
#37357 = EDGE_LOOP ( 'NONE', ( #4970, #28987 ) ) ;
#37358 = CARTESIAN_POINT ( 'NONE',  ( -17.19980212172655953, -7.762775302065857197, 70.79035839668001984 ) ) ;
#37359 = EDGE_CURVE ( 'NONE', #38445, #33928, #47166, .T. ) ;
#37360 = CARTESIAN_POINT ( 'NONE',  ( -10.05862335131466700, -15.92885902279982524, 64.69266873560974318 ) ) ;
#37361 = CARTESIAN_POINT ( 'NONE',  ( -19.17437844398820701, -7.979623566120205957, 63.44561363416070776 ) ) ;
#37362 = ORIENTED_EDGE ( 'NONE', *, *, #38312, .F. ) ;
#37363 = CARTESIAN_POINT ( 'NONE',  ( -12.67665486305926237, -12.56770637434968307, 52.02966884056656482 ) ) ;
#37364 = ORIENTED_EDGE ( 'NONE', *, *, #1423, .T. ) ;
#37365 = CARTESIAN_POINT ( 'NONE',  ( -10.20016939456313843, -12.98476690782802834, 71.39483965270750332 ) ) ;
#37366 = LINE ( 'NONE', #7368, #43747 ) ;
#37367 = ORIENTED_EDGE ( 'NONE', *, *, #16286, .T. ) ;
#37368 = DIRECTION ( 'NONE',  ( -0.000000000000000000, -1.000000000000000000, 0.000000000000000000 ) ) ;
#37369 = DIRECTION ( 'NONE',  ( -3.071710424422018668E-17, 6.404604876783312462E-16, 1.000000000000000000 ) ) ;
#37370 = ORIENTED_EDGE ( 'NONE', *, *, #649, .F. ) ;
#37371 = CARTESIAN_POINT ( 'NONE',  ( -11.25989573505624364, -11.38792594226331190, 64.14882039369129529 ) ) ;
#37372 = DIRECTION ( 'NONE',  ( -2.866981220435666553E-17, 1.000000000000000000, 1.190614954331866791E-16 ) ) ;
#37373 = DIRECTION ( 'NONE',  ( -3.071710424422018668E-17, 6.404604876783312462E-16, 1.000000000000000000 ) ) ;
#37374 = ORIENTED_EDGE ( 'NONE', *, *, #31363, .F. ) ;
#37375 = DIRECTION ( 'NONE',  ( 0.000000000000000000, 0.000000000000000000, 1.000000000000000000 ) ) ;
#37376 = CARTESIAN_POINT ( 'NONE',  ( -24.34138173484706158, -16.17068648017255583, 62.59328676670276792 ) ) ;
#37377 = ORIENTED_EDGE ( 'NONE', *, *, #1716, .F. ) ;
#37378 = ORIENTED_EDGE ( 'NONE', *, *, #26839, .F. ) ;
#37379 = CARTESIAN_POINT ( 'NONE',  ( -22.42594789675818845, -19.77792426076253918, 69.45945937764655298 ) ) ;
#37380 = CARTESIAN_POINT ( 'NONE',  ( -11.93102524044397938, -10.47028995287008257, 71.26893105764186487 ) ) ;
#37381 = CARTESIAN_POINT ( 'NONE',  ( -14.25068793291388225, -8.513811817964199946, 71.02957628655769895 ) ) ;
#37382 = CARTESIAN_POINT ( 'NONE',  ( -24.64621740481133116, -16.83181165628401033, 53.49999999999994316 ) ) ;
#37383 = CARTESIAN_POINT ( 'NONE',  ( -16.31159385759798752, -8.990409506049202193, 49.61344411288074951 ) ) ;
#37384 = CARTESIAN_POINT ( 'NONE',  ( -20.44655245503490448, -7.999037100505644204, 70.43755594487680582 ) ) ;
#37385 = B_SPLINE_CURVE_WITH_KNOTS ( 'NONE', 1,
 ( #38217, #27159 ),
 .UNSPECIFIED., .F., .F.,
 ( 2, 2 ),
 ( 0.000000000000000000, 1.000000000000000000 ),
 .UNSPECIFIED. ) ;
#37386 = CARTESIAN_POINT ( 'NONE',  ( -12.30133590797630738, -20.21947593564565793, 68.52312695590214275 ) ) ;
#37387 = DIRECTION ( 'NONE',  ( 0.9687793358424819923, -0.2479245821708676023, 0.000000000000000000 ) ) ;
#37388 = VECTOR ( 'NONE', #22275, 1000.000000000000114 ) ;
#37389 = ORIENTED_EDGE ( 'NONE', *, *, #36176, .F. ) ;
#37390 = EDGE_CURVE ( 'NONE', #23075, #25499, #4415, .T. ) ;
#37391 = CARTESIAN_POINT ( 'NONE',  ( -10.40245588357037043, -14.17414831712846990, 61.20349182037644198 ) ) ;
#37392 = EDGE_CURVE ( 'NONE', #31125, #3060, #32392, .T. ) ;
#37393 = DIRECTION ( 'NONE',  ( 1.224646799147353207E-16, 1.000000000000000000, -1.912410701131276611E-32 ) ) ;
#37394 = CARTESIAN_POINT ( 'NONE',  ( -10.53147947836020215, -13.32716033773700381, 74.68377445404198056 ) ) ;
#37395 = ORIENTED_EDGE ( 'NONE', *, *, #34037, .T. ) ;
#37396 = ORIENTED_EDGE ( 'NONE', *, *, #6056, .T. ) ;
#37397 = CARTESIAN_POINT ( 'NONE',  ( -41.15852941833841783, -25.10920654474410441, 56.99999999999997868 ) ) ;
#37398 = CARTESIAN_POINT ( 'NONE',  ( -10.63166550887824791, -13.11538008670639321, 71.49212078082935307 ) ) ;
#37399 = CARTESIAN_POINT ( 'NONE',  ( -23.34481533081060434, -18.63641918517796370, 69.44371984263474928 ) ) ;
#37400 = CARTESIAN_POINT ( 'NONE',  ( -20.63647318826268773, -18.96169002115701119, 50.77966884056655772 ) ) ;
#37401 = EDGE_CURVE ( 'NONE', #16467, #4162, #46682, .T. ) ;
#37402 = VERTEX_POINT ( 'NONE', #42749 ) ;
#37403 = ADVANCED_FACE ( 'NONE', ( #9018 ), #37776, .T. ) ;
#37404 = DIRECTION ( 'NONE',  ( -3.071710424422018668E-17, 6.404604876783312462E-16, 1.000000000000000000 ) ) ;
#37405 = CARTESIAN_POINT ( 'NONE',  ( -14.22441598498101989, -8.081217260141077219, 67.44470407312981308 ) ) ;
#37406 = ADVANCED_FACE ( 'NONE', ( #31898 ), #2343, .T. ) ;
#37407 = EDGE_CURVE ( 'NONE', #7384, #11732, #9746, .T. ) ;
#37408 = EDGE_CURVE ( 'NONE', #36043, #26347, #35818, .T. ) ;
#37409 = ORIENTED_EDGE ( 'NONE', *, *, #48211, .T. ) ;
#37410 = DIRECTION ( 'NONE',  ( -5.731567514496413899E-31, -1.020425574103664789E-16, -1.000000000000000000 ) ) ;
#37411 = CARTESIAN_POINT ( 'NONE',  ( -24.34278085428046268, -16.17909949234452682, 66.47813813521833026 ) ) ;
#37412 = EDGE_LOOP ( 'NONE', ( #2182, #37916, #8787, #22675, #15191 ) ) ;
#37413 = CARTESIAN_POINT ( 'NONE',  ( -12.65513433691805290, -20.00553804586020590, 64.75186297256590251 ) ) ;
#37414 = AXIS2_PLACEMENT_3D ( 'NONE', #48254, #21451, #29068 ) ;
#37415 = AXIS2_PLACEMENT_3D ( 'NONE', #11813, #33700, #26837 ) ;
#37416 = VERTEX_POINT ( 'NONE', #9977 ) ;
#37417 = FACE_OUTER_BOUND ( 'NONE', #46487, .T. ) ;
#37418 = FACE_OUTER_BOUND ( 'NONE', #44964, .T. ) ;
#37419 = ORIENTED_EDGE ( 'NONE', *, *, #24161, .F. ) ;
#37420 = DIRECTION ( 'NONE',  ( -3.071710424422018668E-17, 6.404604876783312462E-16, 1.000000000000000000 ) ) ;
#37421 = DIRECTION ( 'NONE',  ( -0.8447509909909737269, 0.5351595679979644915, -5.460905094113873772E-17 ) ) ;
#37422 = CARTESIAN_POINT ( 'NONE',  ( -21.37409385650551741, -9.792211528768504536, 50.49490371617623197 ) ) ;
#37423 = CARTESIAN_POINT ( 'NONE',  ( -17.42409385541300182, -14.80920654474440745, 53.27966884056655061 ) ) ;
#37424 = CARTESIAN_POINT ( 'NONE',  ( -10.06071315540565791, -15.94306492381650564, 64.66804923369144831 ) ) ;
#37425 = LINE ( 'NONE', #44604, #46543 ) ;
#37426 = CARTESIAN_POINT ( 'NONE',  ( -25.93570572548787467, -11.53773867808332199, 54.49999999999995026 ) ) ;
#37427 = ORIENTED_EDGE ( 'NONE', *, *, #45521, .T. ) ;
#37428 = CARTESIAN_POINT ( 'NONE',  ( -10.43906464568624060, -14.34976906838038779, 64.38803843031173813 ) ) ;
#37429 = DIRECTION ( 'NONE',  ( -3.071710424422018668E-17, 6.404604876783312462E-16, 1.000000000000000000 ) ) ;
#37430 = CARTESIAN_POINT ( 'NONE',  ( -18.19036405266678713, -21.76720106350623851, 65.63066800548942581 ) ) ;
#37431 = FACE_OUTER_BOUND ( 'NONE', #30394, .T. ) ;
#37432 = LINE ( 'NONE', #16005, #14845 ) ;
#37433 = DIRECTION ( 'NONE',  ( 1.224646799147352961E-16, 1.000000000000000000, -5.292884291094200710E-16 ) ) ;
#37434 = EDGE_CURVE ( 'NONE', #11000, #4941, #9468, .T. ) ;
#37435 = VERTEX_POINT ( 'NONE', #14357 ) ;
#37436 = VERTEX_POINT ( 'NONE', #3310 ) ;
#37437 = CARTESIAN_POINT ( 'NONE',  ( -23.56005053104643210, -11.33143871826892912, 66.30725794404830253 ) ) ;
#37438 = CARTESIAN_POINT ( 'NONE',  ( -14.86281067640541664, -8.294554978430625169, 56.92322698856733609 ) ) ;
#37439 = EDGE_LOOP ( 'NONE', ( #16255, #47203, #48250, #31930 ) ) ;
#37440 = B_SPLINE_CURVE_WITH_KNOTS ( 'NONE', 3,
 ( #12521, #724, #31483, #39106, #42814, #23628, #23371, #38365, #42588, #30775 ),
 .UNSPECIFIED., .F., .F.,
 ( 4, 2, 2, 2, 4 ),
 ( 0.000000000000000000, 0.2500000000000000000, 0.5000000000000000000, 0.7500000000000000000, 1.000000000000000000 ),
 .UNSPECIFIED. ) ;
#37442 = CARTESIAN_POINT ( 'NONE',  ( -24.43827367352892210, -15.52193379869737200, 73.28831629023289906 ) ) ;
#37441 = DIRECTION ( 'NONE',  ( 0.9687793358424821033, -0.2479245821708677133, 0.000000000000000000 ) ) ;
#37443 = CARTESIAN_POINT ( 'NONE',  ( -15.28291166272248347, -21.52618791248891128, 68.87592918174580348 ) ) ;
#37444 = CARTESIAN_POINT ( 'NONE',  ( -12.54283214832790350, -9.790123402769298266, 57.31765315075176659 ) ) ;
#37445 = CARTESIAN_POINT ( 'NONE',  ( -12.41310947992116098, -19.76871611099698001, 61.68206578716802113 ) ) ;
#37446 = CARTESIAN_POINT ( 'NONE',  ( -24.74075702715665770, -16.21285080831185965, 62.77823949964436423 ) ) ;
#37447 = CARTESIAN_POINT ( 'NONE',  ( -23.01870635325979109, -6.403053727051749355, 54.54971261817296835 ) ) ;
#37448 = CYLINDRICAL_SURFACE ( 'NONE', #36542, 2.000000000000001332 ) ;
#37449 = LINE ( 'NONE', #19007, #5517 ) ;
#37450 = CARTESIAN_POINT ( 'NONE',  ( -24.38600339462866629, -15.53964004551538203, 73.30303710393928895 ) ) ;
#37451 = ORIENTED_EDGE ( 'NONE', *, *, #4177, .T. ) ;
#37452 = CARTESIAN_POINT ( 'NONE',  ( -24.09244580564493177, -11.48710279877582785, 63.14492440366687021 ) ) ;
#37453 = DIRECTION ( 'NONE',  ( -0.1240347345892086200, 1.145860353393066553E-16, -0.9922778767136676281 ) ) ;
#37454 = EDGE_CURVE ( 'NONE', #1741, #46443, #47506, .T. ) ;
#37455 = DIRECTION ( 'NONE',  ( 1.000000000000000000, 1.669677910507523057E-21, 6.493791346278465266E-22 ) ) ;
#37456 = DIRECTION ( 'NONE',  ( 3.084459863448555673E-06, -5.853393718798201518E-06, 0.9999999999781119531 ) ) ;
#37457 =( BOUNDED_CURVE ( )  B_SPLINE_CURVE ( 3, ( #3791, #18801, #107, #25954 ),
 .UNSPECIFIED., .F., .F. ) 
 B_SPLINE_CURVE_WITH_KNOTS ( ( 4, 4 ),
 ( 4.712388980384689674, 4.921828490624009511 ),
 .UNSPECIFIED. ) 
 CURVE ( )  GEOMETRIC_REPRESENTATION_ITEM ( )  RATIONAL_B_SPLINE_CURVE ( ( 1.000000000000000000, 0.9963479302455154896, 0.9963479302455154896, 1.000000000000000000 ) ) 
 REPRESENTATION_ITEM ( '' )  );
#37458 = DIRECTION ( 'NONE',  ( -7.340779737911174687E-07, 8.195271841582110202E-07, -0.9999999999993947064 ) ) ;
#37459 = CARTESIAN_POINT ( 'NONE',  ( -18.05440415122280484, -21.83127237841607027, 65.36004252941745563 ) ) ;
#37460 = ORIENTED_EDGE ( 'NONE', *, *, #31562, .F. ) ;
#37461 = AXIS2_PLACEMENT_3D ( 'NONE', #30528, #41340, #719 ) ;
#37462 = EDGE_LOOP ( 'NONE', ( #42654, #1935, #37082, #314, #11274 ) ) ;
#37463 = CIRCLE ( 'NONE', #16224, 1.999999999999994893 ) ;
#37464 = SURFACE_STYLE_FILL_AREA ( #22470 ) ;
#37465 = ORIENTED_EDGE ( 'NONE', *, *, #37848, .T. ) ;
#37466 = CARTESIAN_POINT ( 'NONE',  ( -23.58616520728616806, -18.99640775243969060, 66.00884813586510802 ) ) ;
#37467 = LINE ( 'NONE', #3762, #33924 ) ;
#37468 = AXIS2_PLACEMENT_3D ( 'NONE', #13436, #28484, #10254 ) ;
#37469 =( BOUNDED_CURVE ( )  B_SPLINE_CURVE ( 3, ( #1254, #31791, #35228, #16514 ),
 .UNSPECIFIED., .F., .F. ) 
 B_SPLINE_CURVE_WITH_KNOTS ( ( 4, 4 ),
 ( 0.9074455897393680637, 1.000000000000000000 ),
 .UNSPECIFIED. ) 
 CURVE ( )  GEOMETRIC_REPRESENTATION_ITEM ( )  RATIONAL_B_SPLINE_CURVE ( ( 0.6983129098260993928, 0.7760317562607036423, 0.8765941196520038448, 1.000000000000000000 ) ) 
 REPRESENTATION_ITEM ( '' )  );
#37470 = CARTESIAN_POINT ( 'NONE',  ( -13.34963310073524312, -8.571971970645527961, 57.09154962634697483 ) ) ;
#37471 = EDGE_CURVE ( 'NONE', #39973, #18340, #7008, .T. ) ;
#37472 = EDGE_CURVE ( 'NONE', #1509, #42407, #27854, .T. ) ;
#37473 = CARTESIAN_POINT ( 'NONE',  ( -17.84735332803204599, -7.371153730986438113, 60.19565454701680807 ) ) ;
#37474 = EDGE_LOOP ( 'NONE', ( #8497, #41756, #10015, #45896, #24982, #3983, #46090, #15865, #46331, #5769 ) ) ;
#37475 = CARTESIAN_POINT ( 'NONE',  ( -24.38143469521110518, -15.58083332675401067, 73.00303748421107741 ) ) ;
#37476 = FACE_OUTER_BOUND ( 'NONE', #47898, .T. ) ;
#37477 = EDGE_LOOP ( 'NONE', ( #22744, #7709 ) ) ;
#37478 = CARTESIAN_POINT ( 'NONE',  ( -15.12355705037926334, -21.47721786961508528, 61.63600470926916586 ) ) ;
#37479 = FACE_OUTER_BOUND ( 'NONE', #12593, .T. ) ;
#37480 =( BOUNDED_SURFACE ( )  B_SPLINE_SURFACE ( 3, 1, ( 
 ( #39388, #21588 ),
 ( #12556, #5671 ),
 ( #35673, #16954 ),
 ( #6569, #8876 ),
 ( #36566, #23897 ),
 ( #14158, #4943 ),
 ( #19951, #1222 ) ),
 .UNSPECIFIED., .T., .F., .F. ) 
 B_SPLINE_SURFACE_WITH_KNOTS ( ( 4, 3, 4 ),
 ( 2, 2 ),
 ( 0.000000000000000000, 0.5000000000000000000, 1.000000000000000000 ),
 ( 0.000000000000000000, 1.000000000000000000 ),
 .UNSPECIFIED. ) 
 GEOMETRIC_REPRESENTATION_ITEM ( )  RATIONAL_B_SPLINE_SURFACE ( (
 ( 1.000000000000000000, 1.000000000000000000),
 ( 0.3333333333333335369, 0.3333333333333330373),
 ( 0.3333333333333335369, 0.3333333333333330373),
 ( 1.000000000000000000, 1.000000000000000000),
 ( 0.3333333333333333703, 0.3333333333333333703),
 ( 0.3333333333333333703, 0.3333333333333333703),
 ( 1.000000000000000000, 1.000000000000000000) ) ) 
 REPRESENTATION_ITEM ( '' )  SURFACE ( )  );
#37481 = VERTEX_POINT ( 'NONE', #40265 ) ;
#37482 = EDGE_CURVE ( 'NONE', #7471, #35637, #19989, .T. ) ;
#37483 = EDGE_CURVE ( 'NONE', #21028, #8614, #22028, .T. ) ;
#37484 = CARTESIAN_POINT ( 'NONE',  ( -19.75048190521760461, -21.47275536819973141, 62.15070614013394135 ) ) ;
#37485 = FACE_OUTER_BOUND ( 'NONE', #25825, .T. ) ;
#37486 = DIRECTION ( 'NONE',  ( -0.3739781583979218116, -0.9274375111247651349, -6.296758467538796555E-09 ) ) ;
#37487 = ORIENTED_EDGE ( 'NONE', *, *, #34901, .F. ) ;
#37488 = CARTESIAN_POINT ( 'NONE',  ( -12.76273281506171919, -20.09846992828358125, 71.81213450582208679 ) ) ;
#37489 = CYLINDRICAL_SURFACE ( 'NONE', #14700, 0.1500000000000072387 ) ;
#37490 = CARTESIAN_POINT ( 'NONE',  ( -15.03805467426947828, -21.39046384358795194, 65.12213282899359967 ) ) ;
#37491 = CARTESIAN_POINT ( 'NONE',  ( -23.91439695282944200, -17.43141281116713515, 66.24357239631997629 ) ) ;
#37492 = ORIENTED_EDGE ( 'NONE', *, *, #18327, .F. ) ;
#37493 = CARTESIAN_POINT ( 'NONE',  ( -10.61641629527463770, -11.78277212779517136, 74.74335553404092991 ) ) ;
#37494 = FACE_OUTER_BOUND ( 'NONE', #30524, .T. ) ;
#37495 = CARTESIAN_POINT ( 'NONE',  ( -15.34011606297474195, -21.49348192942642655, 72.15648571357043295 ) ) ;
#37496 = CIRCLE ( 'NONE', #21794, 1.500000000000001332 ) ;
#37497 = CIRCLE ( 'NONE', #548, 1.500000000000001332 ) ;
#37498 = CARTESIAN_POINT ( 'NONE',  ( -11.07857854458970692, -11.73724703412850801, 71.08860870961423473 ) ) ;
#37499 = CARTESIAN_POINT ( 'NONE',  ( -18.36159385650551812, -9.295667164867525756, 49.30633214617472504 ) ) ;
#37500 = EDGE_CURVE ( 'NONE', #42725, #44357, #4280, .T. ) ;
#37501 = EDGE_LOOP ( 'NONE', ( #22297, #45141, #18173, #41225 ) ) ;
#37502 = CARTESIAN_POINT ( 'NONE',  ( -13.51659408464697698, -24.65568926594394128, 53.49999999999995026 ) ) ;
#37503 = FACE_OUTER_BOUND ( 'NONE', #5123, .T. ) ;
#37504 = ORIENTED_EDGE ( 'NONE', *, *, #3192, .T. ) ;
#37505 = LINE ( 'NONE', #3800, #39439 ) ;
#37506 = AXIS2_PLACEMENT_3D ( 'NONE', #36994, #6978, #29625 ) ;
#37507 = CARTESIAN_POINT ( 'NONE',  ( -11.73260704738458671, -10.00184175524024610, 67.61401452035728710 ) ) ;
#37508 = ORIENTED_EDGE ( 'NONE', *, *, #44753, .F. ) ;
#37509 = LINE ( 'NONE', #16806, #26280 ) ;
#37510 = DIRECTION ( 'NONE',  ( -0.3478314405900341799, -0.9375570856950852239, 0.000000000000000000 ) ) ;
#37511 = ORIENTED_EDGE ( 'NONE', *, *, #38866, .F. ) ;
#37512 = CARTESIAN_POINT ( 'NONE',  ( -12.97364781899516650, -9.395219913213448848, 49.41431986088092998 ) ) ;
#37513 = CARTESIAN_POINT ( 'NONE',  ( -12.84086788549150704, -8.935670915691353855, 67.55659650341593192 ) ) ;
#37514 = CARTESIAN_POINT ( 'NONE',  ( -10.89849601230814713, -17.47747223720621434, 68.09721941041966886 ) ) ;
#37515 = CARTESIAN_POINT ( 'NONE',  ( -16.13432406759100601, -21.74052631579560568, 58.30057715624173653 ) ) ;
#37516 = B_SPLINE_CURVE_WITH_KNOTS ( 'NONE', 1,
 ( #22663, #30309 ),
 .UNSPECIFIED., .F., .F.,
 ( 2, 2 ),
 ( 0.000000000000000000, 1.000000000000000000 ),
 .UNSPECIFIED. ) ;
#37517 = CARTESIAN_POINT ( 'NONE',  ( -10.78898398081525301, -17.19290454168847404, 61.44271037915215317 ) ) ;
#37518 = EDGE_LOOP ( 'NONE', ( #1477, #3358 ) ) ;
#37519 = ORIENTED_EDGE ( 'NONE', *, *, #22841, .T. ) ;
#37520 = CARTESIAN_POINT ( 'NONE',  ( -14.00534385650551883, -8.801233750844183135, 48.81488406609782515 ) ) ;
#37521 = CARTESIAN_POINT ( 'NONE',  ( -10.45863951484398946, -14.11462368554138536, 60.91821294131582931 ) ) ;
#37522 = DIRECTION ( 'NONE',  ( 0.000000000000000000, 0.000000000000000000, 1.000000000000000000 ) ) ;
#37523 = CARTESIAN_POINT ( 'NONE',  ( -15.07409385650551670, -9.792211528768504536, 50.49490371617623197 ) ) ;
#37524 = AXIS2_PLACEMENT_3D ( 'NONE', #24830, #25543, #2417 ) ;
#37525 = VECTOR ( 'NONE', #44066, 1000.000000000000000 ) ;
#37526 = ORIENTED_EDGE ( 'NONE', *, *, #26585, .F. ) ;
#37527 = EDGE_CURVE ( 'NONE', #3166, #21687, #17048, .T. ) ;
#37528 = CARTESIAN_POINT ( 'NONE',  ( -18.72680909822608797, -7.880611277284092608, 70.52068030200462090 ) ) ;
#37529 = CARTESIAN_POINT ( 'NONE',  ( -14.01837044221388595, -8.636059239884618322, 74.48482605064899076 ) ) ;
#37530 = PLANE ( 'NONE',  #45370 ) ;
#37531 = ORIENTED_EDGE ( 'NONE', *, *, #27878, .T. ) ;
#37532 = FACE_OUTER_BOUND ( 'NONE', #17067, .T. ) ;
#37533 = AXIS2_PLACEMENT_3D ( 'NONE', #7261, #11189, #22767 ) ;
#37534 = ORIENTED_EDGE ( 'NONE', *, *, #47511, .F. ) ;
#37535 = EDGE_CURVE ( 'NONE', #20491, #21857, #46473, .T. ) ;
#37536 = DIRECTION ( 'NONE',  ( 5.297746385098606630E-06, 8.914243324979344743E-06, 0.9999999999462350075 ) ) ;
#37537 = CARTESIAN_POINT ( 'NONE',  ( -18.22959580818018566, -21.76314769987743603, 68.83131364167647348 ) ) ;
#37538 = DIRECTION ( 'NONE',  ( 0.9687793358424821033, -0.2479245821708679909, 0.000000000000000000 ) ) ;
#37539 = LINE ( 'NONE', #29688, #34850 ) ;
#37540 = EDGE_CURVE ( 'NONE', #25382, #7068, #29414, .T. ) ;
#37541 = ORIENTED_EDGE ( 'NONE', *, *, #18126, .T. ) ;
#37542 = CARTESIAN_POINT ( 'NONE',  ( -17.98657259272421172, -21.83703102787368167, 62.16063850355641307 ) ) ;
#37543 = CARTESIAN_POINT ( 'NONE',  ( -15.37055318500739354, -21.97060318045666705, 72.24564236423489660 ) ) ;
#37544 = EDGE_CURVE ( 'NONE', #1836, #22645, #28665, .T. ) ;
#37545 = CARTESIAN_POINT ( 'NONE',  ( -10.98557804775572144, -17.68114217416224321, 71.71718193507115302 ) ) ;
#37546 = CARTESIAN_POINT ( 'NONE',  ( -19.86401518824997581, -21.42384811948916479, 69.22010401872219632 ) ) ;
#37547 = ORIENTED_EDGE ( 'NONE', *, *, #9148, .T. ) ;
#37548 = DIRECTION ( 'NONE',  ( -5.731567514496413899E-31, -1.020425574103664789E-16, -1.000000000000000000 ) ) ;
#37549 = CARTESIAN_POINT ( 'NONE',  ( -17.21518928061367859, -7.362082935544761675, 70.59761670184047944 ) ) ;
#37550 = CARTESIAN_POINT ( 'NONE',  ( -18.76558392140857023, -7.480892851696864021, 70.55563303198719893 ) ) ;
#37551 = FACE_BOUND ( 'NONE', #23762, .T. ) ;
#37552 = EDGE_LOOP ( 'NONE', ( #45994, #36015, #39801, #44549, #3969 ) ) ;
#37553 = LINE ( 'NONE', #11723, #6168 ) ;
#37554 = CARTESIAN_POINT ( 'NONE',  ( -10.55840381512346049, -16.17443265670291197, 71.44750434600322819 ) ) ;
#37555 = CARTESIAN_POINT ( 'NONE',  ( -16.97945985512182787, -21.84517132341290591, 72.16543221430227106 ) ) ;
#37556 = VECTOR ( 'NONE', #37486, 1000.000000000000114 ) ;
#37557 = CARTESIAN_POINT ( 'NONE',  ( -24.85076376908920537, -14.22007681150577518, 69.80275272707126533 ) ) ;
#37558 = VERTEX_POINT ( 'NONE', #10946 ) ;
#37559 = CARTESIAN_POINT ( 'NONE',  ( -10.50429924535250414, -16.15944446069507023, 71.46222527016213633 ) ) ;
#37560 = ORIENTED_EDGE ( 'NONE', *, *, #4620, .F. ) ;
#37561 = CARTESIAN_POINT ( 'NONE',  ( -12.67941281020567068, -9.065306902972979586, 71.02642229240572647 ) ) ;
#37562 = DIRECTION ( 'NONE',  ( 0.000000000000000000, -0.9999954153791273948, -0.003028072113819838245 ) ) ;
#37563 = FACE_OUTER_BOUND ( 'NONE', #6018, .T. ) ;
#37564 = ORIENTED_EDGE ( 'NONE', *, *, #46898, .T. ) ;
#37565 = CARTESIAN_POINT ( 'NONE',  ( -10.78978130820344994, -12.42417047965500565, 57.62857332104950103 ) ) ;
#37566 = TOROIDAL_SURFACE ( 'NONE', #41527, 1.999999999999999112, 1.249999999999999334 ) ;
#37567 = VECTOR ( 'NONE', #40179, 1000.000000000000227 ) ;
#37568 = CARTESIAN_POINT ( 'NONE',  ( -18.39194801826630510, -22.19612395633120627, 69.00788843400852102 ) ) ;
#37569 = EDGE_LOOP ( 'NONE', ( #45526, #44298, #2582, #17496 ) ) ;
#37570 = EDGE_LOOP ( 'NONE', ( #34860, #27958, #19027, #17261, #14033 ) ) ;
#37571 = ORIENTED_EDGE ( 'NONE', *, *, #96, .T. ) ;
#37572 = CARTESIAN_POINT ( 'NONE',  ( -15.27269024242438533, -21.52607325516635939, 72.46064223565690554 ) ) ;
#37573 = CARTESIAN_POINT ( 'NONE',  ( -18.05440415122280839, -21.83127237841607027, 65.36004252941745563 ) ) ;
#37574 = VECTOR ( 'NONE', #5246, 1000.000000000000000 ) ;
#37575 = CARTESIAN_POINT ( 'NONE',  ( -21.95523322170430092, -8.895446802377390938, 66.77654591769551473 ) ) ;
#37576 = CARTESIAN_POINT ( 'NONE',  ( -20.73422126667899690, -8.581213913796407411, 63.72610227039507436 ) ) ;
#37577 = CARTESIAN_POINT ( 'NONE',  ( -21.76912952166680881, -20.36565426623231190, 58.85623051144766293 ) ) ;
#37578 = CYLINDRICAL_SURFACE ( 'NONE', #26305, 0.1500000000000050737 ) ;
#37579 = CARTESIAN_POINT ( 'NONE',  ( -23.46260370332432288, -11.17067683354235719, 73.66193301755811262 ) ) ;
#37580 = VECTOR ( 'NONE', #16922, 1000.000000000000000 ) ;
#37581 = ORIENTED_EDGE ( 'NONE', *, *, #9570, .F. ) ;
#37582 = ORIENTED_EDGE ( 'NONE', *, *, #43862, .F. ) ;
#37583 = CARTESIAN_POINT ( 'NONE',  ( -17.49728986656368335, -7.358816873484950172, 63.66401766577892118 ) ) ;
#37584 = DIRECTION ( 'NONE',  ( -1.000000000000000000, -1.669677910507523057E-21, -6.493791346278465266E-22 ) ) ;
#37585 = CARTESIAN_POINT ( 'NONE',  ( -14.84927081153347039, -21.37251255130113137, 61.65072491673618771 ) ) ;
#37586 = LINE ( 'NONE', #18631, #18947 ) ;
#37587 = ORIENTED_EDGE ( 'NONE', *, *, #15293, .T. ) ;
#37588 = ADVANCED_FACE ( 'NONE', ( #10471 ), #40984, .T. ) ;
#37589 = CARTESIAN_POINT ( 'NONE',  ( -15.32409385650551670, -6.426201560718813433, 50.50509628382439331 ) ) ;
#37590 = B_SPLINE_CURVE_WITH_KNOTS ( 'NONE', 3,
 ( #33949, #23364, #27297, #42323, #46258, #8591, #243, #15221, #38619, #41591 ),
 .UNSPECIFIED., .F., .F.,
 ( 4, 2, 2, 2, 4 ),
 ( 0.000000000000000000, 0.2500000000000000000, 0.5000000000000000000, 0.7500000000000000000, 1.000000000000000000 ),
 .UNSPECIFIED. ) ;
#37591 = ORIENTED_EDGE ( 'NONE', *, *, #31976, .F. ) ;
#37592 = CARTESIAN_POINT ( 'NONE',  ( -42.55865267894247239, -14.90920654474414775, 61.92352941176469727 ) ) ;
#37593 = CARTESIAN_POINT ( 'NONE',  ( -12.18836193727821460, -19.53083876418623532, 57.94154444592973618 ) ) ;
#37594 = AXIS2_PLACEMENT_3D ( 'NONE', #1343, #31397, #26979 ) ;
#37595 = CARTESIAN_POINT ( 'NONE',  ( -10.45740709548926262, -13.70915569549963031, 57.86313879094461754 ) ) ;
#37596 = AXIS2_PLACEMENT_3D ( 'NONE', #24470, #36248, #43425 ) ;
#37597 = ORIENTED_EDGE ( 'NONE', *, *, #39048, .T. ) ;
#37598 = DIRECTION ( 'NONE',  ( -3.071710424422018668E-17, 6.404604876783312462E-16, 1.000000000000000000 ) ) ;
#37599 = CIRCLE ( 'NONE', #14802, 2.000000000000000000 ) ;
#37600 = VECTOR ( 'NONE', #4110, 1000.000000000000227 ) ;
#37601 = CARTESIAN_POINT ( 'NONE',  ( -10.38752013045322009, -14.36951432065623813, 64.67331771650336236 ) ) ;
#37602 = CARTESIAN_POINT ( 'NONE',  ( -21.65477468606848532, -9.232349032746775208, 66.96149992608901869 ) ) ;
#37603 = EDGE_CURVE ( 'NONE', #42912, #33146, #23271, .T. ) ;
#37604 = ORIENTED_EDGE ( 'NONE', *, *, #33744, .F. ) ;
#37605 = CARTESIAN_POINT ( 'NONE',  ( -24.26499789074519597, -17.75976756996305639, 62.65856417960095825 ) ) ;
#37606 = EDGE_CURVE ( 'NONE', #46221, #46252, #13883, .T. ) ;
#37607 =( BOUNDED_SURFACE ( )  B_SPLINE_SURFACE ( 3, 1, ( 
 ( #29334, #15019 ),
 ( #44366, #3719 ),
 ( #30082, #6924 ),
 ( #33240, #21944 ),
 ( #3228, #11352 ),
 ( #48280, #29573 ),
 ( #10859, #14759 ) ),
 .UNSPECIFIED., .T., .F., .F. ) 
 B_SPLINE_SURFACE_WITH_KNOTS ( ( 4, 3, 4 ),
 ( 2, 2 ),
 ( 0.000000000000000000, 0.5000000000000000000, 1.000000000000000000 ),
 ( 0.000000000000000000, 1.000000000000000000 ),
 .UNSPECIFIED. ) 
 GEOMETRIC_REPRESENTATION_ITEM ( )  RATIONAL_B_SPLINE_SURFACE ( (
 ( 1.000000000000000000, 1.000000000000000000),
 ( 0.3333333333333335369, 0.3333333333333330373),
 ( 0.3333333333333335369, 0.3333333333333330373),
 ( 1.000000000000000000, 1.000000000000000000),
 ( 0.3333333333333333703, 0.3333333333333333703),
 ( 0.3333333333333333703, 0.3333333333333333703),
 ( 1.000000000000000000, 1.000000000000000000) ) ) 
 REPRESENTATION_ITEM ( '' )  SURFACE ( )  );
#37608 = DIRECTION ( 'NONE',  ( -0.000000000000000000, -1.000000000000000000, -0.000000000000000000 ) ) ;
#37609 = LINE ( 'NONE', #47793, #14227 ) ;
#37610 = VERTEX_POINT ( 'NONE', #33826 ) ;
#37611 = CARTESIAN_POINT ( 'NONE',  ( -11.14069362286655718, -11.72368817214407599, 71.08860884459858198 ) ) ;
#37612 = ORIENTED_EDGE ( 'NONE', *, *, #37911, .T. ) ;
#37613 = CARTESIAN_POINT ( 'NONE',  ( -10.32134938064561247, -17.05723401094961034, 57.88771750990810006 ) ) ;
#37614 = CARTESIAN_POINT ( 'NONE',  ( -11.49187621880558119, -18.52825149122186943, 64.93634258412723170 ) ) ;
#37615 = EDGE_CURVE ( 'NONE', #35750, #16040, #18815, .T. ) ;
#37616 = VERTEX_POINT ( 'NONE', #30650 ) ;
#37617 = CARTESIAN_POINT ( 'NONE',  ( -12.85387012802420514, -9.430729208696401855, 67.53509681483876648 ) ) ;
#37618 = DIRECTION ( 'NONE',  ( -7.236285704734400469E-17, 0.7640846180167337742, 0.6451160333693637394 ) ) ;
#37619 = LINE ( 'NONE', #33190, #47778 ) ;
#37620 = ORIENTED_EDGE ( 'NONE', *, *, #18837, .T. ) ;
#37621 = CARTESIAN_POINT ( 'NONE',  ( -27.42409385541305156, -14.65920654474411045, 47.99999999999997868 ) ) ;
#37622 = ADVANCED_FACE ( 'NONE', ( #45185 ), #45672, .F. ) ;
#37623 = CARTESIAN_POINT ( 'NONE',  ( -19.61601503992405071, -21.50980213996393786, 65.76486213821364402 ) ) ;
#37624 = CARTESIAN_POINT ( 'NONE',  ( -12.00971705810820467, -9.691755786776280246, 60.67422651510300113 ) ) ;
#37625 = ORIENTED_EDGE ( 'NONE', *, *, #46781, .T. ) ;
#37626 = DIRECTION ( 'NONE',  ( -3.289814948237356682E-07, -7.277561423860909391E-07, 0.9999999999996810329 ) ) ;
#37627 =( BOUNDED_CURVE ( )  B_SPLINE_CURVE ( 3, ( #1812, #8970, #42935, #1567 ),
 .UNSPECIFIED., .F., .F. ) 
 B_SPLINE_CURVE_WITH_KNOTS ( ( 4, 4 ),
 ( 0.4074455897393643999, 0.5000000000000000000 ),
 .UNSPECIFIED. ) 
 CURVE ( )  GEOMETRIC_REPRESENTATION_ITEM ( )  RATIONAL_B_SPLINE_CURVE ( ( 0.6983129098260837386, 0.7760317562606962039, 0.8765941196520034007, 1.000000000000009548 ) ) 
 REPRESENTATION_ITEM ( '' )  );
#37628 = CARTESIAN_POINT ( 'NONE',  ( -21.73719165441269396, -8.734630208819112340, 70.32406670146895067 ) ) ;
#37629 = CARTESIAN_POINT ( 'NONE',  ( -14.92409385541305333, -14.80920654474410725, 79.00000000000000000 ) ) ;
#37630 = ORIENTED_EDGE ( 'NONE', *, *, #46108, .T. ) ;
#37631 = ORIENTED_EDGE ( 'NONE', *, *, #12010, .F. ) ;
#37632 = CARTESIAN_POINT ( 'NONE',  ( -12.48216758013337113, -16.58117287899024461, 52.02966884056656482 ) ) ;
#37633 = CARTESIAN_POINT ( 'NONE',  ( -10.73080526501584941, -11.53763522125388086, 71.19586713194442495 ) ) ;
#37635 = CARTESIAN_POINT ( 'NONE',  ( -23.50857174774670355, -19.10953103619692328, 62.46751498843644157 ) ) ;
#37634 = VECTOR ( 'NONE', #27647, 1000.000000000000000 ) ;
#37636 = B_SPLINE_CURVE_WITH_KNOTS ( 'NONE', 3,
 ( #41645, #48288, #523, #30579, #25891, #37189, #22202, #18485, #33491, #26143 ),
 .UNSPECIFIED., .F., .F.,
 ( 4, 2, 2, 2, 4 ),
 ( 0.000000000000000000, 0.2500000000000000000, 0.5000000000000000000, 0.7500000000000000000, 1.000000000000000000 ),
 .UNSPECIFIED. ) ;
#37637 = DIRECTION ( 'NONE',  ( 0.000000000000000000, 0.000000000000000000, 1.000000000000000000 ) ) ;
#37638 = CARTESIAN_POINT ( 'NONE',  ( -13.61159385759799001, -8.990409506049202193, 49.61344411288074951 ) ) ;
#37639 = CARTESIAN_POINT ( 'NONE',  ( -12.50924672071177923, -19.79360999578536351, 61.50564738844418144 ) ) ;
#37640 = COLOUR_RGB ( '', 0.66274510, 0.83137255, 0.94901961) ;
#37641 = CARTESIAN_POINT ( 'NONE',  ( -12.10369268100898132, -9.594121713099781346, 57.27430968559156810 ) ) ;
#37642 = CARTESIAN_POINT ( 'NONE',  ( -24.34502386579654498, -17.56683345968398768, 66.12852568699506151 ) ) ;
#37643 = VECTOR ( 'NONE', #19504, 1000.000000000000000 ) ;
#37644 = CARTESIAN_POINT ( 'NONE',  ( -16.52978676676487169, -22.20534210804297715, 65.42575595334410821 ) ) ;
#37645 = VERTEX_POINT ( 'NONE', #19061 ) ;
#37646 = CARTESIAN_POINT ( 'NONE',  ( -11.49688049385020960, -18.62690763749001732, 64.76179218520603342 ) ) ;
#37647 = SHAPE_REPRESENTATION_RELATIONSHIP ( 'NONE' , 'NONE' ,  #46513, #12638 ) ;
#37648 = AXIS2_PLACEMENT_3D ( 'NONE', #35337, #23546, #19850 ) ;
#37649 = DIRECTION ( 'NONE',  ( -3.071710424422018668E-17, 6.404604876783312462E-16, 1.000000000000000000 ) ) ;
#37650 = CARTESIAN_POINT ( 'NONE',  ( -14.98297878932515381, -10.79466886532025605, 49.52966884056655772 ) ) ;
#37651 = EDGE_CURVE ( 'NONE', #30489, #27713, #28300, .T. ) ;
#37652 = ORIENTED_EDGE ( 'NONE', *, *, #25727, .T. ) ;
#37653 = ORIENTED_EDGE ( 'NONE', *, *, #8028, .F. ) ;
#37654 = CARTESIAN_POINT ( 'NONE',  ( -21.61813339613238227, -8.651787399021619862, 73.71633365192373333 ) ) ;
#37655 = CARTESIAN_POINT ( 'NONE',  ( -9.974654501588993583, -14.90060059298426864, 74.94778899347312517 ) ) ;
#37656 = CARTESIAN_POINT ( 'NONE',  ( -13.28665195206506766, -21.00489563950134553, 61.67792873707563928 ) ) ;
#37657 = CARTESIAN_POINT ( 'NONE',  ( -13.83862390296875056, -21.33972285065757291, 72.11946018631711297 ) ) ;
#37658 = ORIENTED_EDGE ( 'NONE', *, *, #12102, .T. ) ;
#37659 = ADVANCED_FACE ( 'NONE', ( #38005 ), #8237, .T. ) ;
#37660 = CYLINDRICAL_SURFACE ( 'NONE', #8559, 0.1499999999999993838 ) ;
#37661 = CARTESIAN_POINT ( 'NONE',  ( -24.43113031232903865, -15.58634216689856800, 73.30303748141028564 ) ) ;
#37662 = ORIENTED_EDGE ( 'NONE', *, *, #44136, .T. ) ;
#37663 = DIRECTION ( 'NONE',  ( -1.616182858256117057E-16, -0.003028072113818697231, 0.9999954153791273948 ) ) ;
#37664 = VECTOR ( 'NONE', #4895, 1000.000000000000000 ) ;
#37665 = DIRECTION ( 'NONE',  ( -1.224646799147353207E-16, -1.000000000000000000, 1.912410701131276611E-32 ) ) ;
#37666 = ORIENTED_EDGE ( 'NONE', *, *, #43293, .T. ) ;
#37667 = CARTESIAN_POINT ( 'NONE',  ( -24.77723877343947478, -16.00713684962007122, 66.24820200538215431 ) ) ;
#37668 = VERTEX_POINT ( 'NONE', #34068 ) ;
#37669 = LINE ( 'NONE', #42113, #15731 ) ;
#37670 = AXIS2_PLACEMENT_3D ( 'NONE', #184, #7564, #30221 ) ;
#37671 = EDGE_LOOP ( 'NONE', ( #10154, #28205, #35935, #48583, #11926 ) ) ;
#37672 = CARTESIAN_POINT ( 'NONE',  ( -11.19819527566065887, -18.90074491542570456, 64.89707073357136835 ) ) ;
#37673 = B_SPLINE_CURVE_WITH_KNOTS ( 'NONE', 3,
 ( #470, #11303, #37881, #26562, #18669, #12265, #14962, #42315, #34415, #42071 ),
 .UNSPECIFIED., .F., .F.,
 ( 4, 2, 2, 2, 4 ),
 ( 0.000000000000000000, 0.2500000000000000000, 0.5000000000000000000, 0.7500000000000000000, 1.000000000000000000 ),
 .UNSPECIFIED. ) ;
#37674 = EDGE_CURVE ( 'NONE', #22263, #27202, #43410, .T. ) ;
#37675 = CARTESIAN_POINT ( 'NONE',  ( -11.14029015952437263, -10.80702246001832023, 57.46549161190092292 ) ) ;
#37676 = EDGE_LOOP ( 'NONE', ( #12133, #17937, #48269, #41242 ) ) ;
#37677 = CARTESIAN_POINT ( 'NONE',  ( -13.32057209662121267, -9.066726955530414855, 57.12534593251891124 ) ) ;
#37678 = CARTESIAN_POINT ( 'NONE',  ( -10.39679176622870038, -14.24023819782134481, 64.40275955115841100 ) ) ;
#37679 = CARTESIAN_POINT ( 'NONE',  ( -19.40534385650551741, -8.801233750844183135, 48.81488406609782515 ) ) ;
#37680 = CARTESIAN_POINT ( 'NONE',  ( -17.05328393105827089, -14.65920654474411045, 48.99999999999997868 ) ) ;
#37681 = AXIS2_PLACEMENT_3D ( 'NONE', #22261, #18807, #6999 ) ;
#37682 = EDGE_CURVE ( 'NONE', #24279, #18615, #9757, .T. ) ;
#37683 = DIRECTION ( 'NONE',  ( 0.9118114225829225816, 0.4106092176842893182, 5.589476759239149737E-08 ) ) ;
#37684 = CARTESIAN_POINT ( 'NONE',  ( -22.23024899390505027, -9.116745682064513190, 59.82832910242247237 ) ) ;
#37685 = CARTESIAN_POINT ( 'NONE',  ( -13.42146604834728763, -8.525632923396102569, 57.14780542301615185 ) ) ;
#37686 = EDGE_LOOP ( 'NONE', ( #18479, #38113, #39811, #5784, #13207, #38863, #6197, #41878 ) ) ;
#37687 = LINE ( 'NONE', #4221, #8197 ) ;
#37688 = DIRECTION ( 'NONE',  ( -0.9441784275685841665, 0.3294345108122634369, 1.993146885055994800E-08 ) ) ;
#37689 = FACE_OUTER_BOUND ( 'NONE', #47482, .T. ) ;
#37690 = CARTESIAN_POINT ( 'NONE',  ( -22.39476240126155560, -20.35875292466404574, 62.39472529595067840 ) ) ;
#37691 = CARTESIAN_POINT ( 'NONE',  ( -24.18834572025230401, -13.00761457142965938, 62.90552128796598907 ) ) ;
#37692 = ORIENTED_EDGE ( 'NONE', *, *, #42350, .F. ) ;
#37693 = VERTEX_POINT ( 'NONE', #26698 ) ;
#37694 = FACE_OUTER_BOUND ( 'NONE', #872, .T. ) ;
#37695 = CARTESIAN_POINT ( 'NONE',  ( -22.91296630721855365, -15.15889098507617128, 53.49999999999995026 ) ) ;
#37696 = ORIENTED_EDGE ( 'NONE', *, *, #226, .T. ) ;
#37697 = CARTESIAN_POINT ( 'NONE',  ( -21.01131272606871292, -21.33876233430101621, 62.30809711058548572 ) ) ;
#37698 = CARTESIAN_POINT ( 'NONE',  ( -16.38232541403072773, -22.18617787627378846, 61.89421581153325747 ) ) ;
#37699 = CARTESIAN_POINT ( 'NONE',  ( -45.92409385541306222, -14.20920654474410760, 70.50000000000000000 ) ) ;
#37700 = CARTESIAN_POINT ( 'NONE',  ( -17.27965118537360212, -7.810258991196201706, 70.77419234192039710 ) ) ;
#37701 = ADVANCED_FACE ( 'NONE', ( #33564 ), #14439, .T. ) ;
#37702 = LINE ( 'NONE', #34747, #14074 ) ;
#37703 = CARTESIAN_POINT ( 'NONE',  ( -19.52948875563194875, -21.95553444029042467, 62.09529400939659638 ) ) ;
#37704 = EDGE_CURVE ( 'NONE', #27713, #29708, #11035, .T. ) ;
#37705 = DIRECTION ( 'NONE',  ( 0.9956360040033426229, -0.09332174201254497814, 0.000000000000000000 ) ) ;
#37706 = CARTESIAN_POINT ( 'NONE',  ( -16.43317471172368016, -9.385549587026176255, 53.88362224778186516 ) ) ;
#37707 = DIRECTION ( 'NONE',  ( 0.3688590060343596155, -0.9294853595766554566, 0.000000000000000000 ) ) ;
#37708 = ADVANCED_FACE ( 'NONE', ( #30890 ), #38495, .F. ) ;
#37709 = EDGE_CURVE ( 'NONE', #20623, #22645, #37509, .T. ) ;
#37710 = DIRECTION ( 'NONE',  ( 0.9687793358424819923, -0.2479245821708680464, 0.000000000000000000 ) ) ;
#37711 = AXIS2_PLACEMENT_3D ( 'NONE', #31026, #46044, #12299 ) ;
#37712 = CARTESIAN_POINT ( 'NONE',  ( -12.05615918852498680, -19.97535170061420828, 61.51183199568394144 ) ) ;
#37713 =( BOUNDED_CURVE ( )  B_SPLINE_CURVE ( 3, ( #16925, #36594, #25782, #47951 ),
 .UNSPECIFIED., .F., .F. ) 
 B_SPLINE_CURVE_WITH_KNOTS ( ( 4, 4 ),
 ( 0.9074455897393651771, 1.000000000000000000 ),
 .UNSPECIFIED. ) 
 CURVE ( )  GEOMETRIC_REPRESENTATION_ITEM ( )  RATIONAL_B_SPLINE_CURVE ( ( 0.6983129098260764112, 0.7760317562606838804, 0.8765941196519917433, 1.000000000000000000 ) ) 
 REPRESENTATION_ITEM ( '' )  );
#37714 = DIRECTION ( 'NONE',  ( -3.071710424422018668E-17, 6.404604876783312462E-16, 1.000000000000000000 ) ) ;
#37715 = CARTESIAN_POINT ( 'NONE',  ( -13.01353307917097268, -8.804980454159759162, 64.09441913135431435 ) ) ;
#37716 = CARTESIAN_POINT ( 'NONE',  ( 18.87590614458706995, 1.890747609047893185, 50.53028072113869484 ) ) ;
#37717 = CIRCLE ( 'NONE', #37670, 0.5560000000000009379 ) ;
#37718 = ORIENTED_EDGE ( 'NONE', *, *, #4183, .F. ) ;
#37719 = ORIENTED_EDGE ( 'NONE', *, *, #44562, .T. ) ;
#37720 = CARTESIAN_POINT ( 'NONE',  ( -15.04284385541304125, -7.587656875400194068, 49.25157356644813689 ) ) ;
#37721 = ORIENTED_EDGE ( 'NONE', *, *, #29601, .T. ) ;
#37722 = CARTESIAN_POINT ( 'NONE',  ( -23.54569140518488624, -19.05536029250058050, 65.93894040291287695 ) ) ;
#37723 = CARTESIAN_POINT ( 'NONE',  ( -16.39887994223181167, -21.73372354711506560, 61.75568132718285597 ) ) ;
#37724 = AXIS2_PLACEMENT_3D ( 'NONE', #48453, #18408, #18914 ) ;
#37725 = DIRECTION ( 'NONE',  ( -0.5420872618288282707, -0.8403222004463035688, 7.592316861452269267E-08 ) ) ;
#37726 = AXIS2_PLACEMENT_3D ( 'NONE', #4636, #4393, #15948 ) ;
#37727 = ORIENTED_EDGE ( 'NONE', *, *, #27008, .F. ) ;
#37728 = DIRECTION ( 'NONE',  ( -0.9132646967824438189, 0.4073666574609055568, -8.344532079829881716E-09 ) ) ;
#37729 = CARTESIAN_POINT ( 'NONE',  ( -17.63103806674120833, -7.362028203752553068, 63.65782862784570284 ) ) ;
#37730 = VERTEX_POINT ( 'NONE', #35284 ) ;
#37731 = CARTESIAN_POINT ( 'NONE',  ( -18.95534385759798823, -8.623186033802570094, 49.24843789510466507 ) ) ;
#37732 = CARTESIAN_POINT ( 'NONE',  ( -16.60134452727454146, -19.99433755013348701, 49.52966884056656482 ) ) ;
#37733 = ORIENTED_EDGE ( 'NONE', *, *, #22073, .F. ) ;
#37734 = CARTESIAN_POINT ( 'NONE',  ( -23.46741908093438767, -19.16603997859080266, 62.53902161361033052 ) ) ;
#37735 = CARTESIAN_POINT ( 'NONE',  ( -21.42336286209559759, -21.09487474236010485, 69.23945462178221533 ) ) ;
#37736 = EDGE_CURVE ( 'NONE', #13753, #14422, #11141, .T. ) ;
#37737 = CARTESIAN_POINT ( 'NONE',  ( -17.23043714677651295, -7.361597588792181845, 70.61318921025367956 ) ) ;
#37738 = ORIENTED_EDGE ( 'NONE', *, *, #20604, .F. ) ;
#37739 = CARTESIAN_POINT ( 'NONE',  ( -10.73142062415649711, -12.58174813459350538, 64.36016235006516695 ) ) ;
#37740 = CARTESIAN_POINT ( 'NONE',  ( -20.51116909090755769, -10.56274136881318526, 50.77966884056655772 ) ) ;
#37741 = AXIS2_PLACEMENT_3D ( 'NONE', #19707, #9357, #23655 ) ;
#37742 = AXIS2_PLACEMENT_3D ( 'NONE', #6260, #13383, #43457 ) ;
#37743 = CARTESIAN_POINT ( 'NONE',  ( -24.24394117090890788, -12.99133827687660059, 59.51834745271546723 ) ) ;
#37744 = FACE_OUTER_BOUND ( 'NONE', #912, .T. ) ;
#37745 = EDGE_LOOP ( 'NONE', ( #19722, #14043, #41782, #19370, #42670 ) ) ;
#37746 = CARTESIAN_POINT ( 'NONE',  ( -24.69852180232685157, -16.41745880042978101, 59.30827708941524889 ) ) ;
#37747 = DIRECTION ( 'NONE',  ( 0.9687793358424821033, -0.2479245821708680464, 0.000000000000000000 ) ) ;
#37748 = VECTOR ( 'NONE', #22333, 1000.000000000000227 ) ;
#37749 = CARTESIAN_POINT ( 'NONE',  ( 18.62590614458706995, 1.890747609047893185, 50.53028072113869484 ) ) ;
#37750 = PLANE ( 'NONE',  #47045 ) ;
#37751 = CARTESIAN_POINT ( 'NONE',  ( -20.93476986463577916, -20.86527884399460220, 62.34144714227700490 ) ) ;
#37752 = CARTESIAN_POINT ( 'NONE',  ( -21.20554785340111081, -20.76353671134526380, 65.79273731141989856 ) ) ;
#37753 = CARTESIAN_POINT ( 'NONE',  ( -18.30534385650551599, -8.801233750844183135, 48.81488406609782515 ) ) ;
#37754 = ORIENTED_EDGE ( 'NONE', *, *, #30003, .F. ) ;
#37755 = CARTESIAN_POINT ( 'NONE',  ( -24.65061889199765233, -12.99785316138012270, 62.87618224063605510 ) ) ;
#37756 = FACE_OUTER_BOUND ( 'NONE', #1456, .T. ) ;
#37757 = ORIENTED_EDGE ( 'NONE', *, *, #41060, .F. ) ;
#37758 = LINE ( 'NONE', #18810, #11933 ) ;
#37759 = VECTOR ( 'NONE', #17888, 1000.000000000000000 ) ;
#37760 = CARTESIAN_POINT ( 'NONE',  ( -24.44055745662519641, -14.11932379769929113, 73.13743607903229815 ) ) ;
#37761 = CARTESIAN_POINT ( 'NONE',  ( -18.03441950114640235, -20.28875745248266327, 53.69233794759168887 ) ) ;
#37762 =( BOUNDED_CURVE ( )  B_SPLINE_CURVE ( 3, ( #6138, #25338, #14221, #43578 ),
 .UNSPECIFIED., .F., .F. ) 
 B_SPLINE_CURVE_WITH_KNOTS ( ( 4, 4 ),
 ( 0.4074455897393596815, 0.5000000000000000000 ),
 .UNSPECIFIED. ) 
 CURVE ( )  GEOMETRIC_REPRESENTATION_ITEM ( )  RATIONAL_B_SPLINE_CURVE ( ( 0.6983129098260858481, 0.7760317562606769970, 0.8765941196519771994, 0.9999999999999761302 ) ) 
 REPRESENTATION_ITEM ( '' )  );
#37763 = ORIENTED_EDGE ( 'NONE', *, *, #25012, .F. ) ;
#37764 = CARTESIAN_POINT ( 'NONE',  ( -18.64625997845222116, -21.76055708611507100, 68.97081679896227513 ) ) ;
#37765 = EDGE_CURVE ( 'NONE', #2504, #3256, #16316, .T. ) ;
#37766 = CARTESIAN_POINT ( 'NONE',  ( -10.40035142239662669, -15.50347837920617167, 64.65204674534754758 ) ) ;
#37767 = CARTESIAN_POINT ( 'NONE',  ( -23.48338609245114483, -18.31419979820022448, 72.87254147078147071 ) ) ;
#37768 = ADVANCED_FACE ( 'NONE', ( #38743 ), #38984, .T. ) ;
#37769 = EDGE_CURVE ( 'NONE', #42856, #25718, #31111, .T. ) ;
#37770 = ORIENTED_EDGE ( 'NONE', *, *, #26736, .F. ) ;
#37771 = CARTESIAN_POINT ( 'NONE',  ( -14.36784385650551954, -6.428312510596451368, 51.20221977374900035 ) ) ;
#37772 = CARTESIAN_POINT ( 'NONE',  ( -14.39270380832417295, -8.498217223279159072, 70.80127861885151219 ) ) ;
#37773 = CARTESIAN_POINT ( 'NONE',  ( -13.27770617114843965, -9.107455183738579763, 64.05946529205222362 ) ) ;
#37774 = CARTESIAN_POINT ( 'NONE',  ( -24.85414368999009938, -14.26268454367973781, 69.83088022027575903 ) ) ;
#37775 = CARTESIAN_POINT ( 'NONE',  ( -16.97945985512182787, -21.84517132341290591, 72.16543221430227106 ) ) ;
#37776 =( BOUNDED_SURFACE ( )  B_SPLINE_SURFACE ( 3, 1, ( 
 ( #20336, #24278 ),
 ( #42983, #9255 ),
 ( #39288, #35345 ),
 ( #2097, #5571 ),
 ( #6035, #20586 ),
 ( #35583, #13407 ),
 ( #43483, #12451 ) ),
 .UNSPECIFIED., .T., .F., .F. ) 
 B_SPLINE_SURFACE_WITH_KNOTS ( ( 4, 3, 4 ),
 ( 2, 2 ),
 ( 0.000000000000000000, 0.5000000000000000000, 1.000000000000000000 ),
 ( 0.000000000000000000, 1.000000000000000000 ),
 .UNSPECIFIED. ) 
 GEOMETRIC_REPRESENTATION_ITEM ( )  RATIONAL_B_SPLINE_SURFACE ( (
 ( 1.000000000000000000, 1.000000000000000000),
 ( 0.3333333333333335369, 0.3333333333333330373),
 ( 0.3333333333333335369, 0.3333333333333330373),
 ( 1.000000000000000000, 1.000000000000000000),
 ( 0.3333333333333333703, 0.3333333333333333703),
 ( 0.3333333333333333703, 0.3333333333333333703),
 ( 1.000000000000000000, 1.000000000000000000) ) ) 
 REPRESENTATION_ITEM ( '' )  SURFACE ( )  );
#37777 = EDGE_LOOP ( 'NONE', ( #40456, #434, #16994, #17110, #14398, #33980, #19860 ) ) ;
#37778 = VERTEX_POINT ( 'NONE', #20281 ) ;
#37779 = EDGE_CURVE ( 'NONE', #3121, #8094, #16833, .T. ) ;
#37780 = CARTESIAN_POINT ( 'NONE',  ( -15.35534385650551847, -7.417179338643134834, 52.18511593390279302 ) ) ;
#37781 = AXIS2_PLACEMENT_3D ( 'NONE', #18106, #33124, #48163 ) ;
#37782 = LINE ( 'NONE', #23512, #34706 ) ;
#37783 = CARTESIAN_POINT ( 'NONE',  ( -13.46747565276156422, -9.034678650756244878, 60.73950277887485072 ) ) ;
#37784 = CARTESIAN_POINT ( 'NONE',  ( -15.46784385650551918, -6.428312510596451368, 51.20221977374900035 ) ) ;
#37785 = VECTOR ( 'NONE', #15333, 1000.000000000000114 ) ;
#37786 =( BOUNDED_SURFACE ( )  B_SPLINE_SURFACE ( 3, 1, ( 
 ( #37917, #46223 ),
 ( #24065, #1393 ),
 ( #8813, #33974 ),
 ( #5350, #39316 ),
 ( #35128, #16410 ),
 ( #4202, #19209 ),
 ( #15249, #272 ) ),
 .UNSPECIFIED., .T., .F., .F. ) 
 B_SPLINE_SURFACE_WITH_KNOTS ( ( 4, 3, 4 ),
 ( 2, 2 ),
 ( 0.000000000000000000, 0.5000000000000000000, 1.000000000000000000 ),
 ( 0.000000000000000000, 1.000000000000000000 ),
 .UNSPECIFIED. ) 
 GEOMETRIC_REPRESENTATION_ITEM ( )  RATIONAL_B_SPLINE_SURFACE ( (
 ( 1.000000000000000000, 1.000000000000000000),
 ( 0.3333333333333335369, 0.3333333333333330373),
 ( 0.3333333333333335369, 0.3333333333333330373),
 ( 1.000000000000000000, 1.000000000000000000),
 ( 0.3333333333333333703, 0.3333333333333333703),
 ( 0.3333333333333333703, 0.3333333333333333703),
 ( 1.000000000000000000, 1.000000000000000000) ) ) 
 REPRESENTATION_ITEM ( '' )  SURFACE ( )  );
#37787 = CARTESIAN_POINT ( 'NONE',  ( -45.92409385541306222, -17.80920654474411435, 70.50000000000000000 ) ) ;
#37788 = EDGE_CURVE ( 'NONE', #32695, #32895, #39909, .T. ) ;
#37789 = CARTESIAN_POINT ( 'NONE',  ( -10.69992066440855361, -12.66433694503948004, 67.88265386532016521 ) ) ;
#37790 = FACE_OUTER_BOUND ( 'NONE', #18077, .T. ) ;
#37791 = AXIS2_PLACEMENT_3D ( 'NONE', #7344, #2888, #22590 ) ;
#37792 = CARTESIAN_POINT ( 'NONE',  ( -23.77562434277295367, -17.86939608417919345, 59.01850491586762359 ) ) ;
#37793 = ORIENTED_EDGE ( 'NONE', *, *, #48471, .F. ) ;
#37794 = DIRECTION ( 'NONE',  ( 0.000000000000000000, 0.000000000000000000, 1.000000000000000000 ) ) ;
#37795 = VERTEX_POINT ( 'NONE', #39478 ) ;
#37796 = CARTESIAN_POINT ( 'NONE',  ( -12.57352595576265308, -9.154542183914287534, 74.51261323680796522 ) ) ;
#37797 = CARTESIAN_POINT ( 'NONE',  ( -12.56341008138639026, -9.163283831748978869, 74.41948763787014798 ) ) ;
#37798 = CARTESIAN_POINT ( 'NONE',  ( -11.36918367646109651, -19.26602422791083669, 53.76227901944321275 ) ) ;
#37799 = AXIS2_PLACEMENT_3D ( 'NONE', #7389, #22389, #45304 ) ;
#37800 = ORIENTED_EDGE ( 'NONE', *, *, #23270, .T. ) ;
#37801 = CARTESIAN_POINT ( 'NONE',  ( -17.84478125091072087, -22.24806977446377942, 62.06191208170499607 ) ) ;
#37802 = CARTESIAN_POINT ( 'NONE',  ( -24.20525988284104457, -11.72391474569057124, 59.67574024123567256 ) ) ;
#37803 = CARTESIAN_POINT ( 'NONE',  ( -21.02292652713908794, -10.98678540089889921, 50.77966884056655772 ) ) ;
#37804 = CYLINDRICAL_SURFACE ( 'NONE', #111, 0.1499999999999956923 ) ;
#37805 = ORIENTED_EDGE ( 'NONE', *, *, #12701, .T. ) ;
#37806 = DIRECTION ( 'NONE',  ( -3.071710424422018668E-17, 6.404604876783312462E-16, 1.000000000000000000 ) ) ;
#37807 = FACE_OUTER_BOUND ( 'NONE', #14902, .T. ) ;
#37808 = B_SPLINE_CURVE_WITH_KNOTS ( 'NONE', 3,
 ( #44909, #23220, #34273, #11162, #11636, #563, #22739, #41928, #37729, #26668 ),
 .UNSPECIFIED., .F., .F.,
 ( 4, 2, 2, 2, 4 ),
 ( 0.6272669072976760907, 0.7522669073147278951, 0.8772669073317798105, 1.002266907348831726, 1.127266907365883419 ),
 .UNSPECIFIED. ) ;
#37809 = FACE_OUTER_BOUND ( 'NONE', #46738, .T. ) ;
#37810 = FACE_BOUND ( 'NONE', #35098, .T. ) ;
#37811 = ITEM_DEFINED_TRANSFORMATION ( 'NONE', 'NONE', #6240,  #29031 ) ;
#37812 = B_SPLINE_CURVE_WITH_KNOTS ( 'NONE', 3,
 ( #28101, #2000, #9156, #1765, #43127, #47063, #13300, #35482, #16760, #42411 ),
 .UNSPECIFIED., .F., .F.,
 ( 4, 2, 2, 2, 4 ),
 ( 0.000000000000000000, 0.2500000000000000000, 0.5000000000000000000, 0.7500000000000000000, 1.000000000000000000 ),
 .UNSPECIFIED. ) ;
#37813 = EDGE_LOOP ( 'NONE', ( #7481, #17802, #46775, #18288, #3688 ) ) ;
#37814 = AXIS2_PLACEMENT_3D ( 'NONE', #25077, #43057, #5651 ) ;
#37815 = FACE_OUTER_BOUND ( 'NONE', #11127, .T. ) ;
#37816 = CARTESIAN_POINT ( 'NONE',  ( -17.42409385541299471, -14.80920654474435771, 49.52966884056655772 ) ) ;
#37817 = CARTESIAN_POINT ( 'NONE',  ( -23.62573085457600541, -18.93877797592854506, 65.93734031310268051 ) ) ;
#37818 = CIRCLE ( 'NONE', #29178, 2.404255319148937531 ) ;
#37819 = CARTESIAN_POINT ( 'NONE',  ( -14.53659385541304694, -8.995762431863209230, 51.38120296130584563 ) ) ;
#37820 = ORIENTED_EDGE ( 'NONE', *, *, #29619, .T. ) ;
#37821 = CARTESIAN_POINT ( 'NONE',  ( -10.44483699753067718, -14.26928449077156813, 64.68803882970183849 ) ) ;
#37822 = VERTEX_POINT ( 'NONE', #12643 ) ;
#37823 = FACE_OUTER_BOUND ( 'NONE', #29034, .T. ) ;
#37824 = LINE ( 'NONE', #4119, #19623 ) ;
#37825 = ORIENTED_EDGE ( 'NONE', *, *, #44769, .F. ) ;
#37826 = CARTESIAN_POINT ( 'NONE',  ( -18.33709340422855050, -22.20310063599641381, 69.00853016400594697 ) ) ;
#37827 = ORIENTED_EDGE ( 'NONE', *, *, #32856, .T. ) ;
#37828 = ADVANCED_FACE ( 'NONE', ( #16567 ), #46866, .T. ) ;
#37829 = VERTEX_POINT ( 'NONE', #17039 ) ;
#37830 = EDGE_LOOP ( 'NONE', ( #14835, #42503, #42138, #10635, #26833 ) ) ;
#37831 = CARTESIAN_POINT ( 'NONE',  ( -18.29367245688808552, -17.15309925898211318, 75.49999999999994316 ) ) ;
#37832 = CARTESIAN_POINT ( 'NONE',  ( -22.86572475812252847, -14.01004878893095196, 53.49999999999995026 ) ) ;
#37833 = AXIS2_PLACEMENT_3D ( 'NONE', #10368, #17490, #47549 ) ;
#37834 = DIRECTION ( 'NONE',  ( 0.06357898915123481876, -0.9979768094191904249, 0.000000000000000000 ) ) ;
#37835 = FACE_OUTER_BOUND ( 'NONE', #34785, .T. ) ;
#37836 = CARTESIAN_POINT ( 'NONE',  ( -24.17271927670314113, -12.95015993349377048, 66.30246741691458112 ) ) ;
#37837 = CARTESIAN_POINT ( 'NONE',  ( -14.09914604623946488, -8.649277798895779412, 74.19954655170327840 ) ) ;
#37838 = CARTESIAN_POINT ( 'NONE',  ( -12.50249420765911701, -20.40225435000794008, 71.98466421126660464 ) ) ;
#37839 = EDGE_LOOP ( 'NONE', ( #40325, #29359, #5502, #29458, #20308 ) ) ;
#37840 = EDGE_LOOP ( 'NONE', ( #25552, #15338, #41551, #18632, #2989 ) ) ;
#37841 = EDGE_CURVE ( 'NONE', #17387, #18626, #48420, .T. ) ;
#37842 = EDGE_CURVE ( 'NONE', #10553, #10266, #45780, .T. ) ;
#37843 = CARTESIAN_POINT ( 'NONE',  ( -12.09292629619409531, -10.27274204020369197, 64.25587718757367384 ) ) ;
#37844 = AXIS2_PLACEMENT_3D ( 'NONE', #48646, #26244, #25510 ) ;
#37845 = ADVANCED_FACE ( 'NONE', ( #32339 ), #25905, .F. ) ;
#37846 = CARTESIAN_POINT ( 'NONE',  ( -16.87780900865216438, -10.15465445929086208, 49.52966884056655772 ) ) ;
#37847 = CARTESIAN_POINT ( 'NONE',  ( -10.52991701743181174, -16.02177613136639067, 67.97767831076122036 ) ) ;
#37848 = EDGE_CURVE ( 'NONE', #48456, #39905, #6428, .T. ) ;
#37849 = VERTEX_POINT ( 'NONE', #6229 ) ;
#37850 = CARTESIAN_POINT ( 'NONE',  ( -16.05534385650551243, -7.417179338643134834, 52.18511593390279302 ) ) ;
#37851 = ORIENTED_EDGE ( 'NONE', *, *, #1831, .F. ) ;
#37852 = VECTOR ( 'NONE', #33705, 1000.000000000000227 ) ;
#37853 = CARTESIAN_POINT ( 'NONE',  ( -16.20683463515880973, -21.70255690700738782, 58.28585572422844052 ) ) ;
#37854 = EDGE_CURVE ( 'NONE', #25105, #19438, #36963, .T. ) ;
#37855 = CARTESIAN_POINT ( 'NONE',  ( -15.42745694218142027, -21.51847616057531809, 68.80266276951817872 ) ) ;
#37856 = VECTOR ( 'NONE', #39223, 1000.000000000000000 ) ;
#37857 = CARTESIAN_POINT ( 'NONE',  ( -15.29809632361469873, -21.47854941203162937, 68.57592918283285144 ) ) ;
#37858 = ORIENTED_EDGE ( 'NONE', *, *, #33209, .T. ) ;
#37859 = CARTESIAN_POINT ( 'NONE',  ( -13.33852097861372421, -12.48893720396535478, 49.52966884056655772 ) ) ;
#37860 = CARTESIAN_POINT ( 'NONE',  ( -15.76027622468541978, -7.547319663497244591, 67.33281406147084169 ) ) ;
#37861 = CARTESIAN_POINT ( 'NONE',  ( -12.10369346210734243, -9.594120923840563364, 57.27430859790474926 ) ) ;
#37862 = ORIENTED_EDGE ( 'NONE', *, *, #11299, .T. ) ;
#37863 = VECTOR ( 'NONE', #30910, 1000.000000000000114 ) ;
#37864 = FACE_OUTER_BOUND ( 'NONE', #28250, .T. ) ;
#37865 = B_SPLINE_CURVE_WITH_KNOTS ( 'NONE', 1,
 ( #8071, #23080 ),
 .UNSPECIFIED., .F., .F.,
 ( 2, 2 ),
 ( 0.000000000000000000, 1.000000000000000000 ),
 .UNSPECIFIED. ) ;
#37866 = LINE ( 'NONE', #29758, #7878 ) ;
#37867 = DIRECTION ( 'NONE',  ( 0.9893874368562762811, -0.1453014101478983522, 1.482692748682355818E-17 ) ) ;
#37868 = EDGE_LOOP ( 'NONE', ( #7756, #41110, #38264 ) ) ;
#37869 = CARTESIAN_POINT ( 'NONE',  ( -10.50466007945005487, -15.86899602918702001, 64.80771547851877301 ) ) ;
#37870 = ORIENTED_EDGE ( 'NONE', *, *, #13422, .F. ) ;
#37871 = CARTESIAN_POINT ( 'NONE',  ( -14.77897477670383353, -8.270997283837589364, 56.73511376018900876 ) ) ;
#37872 = ORIENTED_EDGE ( 'NONE', *, *, #25817, .F. ) ;
#37873 = CARTESIAN_POINT ( 'NONE',  ( 18.46573386768564973, 2.137037847100790255, 51.75577699556767897 ) ) ;
#37874 = CARTESIAN_POINT ( 'NONE',  ( -24.55824875695236287, -12.66269769826935310, 70.02888935069151444 ) ) ;
#37875 = VECTOR ( 'NONE', #33002, 1000.000000000000000 ) ;
#37876 = CARTESIAN_POINT ( 'NONE',  ( -11.46780417137699004, -10.33417537808259823, 74.54610936257664378 ) ) ;
#37877 = VERTEX_POINT ( 'NONE', #17768 ) ;
#37878 = CARTESIAN_POINT ( 'NONE',  ( -22.11926001268504294, -9.024814352312150234, 63.30658345311071855 ) ) ;
#37879 = EDGE_CURVE ( 'NONE', #22956, #31810, #3252, .T. ) ;
#37880 = LINE ( 'NONE', #30990, #771 ) ;
#37881 = CARTESIAN_POINT ( 'NONE',  ( -10.92393591598462166, -17.40806730853362794, 68.11338529727301250 ) ) ;
#37882 = EDGE_LOOP ( 'NONE', ( #15619, #18217, #9104, #31697 ) ) ;
#37883 = CARTESIAN_POINT ( 'NONE',  ( -19.24513076412772961, -8.048561166981372139, 63.54162403522450830 ) ) ;
#37884 = CARTESIAN_POINT ( 'NONE',  ( -18.76558283008973049, -7.480892646508040755, 70.55563411965815135 ) ) ;
#37885 = VECTOR ( 'NONE', #32471, 1000.000000000000000 ) ;
#37886 = EDGE_CURVE ( 'NONE', #22122, #27032, #6476, .T. ) ;
#37887 = ORIENTED_EDGE ( 'NONE', *, *, #11515, .F. ) ;
#37888 = EDGE_LOOP ( 'NONE', ( #26547, #5575 ) ) ;
#37889 = VECTOR ( 'NONE', #43923, 1000.000000000000000 ) ;
#37890 = DIRECTION ( 'NONE',  ( -3.071710424422018668E-17, 6.404604876783312462E-16, 1.000000000000000000 ) ) ;
#37891 = CARTESIAN_POINT ( 'NONE',  ( -19.40534385759799463, -7.595227055684746986, 51.75156210489594599 ) ) ;
#37892 = DIRECTION ( 'NONE',  ( -9.352133734048191489E-06, -6.779811745274577181E-06, -0.9999999999332859213 ) ) ;
#37893 = DIRECTION ( 'NONE',  ( 1.927470528863184130E-16, 1.434740771370715221E-29, -1.000000000000000000 ) ) ;
#37894 = CARTESIAN_POINT ( 'NONE',  ( -22.35534385650551670, -7.417179338643134834, 52.18511593390279302 ) ) ;
#37895 = CARTESIAN_POINT ( 'NONE',  ( -10.59656512619885227, -13.05092609425065397, 68.02360230423870746 ) ) ;
#37896 = CARTESIAN_POINT ( 'NONE',  ( -12.35277413765887999, -20.26681541663451114, 68.45162113748973809 ) ) ;
#37897 = DIRECTION ( 'NONE',  ( 1.000000000000000000, -4.164305804376849172E-17, 1.614929280266638808E-16 ) ) ;
#37898 = CARTESIAN_POINT ( 'NONE',  ( -17.65006842549283306, -20.30456235612524196, 53.49999999999995026 ) ) ;
#37899 = ORIENTED_EDGE ( 'NONE', *, *, #1140, .F. ) ;
#37900 = CYLINDRICAL_SURFACE ( 'NONE', #21070, 0.1500000000000019651 ) ;
#37901 = ADVANCED_FACE ( 'NONE', ( #21967 ), #40206, .T. ) ;
#37902 = LINE ( 'NONE', #42335, #32726 ) ;
#37903 = CARTESIAN_POINT ( 'NONE',  ( -21.95938932932862642, -9.477124872050278981, 60.02171213236835712 ) ) ;
#37904 = EDGE_CURVE ( 'NONE', #40815, #38501, #27080, .T. ) ;
#37905 = EDGE_LOOP ( 'NONE', ( #37229, #41500 ) ) ;
#37906 = EDGE_CURVE ( 'NONE', #28606, #26764, #14724, .T. ) ;
#37907 = ORIENTED_EDGE ( 'NONE', *, *, #42657, .T. ) ;
#37908 = DIRECTION ( 'NONE',  ( 0.4433615477241707459, -0.8963428685495451465, 2.661652803430218851E-08 ) ) ;
#37909 = CARTESIAN_POINT ( 'NONE',  ( -13.30562964713168306, -21.01738586623506677, 61.70984649199183991 ) ) ;
#37910 = DIRECTION ( 'NONE',  ( -0.1453014101478919129, -0.9893874368562773913, 2.030021817369025738E-16 ) ) ;
#37911 = EDGE_CURVE ( 'NONE', #5353, #4057, #28752, .T. ) ;
#37912 =( BOUNDED_SURFACE ( )  B_SPLINE_SURFACE ( 3, 1, ( 
 ( #36040, #29151 ),
 ( #47394, #36748 ),
 ( #21038, #3037 ),
 ( #3292, #17569 ),
 ( #36515, #24977 ),
 ( #21292, #2322 ),
 ( #10679, #28906 ) ),
 .UNSPECIFIED., .T., .F., .F. ) 
 B_SPLINE_SURFACE_WITH_KNOTS ( ( 4, 3, 4 ),
 ( 2, 2 ),
 ( 0.000000000000000000, 0.5000000000000000000, 1.000000000000000000 ),
 ( 0.000000000000000000, 1.000000000000000000 ),
 .UNSPECIFIED. ) 
 GEOMETRIC_REPRESENTATION_ITEM ( )  RATIONAL_B_SPLINE_SURFACE ( (
 ( 1.000000000000000000, 1.000000000000000000),
 ( 0.3333333333333335369, 0.3333333333333330373),
 ( 0.3333333333333335369, 0.3333333333333330373),
 ( 1.000000000000000000, 1.000000000000000000),
 ( 0.3333333333333333703, 0.3333333333333333703),
 ( 0.3333333333333333703, 0.3333333333333333703),
 ( 1.000000000000000000, 1.000000000000000000) ) ) 
 REPRESENTATION_ITEM ( '' )  SURFACE ( )  );
#37913 = VERTEX_POINT ( 'NONE', #13592 ) ;
#37914 = CARTESIAN_POINT ( 'NONE',  ( -24.47354778464749003, -12.39902454472287197, 73.42720984402279782 ) ) ;
#37915 = CARTESIAN_POINT ( 'NONE',  ( -14.48548941065490148, -8.400516866317895293, 67.27447142263336843 ) ) ;
#37916 = ORIENTED_EDGE ( 'NONE', *, *, #36050, .T. ) ;
#37917 = CARTESIAN_POINT ( 'NONE',  ( -22.48964968825576705, -9.905448439006629968, 73.76689030015370463 ) ) ;
#37918 = CARTESIAN_POINT ( 'NONE',  ( -24.45320359087931550, -14.22178767528806276, 66.39112731077266005 ) ) ;
#37919 = CARTESIAN_POINT ( 'NONE',  ( -11.96181431063714484, -19.87549516500596525, 58.11177798925346139 ) ) ;
#37920 = ORIENTED_EDGE ( 'NONE', *, *, #1683, .F. ) ;
#37921 = LINE ( 'NONE', #30319, #19694 ) ;
#37922 =( BOUNDED_CURVE ( )  B_SPLINE_CURVE ( 3, ( #36851, #6603, #18148, #47963 ),
 .UNSPECIFIED., .F., .F. ) 
 B_SPLINE_CURVE_WITH_KNOTS ( ( 4, 4 ),
 ( 0.5000000000000000000, 0.9074455897393689519 ),
 .UNSPECIFIED. ) 
 CURVE ( )  GEOMETRIC_REPRESENTATION_ITEM ( )  RATIONAL_B_SPLINE_CURVE ( ( 0.9999999999999958922, 0.4567392136813261949, 0.3561768502900309885, 0.6983129098261057210 ) ) 
 REPRESENTATION_ITEM ( '' )  );
#37923 = EDGE_LOOP ( 'NONE', ( #17081, #25511, #5628, #21575, #31453 ) ) ;
#37924 = DIRECTION ( 'NONE',  ( -1.295331064632368052E-06, 6.890485867068654572E-07, 0.9999999999989236388 ) ) ;
#37925 = CARTESIAN_POINT ( 'NONE',  ( -41.67625132147640699, -14.90920654474424190, 68.98274027149319920 ) ) ;
#37926 = ORIENTED_EDGE ( 'NONE', *, *, #35850, .F. ) ;
#37927 = CARTESIAN_POINT ( 'NONE',  ( -13.35550522631041837, -8.568183888810063209, 57.15463030501995689 ) ) ;
#37928 = CARTESIAN_POINT ( 'NONE',  ( -24.32420487361504868, -13.34567816304479848, 62.92444446668879721 ) ) ;
#37929 = CARTESIAN_POINT ( 'NONE',  ( -21.48659385650551457, -9.302874398569244363, 51.68646062012417985 ) ) ;
#37930 = DIRECTION ( 'NONE',  ( -8.563106570025498363E-06, 6.519502999113576510E-06, -0.9999999999420846608 ) ) ;
#37931 = EDGE_CURVE ( 'NONE', #39283, #7665, #8799, .T. ) ;
#37932 = DIRECTION ( 'NONE',  ( -3.071710424422018668E-17, 6.404604876783312462E-16, 1.000000000000000000 ) ) ;
#37933 = CARTESIAN_POINT ( 'NONE',  ( -24.43827367352892210, -15.52193379869737200, 73.28831629023289906 ) ) ;
#37934 = CARTESIAN_POINT ( 'NONE',  ( -13.41559485503361948, -8.529420403834853559, 57.08472365561223683 ) ) ;
#37935 = EDGE_LOOP ( 'NONE', ( #13979, #32190, #7300, #22171, #26651 ) ) ;
#37936 = CARTESIAN_POINT ( 'NONE',  ( -11.79792781917550570, -18.97409009807959279, 71.68685885149984927 ) ) ;
#37937 = CARTESIAN_POINT ( 'NONE',  ( -13.10977233404386944, -20.39504592733330313, 58.19083229533344337 ) ) ;
#37938 = PLANE ( 'NONE',  #45486 ) ;
#37939 = LINE ( 'NONE', #294, #36855 ) ;
#37940 = CARTESIAN_POINT ( 'NONE',  ( -23.79763979734637402, -18.66673721458791491, 72.96357004385932044 ) ) ;
#37941 = EDGE_LOOP ( 'NONE', ( #43059, #6503, #37305, #39719 ) ) ;
#37942 = ORIENTED_EDGE ( 'NONE', *, *, #31508, .T. ) ;
#37943 = CARTESIAN_POINT ( 'NONE',  ( -18.86321414053259105, -7.899510124550229051, 73.98497555292401273 ) ) ;
#37944 = DIRECTION ( 'NONE',  ( -0.8447509909909768355, 0.5351595679979597175, 0.000000000000000000 ) ) ;
#37945 = ORIENTED_EDGE ( 'NONE', *, *, #46096, .F. ) ;
#37946 = CARTESIAN_POINT ( 'NONE',  ( -24.00225416124087374, -17.20718635581271272, 72.99409062911038859 ) ) ;
#37947 = CARTESIAN_POINT ( 'NONE',  ( -15.26209398273251772, -21.93938324809698770, 68.68937616499954402 ) ) ;
#37948 = CARTESIAN_POINT ( 'NONE',  ( -21.31784385759798539, -6.860780111191487229, 51.02154966934377001 ) ) ;
#37949 = LINE ( 'NONE', #4236, #24243 ) ;
#37950 = FACE_OUTER_BOUND ( 'NONE', #27595, .T. ) ;
#37951 = CARTESIAN_POINT ( 'NONE',  ( -22.38400322090610217, -20.36826016184844335, 62.41934579407823236 ) ) ;
#37952 = CARTESIAN_POINT ( 'NONE',  ( -17.42409385541299471, -14.80920654474435594, 52.02966884056656482 ) ) ;
#37953 = FACE_OUTER_BOUND ( 'NONE', #25622, .T. ) ;
#37954 = DIRECTION ( 'NONE',  ( 1.000000000000000000, 2.866981220435666553E-17, 0.000000000000000000 ) ) ;
#37955 = EDGE_CURVE ( 'NONE', #33080, #31526, #9924, .T. ) ;
#37956 = DIRECTION ( 'NONE',  ( 2.866981220435666553E-17, -1.000000000000000000, -1.190614954331866791E-16 ) ) ;
#37957 = CARTESIAN_POINT ( 'NONE',  ( -24.32886716615087153, -16.23426984194678724, 62.60800820172418923 ) ) ;
#37958 = CARTESIAN_POINT ( 'NONE',  ( -11.82099749022622426, -9.899105802180386604, 64.21409645106085406 ) ) ;
#37959 = B_SPLINE_CURVE_WITH_KNOTS ( 'NONE', 3,
 ( #13156, #35815, #6032, #13643, #2341, #28684, #1612, #24994, #43968, #47644 ),
 .UNSPECIFIED., .F., .F.,
 ( 4, 2, 2, 2, 4 ),
 ( 0.000000000000000000, 0.2500000000000000000, 0.5000000000000000000, 0.7500000000000000000, 1.000000000000000000 ),
 .UNSPECIFIED. ) ;
#37960 = FACE_BOUND ( 'NONE', #23914, .T. ) ;
#37961 = ORIENTED_EDGE ( 'NONE', *, *, #2705, .T. ) ;
#37962 = EDGE_LOOP ( 'NONE', ( #32193, #17794, #26702, #16265, #36908 ) ) ;
#37963 = CARTESIAN_POINT ( 'NONE',  ( -20.16691211377460391, -21.73601867580754288, 72.58974061177721637 ) ) ;
#37964 = ADVANCED_FACE ( 'NONE', ( #21254 ), #19822, .T. ) ;
#37965 = ORIENTED_EDGE ( 'NONE', *, *, #31552, .F. ) ;
#37966 = FACE_OUTER_BOUND ( 'NONE', #32300, .T. ) ;
#37967 = CARTESIAN_POINT ( 'NONE',  ( -21.62565899036455264, -11.23921691435401904, 53.88362224778187226 ) ) ;
#37968 = ADVANCED_FACE ( 'NONE', ( #307 ), #14783, .T. ) ;
#37969 = CARTESIAN_POINT ( 'NONE',  ( -13.34909364474977522, -8.572319965759302107, 57.14684612213136461 ) ) ;
#37970 = CARTESIAN_POINT ( 'NONE',  ( -16.91478550490786503, -21.84108428878278119, 72.18015306840750611 ) ) ;
#37971 = VECTOR ( 'NONE', #10911, 1000.000000000000227 ) ;
#37972 = VERTEX_POINT ( 'NONE', #26389 ) ;
#37973 = CARTESIAN_POINT ( 'NONE',  ( -13.87299615820197296, -20.90301826156740717, 72.34096506744559463 ) ) ;
#37974 = ORIENTED_EDGE ( 'NONE', *, *, #21210, .T. ) ;
#37975 = CARTESIAN_POINT ( 'NONE',  ( -22.37828812292848824, -20.37331024823514980, 62.42713317377827309 ) ) ;
#37976 = EDGE_CURVE ( 'NONE', #4804, #6954, #12871, .T. ) ;
#37977 = CARTESIAN_POINT ( 'NONE',  ( -23.98474789688958353, -17.25007084823549874, 69.71339792561613535 ) ) ;
#37978 = EDGE_CURVE ( 'NONE', #12756, #14479, #45849, .T. ) ;
#37979 = ORIENTED_EDGE ( 'NONE', *, *, #1038, .T. ) ;
#37980 = CARTESIAN_POINT ( 'NONE',  ( -24.87450840884172365, -14.73858704721042123, 59.35644987740099765 ) ) ;
#37981 = CARTESIAN_POINT ( 'NONE',  ( -11.05753579597473113, -11.89914114276540680, 74.55840159191156147 ) ) ;
#37982 = CARTESIAN_POINT ( 'NONE',  ( -18.75492427513048455, -7.882278092513721468, 73.93244671259982681 ) ) ;
#37983 = EDGE_CURVE ( 'NONE', #19518, #43128, #3995, .T. ) ;
#37984 = ORIENTED_EDGE ( 'NONE', *, *, #42422, .F. ) ;
#37985 = CARTESIAN_POINT ( 'NONE',  ( -10.93089496422971330, -11.15644115613137188, 64.32694814133255079 ) ) ;
#37986 = CARTESIAN_POINT ( 'NONE',  ( -17.72612443559818018, -7.765381109175947927, 60.36588690973874094 ) ) ;
#37987 = EDGE_CURVE ( 'NONE', #24972, #10986, #24846, .T. ) ;
#37988 = CARTESIAN_POINT ( 'NONE',  ( -14.60079031338673516, -21.70357006634377584, 58.35892056026858654 ) ) ;
#37989 = CARTESIAN_POINT ( 'NONE',  ( -24.08517543038346531, -12.49907855475201579, 73.52753481283211556 ) ) ;
#37990 = VERTEX_POINT ( 'NONE', #37951 ) ;
#37991 = CARTESIAN_POINT ( 'NONE',  ( -11.45751978572037011, -19.27057081285444085, 71.87181161472111057 ) ) ;
#37992 = CARTESIAN_POINT ( 'NONE',  ( -24.38391081516821401, -14.06024225110868464, 73.12271507915593816 ) ) ;
#37993 = CARTESIAN_POINT ( 'NONE',  ( -11.07877888056294147, -17.89008669626860737, 71.56718224920616933 ) ) ;
#37994 = CARTESIAN_POINT ( 'NONE',  ( -23.56138519289638822, -11.33989039198723248, 69.89210750373884196 ) ) ;
#37995 = CARTESIAN_POINT ( 'NONE',  ( -13.82526118368687307, -18.63162768858978779, 49.52966884056656482 ) ) ;
#37996 = CARTESIAN_POINT ( 'NONE',  ( -19.88034385650552238, -6.424090610841176385, 49.80797279389978627 ) ) ;
#37997 = ORIENTED_EDGE ( 'NONE', *, *, #46963, .F. ) ;
#37998 = DIRECTION ( 'NONE',  ( 0.000000000000000000, 1.000000000000000000, -0.000000000000000000 ) ) ;
#37999 = CARTESIAN_POINT ( 'NONE',  ( -4.924093855413054222, -6.859206544744110623, 63.99999999999998579 ) ) ;
#38000 = VERTEX_POINT ( 'NONE', #34249 ) ;
#38001 = CARTESIAN_POINT ( 'NONE',  ( -11.30641337201207364, -19.06087391327494629, 68.31715392936506248 ) ) ;
#38002 = CARTESIAN_POINT ( 'NONE',  ( -22.52510391186153171, -10.01533143912503832, 73.48161092902591918 ) ) ;
#38003 = CARTESIAN_POINT ( 'NONE',  ( -14.67456088659309899, -21.24707878532894512, 58.45001277033151155 ) ) ;
#38004 = EDGE_LOOP ( 'NONE', ( #32482, #27949, #24043, #6438, #19651 ) ) ;
#38005 = FACE_OUTER_BOUND ( 'NONE', #8990, .T. ) ;
#38006 = CARTESIAN_POINT ( 'NONE',  ( -16.66933960180709917, -7.791706125978248743, 74.11585391104840426 ) ) ;
#38007 = CARTESIAN_POINT ( 'NONE',  ( -17.42409385541300892, -14.80920654474439679, 54.49999999999994316 ) ) ;
#38008 = ORIENTED_EDGE ( 'NONE', *, *, #21877, .T. ) ;
#38009 = AXIS2_PLACEMENT_3D ( 'NONE', #27816, #44014, #31518 ) ;
#38010 = CARTESIAN_POINT ( 'NONE',  ( -14.08659385650551776, -9.302874398569244363, 51.68646062012417985 ) ) ;
#38011 = CARTESIAN_POINT ( 'NONE',  ( -12.90354087724769272, -8.887350501024684490, 67.49447389996370816 ) ) ;
#38012 = CARTESIAN_POINT ( 'NONE',  ( -12.82854046268865034, -13.89041861240101206, 49.52966884056655772 ) ) ;
#38013 = CARTESIAN_POINT ( 'NONE',  ( -14.04637585414641165, -8.168855721704870732, 70.83619327840688129 ) ) ;
#38014 = CARTESIAN_POINT ( 'NONE',  ( -21.15569899156770717, -20.79502053738513112, 72.82446725055457648 ) ) ;
#38015 = VERTEX_POINT ( 'NONE', #26893 ) ;
#38016 = ORIENTED_EDGE ( 'NONE', *, *, #7106, .T. ) ;
#38017 = CARTESIAN_POINT ( 'NONE',  ( -14.79284385650551670, -7.406986770994973490, 48.81910596585309747 ) ) ;
#38018 = EDGE_CURVE ( 'NONE', #7220, #28, #28142, .T. ) ;
#38019 = CARTESIAN_POINT ( 'NONE',  ( -13.87677485259778543, -8.712488334168142501, 74.40774694939290157 ) ) ;
#38020 = ADVANCED_FACE ( 'NONE', ( #44881 ), #18752, .T. ) ;
#38021 = CARTESIAN_POINT ( 'NONE',  ( -43.14308517176575464, -25.10920654474410441, 57.24806946917839667 ) ) ;
#38022 = CARTESIAN_POINT ( 'NONE',  ( -14.06159385650551741, -9.295667164867525756, 49.30633214617472504 ) ) ;
#38023 = B_SPLINE_CURVE_WITH_KNOTS ( 'NONE', 3,
 ( #4072, #34079, #18828, #11937, #8017, #34315, #33835, #11684, #23029, #15115 ),
 .UNSPECIFIED., .F., .F.,
 ( 4, 2, 2, 2, 4 ),
 ( 0.000000000000000000, 0.2500000000000000000, 0.5000000000000000000, 0.7500000000000000000, 1.000000000000000000 ),
 .UNSPECIFIED. ) ;
#38024 = FACE_OUTER_BOUND ( 'NONE', #34913, .T. ) ;
#38025 = FACE_OUTER_BOUND ( 'NONE', #19400, .T. ) ;
#38026 = CARTESIAN_POINT ( 'NONE',  ( -22.33376602745314798, -19.86903051493498040, 69.18890041286789483 ) ) ;
#38027 = DIRECTION ( 'NONE',  ( 6.885933443815673122E-06, -1.077603661396111343E-05, 0.9999999999182304089 ) ) ;
#38028 = ORIENTED_EDGE ( 'NONE', *, *, #14129, .T. ) ;
#38029 = FACE_OUTER_BOUND ( 'NONE', #5713, .T. ) ;
#38030 = EDGE_CURVE ( 'NONE', #7125, #6672, #26398, .T. ) ;
#38031 = EDGE_LOOP ( 'NONE', ( #33123, #41184, #5409, #17203 ) ) ;
#38032 = CARTESIAN_POINT ( 'NONE',  ( -22.24723880939002996, -9.656319818818069223, 59.86604062818025795 ) ) ;
#38033 = CARTESIAN_POINT ( 'NONE',  ( -9.974130135034549482, -14.85786239279031840, 74.97591673537033330 ) ) ;
#38034 = EDGE_CURVE ( 'NONE', #18836, #32319, #31725, .T. ) ;
#38036 = EDGE_CURVE ( 'NONE', #37009, #45418, #19978, .T. ) ;
#38035 = CARTESIAN_POINT ( 'NONE',  ( -23.74619254753875808, -11.68933987248222550, 63.10218278636759237 ) ) ;
#38037 = CARTESIAN_POINT ( 'NONE',  ( -12.06140467229625912, -20.05244645202335008, 54.27966884056654351 ) ) ;
#38038 = EDGE_CURVE ( 'NONE', #33140, #4721, #29881, .T. ) ;
#38039 = VERTEX_POINT ( 'NONE', #42145 ) ;
#38040 = CARTESIAN_POINT ( 'NONE',  ( -17.91451304303208403, -22.24313331792350112, 61.99040607801043734 ) ) ;
#38041 = DIRECTION ( 'NONE',  ( 3.413470714839332458E-33, -1.190614954331866791E-16, 1.000000000000000000 ) ) ;
#38042 =( BOUNDED_CURVE ( )  B_SPLINE_CURVE ( 2, ( #22235, #6497, #14324, #37227, #40226, #32815, #47849, #33527, #14086 ),
 .UNSPECIFIED., .F., .F. ) 
 B_SPLINE_CURVE_WITH_KNOTS ( ( 3, 2, 2, 2, 3 ),
 ( 0.2083333333333331761, 0.2187499999999998890, 0.2291666666666666297, 0.2395833333333333703, 0.2500000000000001110 ),
 .UNSPECIFIED. ) 
 CURVE ( )  GEOMETRIC_REPRESENTATION_ITEM ( )  RATIONAL_B_SPLINE_CURVE ( ( 1.000000000000001110, 0.9238795325112855172, 1.000000000000000000, 0.9238795325112867385, 1.000000000000000000, 0.9238795325112867385, 1.000000000000000000, 0.9238795325112859613, 1.000000000000000888 ) ) 
 REPRESENTATION_ITEM ( '' )  );
#38043 = CARTESIAN_POINT ( 'NONE',  ( -17.03575403388767384, -5.365376231199011414, 53.49999999999995026 ) ) ;
#38044 = ORIENTED_EDGE ( 'NONE', *, *, #7217, .F. ) ;
#38045 = DIRECTION ( 'NONE',  ( -0.8967515337576290602, 0.4425343904188011046, -9.546469663397771497E-09 ) ) ;
#38046 = CARTESIAN_POINT ( 'NONE',  ( -17.42409385541299471, -14.80920654474435771, 49.52966884056655772 ) ) ;
#38047 = CARTESIAN_POINT ( 'NONE',  ( -16.26183769579148475, -7.855670737815882987, 60.50028478907629648 ) ) ;
#38048 = CARTESIAN_POINT ( 'NONE',  ( -13.38462656077074442, -20.58719956993326861, 58.19650077713541947 ) ) ;
#38049 = PRODUCT_CONTEXT ( 'NONE', #33787, 'mechanical' ) ;
#38050 = VERTEX_POINT ( 'NONE', #31296 ) ;
#38051 = B_SPLINE_CURVE_WITH_KNOTS ( 'NONE', 1,
 ( #43699, #28902 ),
 .UNSPECIFIED., .F., .F.,
 ( 2, 2 ),
 ( 0.000000000000000000, 1.000000000000000000 ),
 .UNSPECIFIED. ) ;
#38052 = DIRECTION ( 'NONE',  ( -3.071710424422018668E-17, 6.404604876783312462E-16, 1.000000000000000000 ) ) ;
#38053 = CARTESIAN_POINT ( 'NONE',  ( -50.42609385541305755, -14.80920654474419074, 65.94705882352940307 ) ) ;
#38054 = CARTESIAN_POINT ( 'NONE',  ( -14.81784385541216587, -6.860780111197240849, 51.02154966934948277 ) ) ;
#38055 = EDGE_LOOP ( 'NONE', ( #44425, #1127 ) ) ;
#38056 = FACE_OUTER_BOUND ( 'NONE', #3608, .T. ) ;
#38057 = ORIENTED_EDGE ( 'NONE', *, *, #17632, .T. ) ;
#38058 = CARTESIAN_POINT ( 'NONE',  ( -12.70343478140934224, -9.045698024298063800, 70.94901720388561728 ) ) ;
#38059 = CARTESIAN_POINT ( 'NONE',  ( -12.14425528403576848, -10.13739698163135117, 64.02914326607979945 ) ) ;
#38060 = ORIENTED_EDGE ( 'NONE', *, *, #28932, .F. ) ;
#38061 =( BOUNDED_SURFACE ( )  B_SPLINE_SURFACE ( 3, 1, ( 
 ( #9539, #36091 ),
 ( #21343, #17384 ),
 ( #31690, #39069 ),
 ( #36336, #24562 ),
 ( #13675, #9051 ),
 ( #5352, #2615 ),
 ( #43511, #43752 ) ),
 .UNSPECIFIED., .T., .F., .F. ) 
 B_SPLINE_SURFACE_WITH_KNOTS ( ( 4, 3, 4 ),
 ( 2, 2 ),
 ( 0.000000000000000000, 0.5000000000000000000, 1.000000000000000000 ),
 ( 0.000000000000000000, 1.000000000000000000 ),
 .UNSPECIFIED. ) 
 GEOMETRIC_REPRESENTATION_ITEM ( )  RATIONAL_B_SPLINE_SURFACE ( (
 ( 1.000000000000000000, 1.000000000000000000),
 ( 0.3333333333333335369, 0.3333333333333330373),
 ( 0.3333333333333335369, 0.3333333333333330373),
 ( 1.000000000000000000, 1.000000000000000000),
 ( 0.3333333333333333703, 0.3333333333333333703),
 ( 0.3333333333333333703, 0.3333333333333333703),
 ( 1.000000000000000000, 1.000000000000000000) ) ) 
 REPRESENTATION_ITEM ( '' )  SURFACE ( )  );
#38062 = CARTESIAN_POINT ( 'NONE',  ( -10.96962953718779232, -17.51874670794821043, 68.39721950254519811 ) ) ;
#38063 = ORIENTED_EDGE ( 'NONE', *, *, #17429, .F. ) ;
#38064 = ADVANCED_FACE ( 'NONE', ( #47044 ), #8904, .T. ) ;
#38065 = VERTEX_POINT ( 'NONE', #13050 ) ;
#38066 = VERTEX_POINT ( 'NONE', #38926 ) ;
#38067 = B_SPLINE_CURVE_WITH_KNOTS ( 'NONE', 3,
 ( #15662, #662, #42027, #30717, #34624, #45743, #15907, #1625, #34866, #30952 ),
 .UNSPECIFIED., .F., .F.,
 ( 4, 2, 2, 2, 4 ),
 ( 0.6272669072783326749, 0.7522669073002039575, 0.8772669073220753511, 1.002266907343946745, 1.127266907365817916 ),
 .UNSPECIFIED. ) ;
#38068 = CARTESIAN_POINT ( 'NONE',  ( -19.38354029837526937, -21.99704006310037130, 58.70224247979420085 ) ) ;
#38069 = DIRECTION ( 'NONE',  ( -0.7670373483544790094, -0.6416024518573233415, 2.496223344567222537E-08 ) ) ;
#38070 = CARTESIAN_POINT ( 'NONE',  ( -24.16171830865566861, -12.91022455891425125, 66.30246698681006023 ) ) ;
#38071 = DIRECTION ( 'NONE',  ( 0.9687793358424822143, -0.2479245821708672415, 0.000000000000000000 ) ) ;
#38072 = CARTESIAN_POINT ( 'NONE',  ( -19.88034385541303450, -9.360768649639323868, 51.01397948905923130 ) ) ;
#38073 =( BOUNDED_CURVE ( )  B_SPLINE_CURVE ( 3, ( #45639, #4992, #38206, #20003 ),
 .UNSPECIFIED., .F., .F. ) 
 B_SPLINE_CURVE_WITH_KNOTS ( ( 4, 4 ),
 ( 0.4074455897393702841, 0.5000000000000000000 ),
 .UNSPECIFIED. ) 
 CURVE ( )  GEOMETRIC_REPRESENTATION_ITEM ( )  RATIONAL_B_SPLINE_CURVE ( ( 0.6983129098261073864, 0.7760317562607140784, 0.8765941196520128376, 1.000000000000005773 ) ) 
 REPRESENTATION_ITEM ( '' )  );
#38074 = ORIENTED_EDGE ( 'NONE', *, *, #32489, .T. ) ;
#38075 = ORIENTED_EDGE ( 'NONE', *, *, #41984, .T. ) ;
#38076 = AXIS2_PLACEMENT_3D ( 'NONE', #29111, #18254, #6950 ) ;
#38077 = B_SPLINE_CURVE_WITH_KNOTS ( 'NONE', 3,
 ( #5347, #31923, #23824, #34645, #1644, #42537, #27742, #16405, #4869, #16883 ),
 .UNSPECIFIED., .F., .F.,
 ( 4, 2, 2, 2, 4 ),
 ( 0.000000000000000000, 0.2500000000000000000, 0.5000000000000000000, 0.7500000000000000000, 1.000000000000000000 ),
 .UNSPECIFIED. ) ;
#38078 = CARTESIAN_POINT ( 'NONE',  ( -17.79901357976508791, -7.766176623049141803, 63.96545652844361740 ) ) ;
#38079 = CIRCLE ( 'NONE', #47547, 5.249999999999998224 ) ;
#38080 = EDGE_CURVE ( 'NONE', #6697, #24590, #15835, .T. ) ;
#38081 = FACE_OUTER_BOUND ( 'NONE', #24946, .T. ) ;
#38082 = CARTESIAN_POINT ( 'NONE',  ( -20.27409385541325904, -6.859212275519745106, 50.50378509014061734 ) ) ;
#38083 = CARTESIAN_POINT ( 'NONE',  ( -23.16275847746607752, -18.91806288495012112, 69.43805163930900903 ) ) ;
#38084 = ORIENTED_EDGE ( 'NONE', *, *, #29266, .T. ) ;
#38085 = CARTESIAN_POINT ( 'NONE',  ( -14.59284385650551563, -7.406986770994973490, 48.81910596585309747 ) ) ;
#38086 = ORIENTED_EDGE ( 'NONE', *, *, #31717, .F. ) ;
#38087 = CARTESIAN_POINT ( 'NONE',  ( -17.06879511326789256, -7.767867012253359071, 73.97490359703523666 ) ) ;
#38088 = CARTESIAN_POINT ( 'NONE',  ( -12.05727448861903639, -19.97649948735875114, 61.65324539733175868 ) ) ;
#38089 = DIRECTION ( 'NONE',  ( -0.5652317888644006194, -0.8249321334856242194, 7.911723905267717726E-08 ) ) ;
#38090 = ORIENTED_EDGE ( 'NONE', *, *, #1294, .F. ) ;
#38091 = FACE_OUTER_BOUND ( 'NONE', #41201, .T. ) ;
#38092 = DIRECTION ( 'NONE',  ( -3.071710424422018668E-17, 6.404604876783312462E-16, 1.000000000000000000 ) ) ;
#38093 = ADVANCED_FACE ( 'NONE', ( #35697 ), #16253, .T. ) ;
#38094 = EDGE_CURVE ( 'NONE', #35350, #20172, #34897, .T. ) ;
#38095 = CARTESIAN_POINT ( 'NONE',  ( -22.78151503426583702, -19.98625364524674097, 72.75905110386234753 ) ) ;
#38096 = ORIENTED_EDGE ( 'NONE', *, *, #23137, .F. ) ;
#38097 = DIRECTION ( 'NONE',  ( 1.000000000000000000, 2.866981220435666553E-17, 0.000000000000000000 ) ) ;
#38098 = CYLINDRICAL_SURFACE ( 'NONE', #28357, 0.1499999999999988287 ) ;
#38099 = CARTESIAN_POINT ( 'NONE',  ( -20.16899036125798972, -7.883296231106626806, 73.82122343779342089 ) ) ;
#38100 = ORIENTED_EDGE ( 'NONE', *, *, #40762, .T. ) ;
#38101 = LINE ( 'NONE', #3911, #3155 ) ;
#38102 = VERTEX_POINT ( 'NONE', #1498 ) ;
#38103 = CIRCLE ( 'NONE', #19250, 1.999999999999999112 ) ;
#38104 = CARTESIAN_POINT ( 'NONE',  ( -10.18364478422453345, -13.05433800282328960, 71.46474530336836040 ) ) ;
#38105 = EDGE_CURVE ( 'NONE', #31313, #19293, #6293, .T. ) ;
#38106 = ADVANCED_FACE ( 'NONE', ( #20470 ), #35465, .T. ) ;
#38107 = CARTESIAN_POINT ( 'NONE',  ( -24.35389707626741185, -16.10709931453381216, 62.87856533165624029 ) ) ;
#38108 = ORIENTED_EDGE ( 'NONE', *, *, #25832, .F. ) ;
#38109 = CARTESIAN_POINT ( 'NONE',  ( -24.26384900572966075, -13.06773595597165460, 69.91676003018049812 ) ) ;
#38110 = VECTOR ( 'NONE', #39318, 1000.000000000000000 ) ;
#38111 = EDGE_CURVE ( 'NONE', #7006, #16121, #46806, .T. ) ;
#38112 = DIRECTION ( 'NONE',  ( 0.5540494244615011832, -0.8324837747691418155, 2.496966302803637394E-17 ) ) ;
#38113 = ORIENTED_EDGE ( 'NONE', *, *, #11237, .F. ) ;
#38114 = CARTESIAN_POINT ( 'NONE',  ( -22.13027617770598354, -9.033668753454486833, 63.35300274347135741 ) ) ;
#38115 = UNCERTAINTY_MEASURE_WITH_UNIT (LENGTH_MEASURE( 1.000000000000000082E-05 ), #5152, 'distance_accuracy_value', 'NONE');
#38116 = CARTESIAN_POINT ( 'NONE',  ( -15.92409385541305333, -15.80920654474410725, 52.21286476528345588 ) ) ;
#38117 = CARTESIAN_POINT ( 'NONE',  ( -11.46207494020916862, -11.14107511578148113, 57.49437795721348010 ) ) ;
#38118 = EDGE_LOOP ( 'NONE', ( #22976, #15934 ) ) ;
#38119 = CARTESIAN_POINT ( 'NONE',  ( -43.51983853626412468, -13.51240245935757578, 70.50000000000000000 ) ) ;
#38120 = EDGE_CURVE ( 'NONE', #40496, #28056, #3852, .T. ) ;
#38121 = EDGE_LOOP ( 'NONE', ( #23549, #35213, #23426, #4663, #42687, #40423, #47719, #35698, #6259, #13947, #37587, #23043, #14117, #18119 ) ) ;
#38122 = ORIENTED_EDGE ( 'NONE', *, *, #17901, .F. ) ;
#38123 = CARTESIAN_POINT ( 'NONE',  ( -27.42409385541305511, -25.10920654474410441, 81.99999999999998579 ) ) ;
#38124 = CARTESIAN_POINT ( 'NONE',  ( -10.64242474325409304, -12.85371797616438272, 71.35261706278205907 ) ) ;
#38125 = B_SPLINE_CURVE_WITH_KNOTS ( 'NONE', 3,
 ( #14879, #21581, #21812, #26238, #3579, #33858, #6794, #13912, #44475, #3090 ),
 .UNSPECIFIED., .F., .F.,
 ( 4, 2, 2, 2, 4 ),
 ( 0.1272669073658506955, 0.2522669073463346678, 0.3772669073268186679, 0.5022669073073026125, 0.6272669072877865570 ),
 .UNSPECIFIED. ) ;
#38126 = PLANE ( 'NONE',  #28051 ) ;
#38127 = CARTESIAN_POINT ( 'NONE',  ( -22.74909385650551386, -8.104110260919577868, 48.81699501597546487 ) ) ;
#38128 = CARTESIAN_POINT ( 'NONE',  ( -12.43268922994311509, -19.71711825911901528, 61.69678636630293056 ) ) ;
#38129 = CARTESIAN_POINT ( 'NONE',  ( -12.69763806180496601, -20.04058448603118592, 68.62185382311069759 ) ) ;
#38130 = CARTESIAN_POINT ( 'NONE',  ( -14.23034385759798859, -6.857644439848010975, 49.98602051094140108 ) ) ;
#38131 = CARTESIAN_POINT ( 'NONE',  ( -12.14425506381237163, -10.13739722748950634, 64.32914326607961186 ) ) ;
#38132 = ORIENTED_EDGE ( 'NONE', *, *, #12287, .F. ) ;
#38133 = DIRECTION ( 'NONE',  ( -9.593247862760507776E-06, -5.650837228699102996E-06, 0.9999999999380188020 ) ) ;
#38134 = B_SPLINE_CURVE_WITH_KNOTS ( 'NONE', 3,
 ( #24515, #36517, #20802, #17333, #1845, #13633, #35802, #9241, #2079, #17080 ),
 .UNSPECIFIED., .F., .F.,
 ( 4, 2, 2, 2, 4 ),
 ( 0.000000000000000000, 0.2500000000000000000, 0.5000000000000000000, 0.7500000000000000000, 1.000000000000000000 ),
 .UNSPECIFIED. ) ;
#38135 = CARTESIAN_POINT ( 'NONE',  ( -10.02898863523709316, -13.90543673706342886, 57.62541899832793035 ) ) ;
#38136 = CARTESIAN_POINT ( 'NONE',  ( -21.90037927395905371, -9.427412627673714240, 59.73673662101968063 ) ) ;
#38137 = ORIENTED_EDGE ( 'NONE', *, *, #27492, .F. ) ;
#38138 = AXIS2_PLACEMENT_3D ( 'NONE', #25783, #26518, #3127 ) ;
#38139 = ORIENTED_EDGE ( 'NONE', *, *, #17372, .F. ) ;
#38140 = DIRECTION ( 'NONE',  ( 2.866981220435666553E-17, -1.000000000000000000, -1.190614954331866791E-16 ) ) ;
#38141 = VECTOR ( 'NONE', #46194, 1000.000000000000000 ) ;
#38142 = CARTESIAN_POINT ( 'NONE',  ( -24.86610161942810038, -14.46236550061385984, 66.29797407254456232 ) ) ;
#38143 = CARTESIAN_POINT ( 'NONE',  ( -15.71124685674608124, -7.966721484443281653, 74.17165852965567296 ) ) ;
#38144 = CARTESIAN_POINT ( 'NONE',  ( -22.04114742393716142, -9.481025248639417313, 59.73643293354757589 ) ) ;
#38145 = EDGE_CURVE ( 'NONE', #383, #27062, #44037, .T. ) ;
#38146 = ORIENTED_EDGE ( 'NONE', *, *, #36525, .F. ) ;
#38147 = DIRECTION ( 'NONE',  ( -5.466375705775733989E-17, 0.000000000000000000, -1.000000000000000000 ) ) ;
#38148 = CARTESIAN_POINT ( 'NONE',  ( -22.96481576609224717, -19.16891988936071556, 58.89882756593014790 ) ) ;
#38149 = EDGE_CURVE ( 'NONE', #46061, #4040, #25127, .T. ) ;
#38150 = ORIENTED_EDGE ( 'NONE', *, *, #37338, .T. ) ;
#38151 = PLANE ( 'NONE',  #21795 ) ;
#38152 = CARTESIAN_POINT ( 'NONE',  ( -17.42409385541299471, -14.80920654474434883, 62.02966884056656482 ) ) ;
#38153 = VERTEX_POINT ( 'NONE', #10104 ) ;
#38154 = CARTESIAN_POINT ( 'NONE',  ( -12.55411140858086760, -19.90724249994213935, 65.15202838036978505 ) ) ;
#38155 = ORIENTED_EDGE ( 'NONE', *, *, #28577, .T. ) ;
#38156 = B_SPLINE_CURVE_WITH_KNOTS ( 'NONE', 3,
 ( #38992, #20288, #35293, #47371, #25433, #6242, #28881, #24482, #40444, #39970 ),
 .UNSPECIFIED., .F., .F.,
 ( 4, 2, 2, 2, 4 ),
 ( 0.000000000000000000, 0.2500000000000000000, 0.5000000000000000000, 0.7500000000000000000, 1.000000000000000000 ),
 .UNSPECIFIED. ) ;
#38157 = ADVANCED_FACE ( 'NONE', ( #2936 ), #24653, .T. ) ;
#38158 = CARTESIAN_POINT ( 'NONE',  ( -16.98659385759799179, -7.222650657624104298, 49.61879703869476543 ) ) ;
#38159 = VERTEX_POINT ( 'NONE', #14247 ) ;
#38160 = CARTESIAN_POINT ( 'NONE',  ( -13.77528250856571645, -8.773395728905704516, 57.38456636527085664 ) ) ;
#38161 = ADVANCED_FACE ( 'NONE', ( #3187 ), #15469, .T. ) ;
#38162 = CARTESIAN_POINT ( 'NONE',  ( -16.70534385650551812, -8.801233750844183135, 48.81488406609782515 ) ) ;
#38163 = CARTESIAN_POINT ( 'NONE',  ( -17.72419709140651278, -21.80277058947482516, 58.70553378253836030 ) ) ;
#38164 = EDGE_CURVE ( 'NONE', #18836, #32319, #4084, .T. ) ;
#38165 = DIRECTION ( 'NONE',  ( 3.071710424422018668E-17, -6.404604876783312462E-16, -1.000000000000000000 ) ) ;
#38166 = CARTESIAN_POINT ( 'NONE',  ( -22.23733827145997566, -19.96043728507621040, 65.70421731380814379 ) ) ;
#38167 = EDGE_LOOP ( 'NONE', ( #776, #16319 ) ) ;
#38168 = CARTESIAN_POINT ( 'NONE',  ( -14.98249323814573941, -9.880861343182303358, 53.49999999999995026 ) ) ;
#38169 = DIRECTION ( 'NONE',  ( 0.9687793358424821033, -0.2479245821708679909, 0.000000000000000000 ) ) ;
#38170 = DIRECTION ( 'NONE',  ( 0.000000000000000000, 0.000000000000000000, 1.000000000000000000 ) ) ;
#38171 = CARTESIAN_POINT ( 'NONE',  ( -48.42409385541304800, -25.10920654474410441, 47.99999999999998579 ) ) ;
#38172 = CARTESIAN_POINT ( 'NONE',  ( -22.84361065395838608, -9.697247154002193170, 73.58886925941359891 ) ) ;
#38173 = EDGE_LOOP ( 'NONE', ( #24181, #5111, #30317, #5777, #19455 ) ) ;
#38174 = ORIENTED_EDGE ( 'NONE', *, *, #865, .F. ) ;
#38175 = LINE ( 'NONE', #4961, #36137 ) ;
#38176 = DIRECTION ( 'NONE',  ( -0.7111926860893348357, 0.6953514824629878355, 0.1033986416233889510 ) ) ;
#38177 = VERTEX_POINT ( 'NONE', #36423 ) ;
#38178 = CARTESIAN_POINT ( 'NONE',  ( -24.10561640116403481, -17.05872324192169032, 73.18336028593354570 ) ) ;
#38179 = CARTESIAN_POINT ( 'NONE',  ( -15.80117947156642622, -7.538110422750471606, 67.24033040303804398 ) ) ;
#38180 = CARTESIAN_POINT ( 'NONE',  ( -21.37409385759799108, -6.859212275519751323, 50.50378509014259265 ) ) ;
#38181 = CARTESIAN_POINT ( 'NONE',  ( -20.15615321779684521, -7.878236066423426109, 73.87096600761617538 ) ) ;
#38182 =( BOUNDED_CURVE ( )  B_SPLINE_CURVE ( 3, ( #7207, #29595, #44625, #10883 ),
 .UNSPECIFIED., .F., .F. ) 
 B_SPLINE_CURVE_WITH_KNOTS ( ( 4, 4 ),
 ( 0.5000000000000000000, 0.9074455897393655102 ),
 .UNSPECIFIED. ) 
 CURVE ( )  GEOMETRIC_REPRESENTATION_ITEM ( )  RATIONAL_B_SPLINE_CURVE ( ( 0.9999999999999850120, 0.4567392136813225867, 0.3561768502900372058, 0.6983129098261126044 ) ) 
 REPRESENTATION_ITEM ( '' )  );
#38183 = CARTESIAN_POINT ( 'NONE',  ( -12.05084272712144511, -19.96988037603709643, 61.51961716641547184 ) ) ;
#38184 = DIRECTION ( 'NONE',  ( 2.866981220435666553E-17, -1.000000000000000000, -1.190614954331866791E-16 ) ) ;
#38185 = DIRECTION ( 'NONE',  ( 0.000000000000000000, 0.000000000000000000, 1.000000000000000000 ) ) ;
#38186 = ORIENTED_EDGE ( 'NONE', *, *, #18400, .F. ) ;
#38187 = LINE ( 'NONE', #30106, #34376 ) ;
#38188 = CARTESIAN_POINT ( 'NONE',  ( 10.57590614458695377, 3.114729847419844599, 50.78398819077492732 ) ) ;
#38189 = CARTESIAN_POINT ( 'NONE',  ( -19.80301260837064703, -21.44571507605098404, 69.23482476707422961 ) ) ;
#38190 = CARTESIAN_POINT ( 'NONE',  ( -17.42409385541299471, -14.80920654474435771, 49.52966884056655772 ) ) ;
#38191 = CARTESIAN_POINT ( 'NONE',  ( -21.59804182614902146, -20.98026282434625500, 72.70941811628220819 ) ) ;
#38192 =( BOUNDED_SURFACE ( )  B_SPLINE_SURFACE ( 3, 1, ( 
 ( #10570, #7374 ),
 ( #21649, #36405 ),
 ( #25580, #10083 ),
 ( #47992, #44547 ),
 ( #3415, #40587 ),
 ( #33193, #18420 ),
 ( #40843, #6872 ) ),
 .UNSPECIFIED., .T., .F., .F. ) 
 B_SPLINE_SURFACE_WITH_KNOTS ( ( 4, 3, 4 ),
 ( 2, 2 ),
 ( 0.000000000000000000, 0.5000000000000000000, 1.000000000000000000 ),
 ( 0.000000000000000000, 1.000000000000000000 ),
 .UNSPECIFIED. ) 
 GEOMETRIC_REPRESENTATION_ITEM ( )  RATIONAL_B_SPLINE_SURFACE ( (
 ( 1.000000000000000000, 1.000000000000000000),
 ( 0.3333333333333335369, 0.3333333333333330373),
 ( 0.3333333333333335369, 0.3333333333333330373),
 ( 1.000000000000000000, 1.000000000000000000),
 ( 0.3333333333333333703, 0.3333333333333333703),
 ( 0.3333333333333333703, 0.3333333333333333703),
 ( 1.000000000000000000, 1.000000000000000000) ) ) 
 REPRESENTATION_ITEM ( '' )  SURFACE ( )  );
#38193 = DIRECTION ( 'NONE',  ( 3.549360974551883545E-17, -6.371834667872732552E-18, -1.000000000000000000 ) ) ;
#38194 = EDGE_LOOP ( 'NONE', ( #41651, #18908, #1799, #44971, #1129 ) ) ;
#38195 = ORIENTED_EDGE ( 'NONE', *, *, #42754, .F. ) ;
#38196 = EDGE_LOOP ( 'NONE', ( #11399, #20279, #4398, #2569, #36005 ) ) ;
#38197 = CARTESIAN_POINT ( 'NONE',  ( -11.64547064851736202, -18.85300969848255193, 64.63218190802510321 ) ) ;
#38198 = CARTESIAN_POINT ( 'NONE',  ( -18.85724798917316392, -7.906108138700305155, 67.18599644112759961 ) ) ;
#38199 = EDGE_CURVE ( 'NONE', #32734, #40286, #45967, .T. ) ;
#38200 =( BOUNDED_CURVE ( )  B_SPLINE_CURVE ( 2, ( #21284, #36996, #36281, #36739, #21527, #44195, #32822, #10443, #14565 ),
 .UNSPECIFIED., .F., .F. ) 
 B_SPLINE_CURVE_WITH_KNOTS ( ( 3, 2, 2, 2, 3 ),
 ( 0.02360435172767372594, 0.02458795513743799663, 0.02557155854720226038, 0.02655516195696652759, 0.02753876536673079828 ),
 .UNSPECIFIED. ) 
 CURVE ( )  GEOMETRIC_REPRESENTATION_ITEM ( )  RATIONAL_B_SPLINE_CURVE ( ( 0.9999999999999431566, 0.9238795325113435819, 1.000000000000000000, 0.9238795325112867385, 1.000000000000000000, 0.9238795325112867385, 1.000000000000000000, 0.9238795325108709600, 1.000000000000415890 ) ) 
 REPRESENTATION_ITEM ( '' )  );
#38201 = CARTESIAN_POINT ( 'NONE',  ( -10.80691635537187878, -11.38640170085024828, 67.81853383790260636 ) ) ;
#38202 = AXIS2_PLACEMENT_3D ( 'NONE', #1443, #28288, #16699 ) ;
#38203 = CARTESIAN_POINT ( 'NONE',  ( -13.62591164035943692, -20.69067956303819145, 65.05799250888908603 ) ) ;
#38204 = CARTESIAN_POINT ( 'NONE',  ( -17.70613249112851761, -7.363797380145674865, 60.19405475747598899 ) ) ;
#38205 = VERTEX_POINT ( 'NONE', #43366 ) ;
#38206 = CARTESIAN_POINT ( 'NONE',  ( -18.07335586441531916, -21.82939548422117682, 65.35091948115599791 ) ) ;
#38207 = B_SPLINE_CURVE_WITH_KNOTS ( 'NONE', 3,
 ( #21142, #1700, #2423, #13004, #17434, #47717, #32465, #9096, #47490, #24357 ),
 .UNSPECIFIED., .F., .F.,
 ( 4, 2, 2, 2, 4 ),
 ( 0.000000000000000000, 0.2500000000000000000, 0.5000000000000000000, 0.7500000000000000000, 1.000000000000000000 ),
 .UNSPECIFIED. ) ;
#38208 = DIRECTION ( 'NONE',  ( 0.000000000000000000, 0.000000000000000000, -1.000000000000000000 ) ) ;
#38209 = VERTEX_POINT ( 'NONE', #43607 ) ;
#38210 = CARTESIAN_POINT ( 'NONE',  ( -19.74200936563730124, -21.46758226568296024, 68.94954551542706156 ) ) ;
#38211 = FACE_OUTER_BOUND ( 'NONE', #1726, .T. ) ;
#38212 = ORIENTED_EDGE ( 'NONE', *, *, #39825, .F. ) ;
#38213 = FACE_OUTER_BOUND ( 'NONE', #21697, .T. ) ;
#38214 = CARTESIAN_POINT ( 'NONE',  ( -12.86353962931362283, -9.432586330540292607, 74.33395128836551180 ) ) ;
#38215 = CARTESIAN_POINT ( 'NONE',  ( -17.77594298899184366, -7.367433885636743618, 60.26556189360973548 ) ) ;
#38216 = ORIENTED_EDGE ( 'NONE', *, *, #29302, .T. ) ;
#38217 = CARTESIAN_POINT ( 'NONE',  ( -11.49688049385020960, -18.62690763749001732, 64.76179218520603342 ) ) ;
#38218 = EDGE_CURVE ( 'NONE', #21369, #15882, #29363, .T. ) ;
#38219 = DIRECTION ( 'NONE',  ( 0.000000000000000000, 9.912705577010318647E-16, 1.000000000000000000 ) ) ;
#38220 = EDGE_CURVE ( 'NONE', #27631, #2446, #1717, .T. ) ;
#38221 = CARTESIAN_POINT ( 'NONE',  ( -16.22585665461787841, -7.910893037574660447, 63.78084232168319545 ) ) ;
#38222 = CARTESIAN_POINT ( 'NONE',  ( -20.35492123770571382, -11.13690394275196383, 52.02966884056656482 ) ) ;
#38223 = CARTESIAN_POINT ( 'NONE',  ( -12.18836193727821460, -19.53083876418623532, 57.94154444592973618 ) ) ;
#38224 = DIRECTION ( 'NONE',  ( 1.000000000000000000, 1.669677910507523057E-21, 6.493791346278465266E-22 ) ) ;
#38225 = CARTESIAN_POINT ( 'NONE',  ( -15.56465948913149333, -7.543361525925791788, 53.27966884056655061 ) ) ;
#38226 = CARTESIAN_POINT ( 'NONE',  ( -18.67235195658554403, -19.33882101600501713, 52.02966884056656482 ) ) ;
#38227 = EDGE_CURVE ( 'NONE', #43698, #2810, #31024, .T. ) ;
#38228 = CARTESIAN_POINT ( 'NONE',  ( -22.68646401470678953, -20.08284273627726435, 69.35913316877790180 ) ) ;
#38229 = CARTESIAN_POINT ( 'NONE',  ( -21.51159385650551670, -6.922745924619793101, 51.69366785382590024 ) ) ;
#38230 = ORIENTED_EDGE ( 'NONE', *, *, #6756, .F. ) ;
#38231 = LINE ( 'NONE', #19296, #9275 ) ;
#38232 = ORIENTED_EDGE ( 'NONE', *, *, #46983, .T. ) ;
#38233 = CARTESIAN_POINT ( 'NONE',  ( -24.38441325179858410, -15.93105629309529370, 66.35765103335467074 ) ) ;
#38234 = CARTESIAN_POINT ( 'NONE',  ( -23.22802958525249295, -10.13834356547682702, 63.27174767778126352 ) ) ;
#38235 = DIRECTION ( 'NONE',  ( 1.000000000000000000, 2.866981220435666553E-17, 0.000000000000000000 ) ) ;
#38236 = ADVANCED_FACE ( 'NONE', ( #30045 ), #45716, .T. ) ;
#38237 = ORIENTED_EDGE ( 'NONE', *, *, #15928, .F. ) ;
#38238 = EDGE_CURVE ( 'NONE', #31794, #31985, #4680, .T. ) ;
#38239 = CARTESIAN_POINT ( 'NONE',  ( -23.62594491300536959, -11.45603751788689451, 66.70742424642772050 ) ) ;
#38240 = AXIS2_PLACEMENT_3D ( 'NONE', #30792, #15240, #8139 ) ;
#38241 = CARTESIAN_POINT ( 'NONE',  ( -10.05862335131466700, -15.92885902279982524, 64.69266873560974318 ) ) ;
#38242 = VECTOR ( 'NONE', #12835, 1000.000000000000000 ) ;
#38243 = CARTESIAN_POINT ( 'NONE',  ( -10.09423541311275763, -16.14245677117450839, 68.15484689107481131 ) ) ;
#38244 = ORIENTED_EDGE ( 'NONE', *, *, #30060, .F. ) ;
#38245 = CYLINDRICAL_SURFACE ( 'NONE', #7009, 4.686499999999997002 ) ;
#38246 = CARTESIAN_POINT ( 'NONE',  ( -23.74454562765497556, -11.67923450027144305, 59.36747125042367657 ) ) ;
#38247 = CARTESIAN_POINT ( 'NONE',  ( -24.54490520938829334, -12.61907488956320833, 69.97231776601158515 ) ) ;
#38248 = CARTESIAN_POINT ( 'NONE',  ( -10.46153521202717229, -17.45973047739676076, 64.77739380354385901 ) ) ;
#38249 = LINE ( 'NONE', #26462, #24425 ) ;
#38250 = EDGE_LOOP ( 'NONE', ( #32700, #18880, #3363, #7844, #40071, #36299, #33108, #18369, #17306, #9544, #8091, #43852 ) ) ;
#38251 = ORIENTED_EDGE ( 'NONE', *, *, #5460, .T. ) ;
#38252 = CARTESIAN_POINT ( 'NONE',  ( -22.35534385541304658, -8.623186033802570094, 49.24843789510466507 ) ) ;
#38253 = DIRECTION ( 'NONE',  ( 1.000000000000000000, 2.866981220435666553E-17, 0.000000000000000000 ) ) ;
#38254 = DIRECTION ( 'NONE',  ( -0.8459089628457129306, -0.5333273165489313961, 7.771812504399799980E-08 ) ) ;
#38255 = ADVANCED_FACE ( 'NONE', ( #18943 ), #30532, .T. ) ;
#38256 = CARTESIAN_POINT ( 'NONE',  ( -20.94324281608204430, -8.242681057013424351, 60.09771182510558418 ) ) ;
#38257 = CARTESIAN_POINT ( 'NONE',  ( -10.38360249164154325, -14.43747963625415487, 67.87272197508832505 ) ) ;
#38258 = CARTESIAN_POINT ( 'NONE',  ( -24.41089624436030547, -15.77327213725850719, 65.94836039739031719 ) ) ;
#38259 = ORIENTED_EDGE ( 'NONE', *, *, #40037, .T. ) ;
#38260 = CARTESIAN_POINT ( 'NONE',  ( -21.95523233784883033, -8.895446131873137929, 66.77654700642760588 ) ) ;
#38261 = EDGE_CURVE ( 'NONE', #11018, #26541, #45551, .T. ) ;
#38262 = CIRCLE ( 'NONE', #44581, 1.249999999999999334 ) ;
#38263 = CIRCLE ( 'NONE', #16266, 4.686499999999998778 ) ;
#38264 = ORIENTED_EDGE ( 'NONE', *, *, #21291, .T. ) ;
#38265 = CARTESIAN_POINT ( 'NONE',  ( -19.78614083979442029, -21.39864764726399216, 69.23482476778590922 ) ) ;
#38266 = CARTESIAN_POINT ( 'NONE',  ( -20.21548144266859737, -8.389848675143694479, 66.88990156496440420 ) ) ;
#38267 = DIRECTION ( 'NONE',  ( 6.865757730863489906E-07, 1.412849154798944614E-06, 0.9999999999987662092 ) ) ;
#38268 = CARTESIAN_POINT ( 'NONE',  ( -10.40245588357037043, -14.17414831712846990, 61.20349182037644198 ) ) ;
#38269 = ORIENTED_EDGE ( 'NONE', *, *, #45619, .T. ) ;
#38270 = CARTESIAN_POINT ( 'NONE',  ( -10.37818569806566948, -17.22973468411262132, 61.27247807055057649 ) ) ;
#38271 =( BOUNDED_CURVE ( )  B_SPLINE_CURVE ( 3, ( #11589, #37928, #26869, #45825 ),
 .UNSPECIFIED., .F., .F. ) 
 B_SPLINE_CURVE_WITH_KNOTS ( ( 4, 4 ),
 ( 0.5000000000000000000, 0.9074455897393649551 ),
 .UNSPECIFIED. ) 
 CURVE ( )  GEOMETRIC_REPRESENTATION_ITEM ( )  RATIONAL_B_SPLINE_CURVE ( ( 1.000000000000047296, 0.4567392136813318571, 0.3561768502899970157, 0.6983129098260942857 ) ) 
 REPRESENTATION_ITEM ( '' )  );
#38272 = VECTOR ( 'NONE', #34186, 1000.000000000000000 ) ;
#38273 = CARTESIAN_POINT ( 'NONE',  ( -20.13456941707305248, -8.355134980150365820, 70.55100345209505974 ) ) ;
#38274 = CARTESIAN_POINT ( 'NONE',  ( -19.52026799707963178, -8.074260338512710078, 60.05273170036824126 ) ) ;
#38275 = EDGE_LOOP ( 'NONE', ( #21892, #34058, #19834, #24600, #46027 ) ) ;
#38276 = PLANE ( 'NONE',  #34651 ) ;
#38277 = CARTESIAN_POINT ( 'NONE',  ( -20.86194851583517362, -21.41857929898468171, 58.74451539084461871 ) ) ;
#38278 = CARTESIAN_POINT ( 'NONE',  ( -10.89280197141400919, -11.22507430941316642, 64.33377434530349603 ) ) ;
#38279 = CARTESIAN_POINT ( 'NONE',  ( -21.12516169987187098, -20.80993955427394582, 69.06922321213187388 ) ) ;
#38280 = SHAPE_DEFINITION_REPRESENTATION ( #40922, #22625 ) ;
#38281 = B_SPLINE_CURVE_WITH_KNOTS ( 'NONE', 1,
 ( #40252, #2575 ),
 .UNSPECIFIED., .F., .F.,
 ( 2, 2 ),
 ( 0.000000000000000000, 1.000000000000000000 ),
 .UNSPECIFIED. ) ;
#38282 = EDGE_CURVE ( 'NONE', #11545, #34062, #15760, .T. ) ;
#38283 = CARTESIAN_POINT ( 'NONE',  ( -11.32469144785209103, -18.34471071427194744, 57.80714594245691984 ) ) ;
#38284 = CARTESIAN_POINT ( 'NONE',  ( -10.56627932147773308, -16.21290872759732693, 71.74750383609593030 ) ) ;
#38285 = CARTESIAN_POINT ( 'NONE',  ( -24.47371109942907808, -14.90716652360855576, 59.25772288469824645 ) ) ;
#38286 = EDGE_CURVE ( 'NONE', #27510, #42061, #10470, .T. ) ;
#38287 = CARTESIAN_POINT ( 'NONE',  ( -17.59331746709300148, -7.761237804004919916, 63.70057029381062819 ) ) ;
#38288 = EDGE_LOOP ( 'NONE', ( #38598, #44215, #17381, #33516 ) ) ;
#38289 = CARTESIAN_POINT ( 'NONE',  ( -12.14070233592774706, -10.21533170167876392, 67.57067125136083519 ) ) ;
#38290 = EDGE_CURVE ( 'NONE', #33105, #5915, #48240, .T. ) ;
#38291 = ORIENTED_EDGE ( 'NONE', *, *, #14447, .F. ) ;
#38292 = CARTESIAN_POINT ( 'NONE',  ( -11.88016137193916677, -19.16921147633432199, 71.57197012879584008 ) ) ;
#38293 = CARTESIAN_POINT ( 'NONE',  ( -12.10369268100898132, -9.594121713099781346, 57.27430968559156810 ) ) ;
#38294 = VERTEX_POINT ( 'NONE', #30288 ) ;
#38295 = FACE_BOUND ( 'NONE', #17638, .T. ) ;
#38296 = ORIENTED_EDGE ( 'NONE', *, *, #17120, .T. ) ;
#38297 = ORIENTED_EDGE ( 'NONE', *, *, #8995, .F. ) ;
#38298 = ORIENTED_EDGE ( 'NONE', *, *, #28769, .F. ) ;
#38299 = LINE ( 'NONE', #30711, #12351 ) ;
#38300 = CARTESIAN_POINT ( 'NONE',  ( -13.41559485503361948, -8.529420403834853559, 57.08472365561223683 ) ) ;
#38301 = CARTESIAN_POINT ( 'NONE',  ( -12.18170072908086965, -10.17053062278287889, 64.32914326641392222 ) ) ;
#38302 = CARTESIAN_POINT ( 'NONE',  ( -11.85162103594838001, -10.49015045520576983, 71.25420998615621215 ) ) ;
#38303 = EDGE_CURVE ( 'NONE', #22272, #38392, #22115, .T. ) ;
#38304 = CARTESIAN_POINT ( 'NONE',  ( -17.92193097897699872, -21.84160713959417421, 62.17535923543130139 ) ) ;
#38305 = CARTESIAN_POINT ( 'NONE',  ( -19.82409385541304303, -9.359200813967568422, 50.49621490985803263 ) ) ;
#38306 = EDGE_CURVE ( 'NONE', #44794, #33937, #11555, .T. ) ;
#38307 = VECTOR ( 'NONE', #13163, 1000.000000000000000 ) ;
#38308 = AXIS2_PLACEMENT_3D ( 'NONE', #22987, #19269, #45873 ) ;
#38309 = ORIENTED_EDGE ( 'NONE', *, *, #31301, .T. ) ;
#38310 = EDGE_LOOP ( 'NONE', ( #42311, #36501, #29047, #15309, #6157 ) ) ;
#38311 = CARTESIAN_POINT ( 'NONE',  ( -20.92409385650551812, -6.426201560718813433, 50.50509628382439331 ) ) ;
#38312 = EDGE_CURVE ( 'NONE', #29465, #40716, #5212, .T. ) ;
#38313 = EDGE_CURVE ( 'NONE', #45950, #23554, #46283, .T. ) ;
#38314 = CARTESIAN_POINT ( 'NONE',  ( -9.995623895585607599, -14.24219643007072023, 64.64449787557668969 ) ) ;
#38315 = DIRECTION ( 'NONE',  ( -0.4749924142254751680, -0.8799898899579781109, -8.916637576350562172E-09 ) ) ;
#38316 = AXIS2_PLACEMENT_3D ( 'NONE', #20313, #24513, #28189 ) ;
#38317 = CARTESIAN_POINT ( 'NONE',  ( -21.60699298862427398, -9.194826105172156261, 70.20302893975198799 ) ) ;
#38318 = ORIENTED_EDGE ( 'NONE', *, *, #6611, .T. ) ;
#38319 = CARTESIAN_POINT ( 'NONE',  ( -15.99909385650551741, -8.114302828567740988, 52.18300498402516041 ) ) ;
#38320 = ORIENTED_EDGE ( 'NONE', *, *, #29716, .T. ) ;
#38321 = CARTESIAN_POINT ( 'NONE',  ( -11.62344814847972252, -18.82242928093252843, 71.77866150141453261 ) ) ;
#38322 = CARTESIAN_POINT ( 'NONE',  ( -15.79771479060332240, -19.20445095063907104, 49.52966884056656482 ) ) ;
#38323 = CARTESIAN_POINT ( 'NONE',  ( -24.46506320217640962, -17.24406362331221132, 72.99840605271779737 ) ) ;
#38324 =( BOUNDED_CURVE ( )  B_SPLINE_CURVE ( 3, ( #20779, #42716, #32105, #12659 ),
 .UNSPECIFIED., .F., .F. ) 
 B_SPLINE_CURVE_WITH_KNOTS ( ( 4, 4 ),
 ( 0.9074455897393626236, 1.000000000000000000 ),
 .UNSPECIFIED. ) 
 CURVE ( )  GEOMETRIC_REPRESENTATION_ITEM ( )  RATIONAL_B_SPLINE_CURVE ( ( 0.6983129098261133816, 0.7760317562607157438, 0.8765941196520112833, 1.000000000000000000 ) ) 
 REPRESENTATION_ITEM ( '' )  );
#38325 = EDGE_LOOP ( 'NONE', ( #32758, #26819, #24497, #34460 ) ) ;
#38326 = CARTESIAN_POINT ( 'NONE',  ( -26.92409385541305511, -6.859206544744110623, 47.99999999999997868 ) ) ;
#38327 = LINE ( 'NONE', #16411, #39793 ) ;
#38328 = EDGE_CURVE ( 'NONE', #10862, #36372, #15718, .T. ) ;
#38329 = FACE_OUTER_BOUND ( 'NONE', #20565, .T. ) ;
#38330 = ORIENTED_EDGE ( 'NONE', *, *, #3886, .T. ) ;
#38331 = VECTOR ( 'NONE', #29939, 1000.000000000000000 ) ;
#38332 = CARTESIAN_POINT ( 'NONE',  ( -12.27604185553471616, -19.62628656662749549, 58.21210303282668264 ) ) ;
#38333 = DIRECTION ( 'NONE',  ( 0.000000000000000000, 0.000000000000000000, -1.000000000000000000 ) ) ;
#38334 = CYLINDRICAL_SURFACE ( 'NONE', #28436, 4.686499999999997002 ) ;
#38335 = ORIENTED_EDGE ( 'NONE', *, *, #31932, .F. ) ;
#38336 =( BOUNDED_SURFACE ( )  B_SPLINE_SURFACE ( 3, 1, ( 
 ( #4396, #14964 ),
 ( #27047, #26820 ),
 ( #8112, #19669 ),
 ( #23358, #30029 ),
 ( #45059, #23125 ),
 ( #19412, #4640 ),
 ( #15706, #30761 ) ),
 .UNSPECIFIED., .T., .F., .F. ) 
 B_SPLINE_SURFACE_WITH_KNOTS ( ( 4, 3, 4 ),
 ( 2, 2 ),
 ( 0.000000000000000000, 0.5000000000000000000, 1.000000000000000000 ),
 ( 0.000000000000000000, 1.000000000000000000 ),
 .UNSPECIFIED. ) 
 GEOMETRIC_REPRESENTATION_ITEM ( )  RATIONAL_B_SPLINE_SURFACE ( (
 ( 1.000000000000000000, 1.000000000000000000),
 ( 0.3333333333333335369, 0.3333333333333330373),
 ( 0.3333333333333335369, 0.3333333333333330373),
 ( 1.000000000000000000, 1.000000000000000000),
 ( 0.3333333333333333703, 0.3333333333333333703),
 ( 0.3333333333333333703, 0.3333333333333333703),
 ( 1.000000000000000000, 1.000000000000000000) ) ) 
 REPRESENTATION_ITEM ( '' )  SURFACE ( )  );
#38337 = AXIS2_PLACEMENT_3D ( 'NONE', #24934, #14300, #10409 ) ;
#38338 = AXIS2_PLACEMENT_3D ( 'NONE', #41634, #34225, #34469 ) ;
#38339 = ORIENTED_EDGE ( 'NONE', *, *, #29114, .F. ) ;
#38340 = DIRECTION ( 'NONE',  ( -0.1240347345892086062, 1.145860353393066553E-16, -0.9922778767136676281 ) ) ;
#38341 = CARTESIAN_POINT ( 'NONE',  ( -24.72725712452650981, -16.28144042551206638, 62.84974626185121593 ) ) ;
#38343 = ADVANCED_FACE ( 'NONE', ( #16448 ), #31004, .T. ) ;
#38342 = ORIENTED_EDGE ( 'NONE', *, *, #20479, .F. ) ;
#38344 = CARTESIAN_POINT ( 'NONE',  ( -10.43125871347677958, -13.91323993190135155, 57.59825034919892772 ) ) ;
#38345 = CARTESIAN_POINT ( 'NONE',  ( -17.96757567997740423, -21.83837585814599080, 62.16976149166120535 ) ) ;
#38346 = CARTESIAN_POINT ( 'NONE',  ( -14.28223569189418996, -8.054058993954978263, 67.36700916836338138 ) ) ;
#38347 = ORIENTED_EDGE ( 'NONE', *, *, #9006, .T. ) ;
#38348 = CARTESIAN_POINT ( 'NONE',  ( -15.39536932222403287, -19.92137602241599836, 54.07175714974879099 ) ) ;
#38349 = VECTOR ( 'NONE', #34668, 1000.000000000000000 ) ;
#38350 = CARTESIAN_POINT ( 'NONE',  ( -41.80424091423659405, -14.80920654474421205, 67.95882352941174531 ) ) ;
#38351 = CARTESIAN_POINT ( 'NONE',  ( -22.27817919856018136, -9.157513542003881568, 59.83675792137641736 ) ) ;
#38352 = VERTEX_POINT ( 'NONE', #24343 ) ;
#38353 = CARTESIAN_POINT ( 'NONE',  ( -11.46028008028683942, -18.56947564720590194, 61.56238700194530367 ) ) ;
#38354 = CIRCLE ( 'NONE', #21849, 1.249999999999999334 ) ;
#38355 = CARTESIAN_POINT ( 'NONE',  ( -11.60247201135026884, -18.79965542285971836, 61.43277710409636683 ) ) ;
#38356 = ORIENTED_EDGE ( 'NONE', *, *, #39480, .F. ) ;
#38357 = ORIENTED_EDGE ( 'NONE', *, *, #7248, .T. ) ;
#38358 = B_SPLINE_CURVE_WITH_KNOTS ( 'NONE', 3,
 ( #8436, #27634, #19770, #34526, #23949, #46603, #34778, #5479, #4495, #8930 ),
 .UNSPECIFIED., .F., .F.,
 ( 4, 2, 2, 2, 4 ),
 ( 0.000000000000000000, 0.2500000000000000000, 0.5000000000000000000, 0.7500000000000000000, 1.000000000000000000 ),
 .UNSPECIFIED. ) ;
#38359 = CARTESIAN_POINT ( 'NONE',  ( -22.85634334395279055, -10.39183557728184581, 66.65255357689962068 ) ) ;
#38360 = LINE ( 'NONE', #23622, #23444 ) ;
#38361 = FACE_OUTER_BOUND ( 'NONE', #2668, .T. ) ;
#38362 = CARTESIAN_POINT ( 'NONE',  ( -13.16159385759798894, -7.228003583438117552, 51.38655588711986155 ) ) ;
#38363 = CARTESIAN_POINT ( 'NONE',  ( 10.57590614458695377, 3.140741878271521514, 50.53406581128081143 ) ) ;
#38364 = CARTESIAN_POINT ( 'NONE',  ( -11.93195840498443516, -10.38844327383712773, 70.98365212470247343 ) ) ;
#38365 = CARTESIAN_POINT ( 'NONE',  ( -23.26031998850344706, -18.67503058230525070, 69.57755490092647221 ) ) ;
#38366 = CARTESIAN_POINT ( 'NONE',  ( -12.10131192688100299, -10.18592936015514816, 64.31442259820508411 ) ) ;
#38367 = ORIENTED_EDGE ( 'NONE', *, *, #18386, .T. ) ;
#38368 = ORIENTED_EDGE ( 'NONE', *, *, #23943, .F. ) ;
#38369 = CARTESIAN_POINT ( 'NONE',  ( -22.44308142039503906, -9.846875392603276822, 70.16745681354213104 ) ) ;
#38370 = EDGE_CURVE ( 'NONE', #38839, #17452, #27888, .T. ) ;
#38371 = EDGE_CURVE ( 'NONE', #6771, #8867, #37440, .T. ) ;
#38372 = CARTESIAN_POINT ( 'NONE',  ( -14.54324430907851173, -21.67975036377454501, 58.42263788831355953 ) ) ;
#38373 = AXIS2_PLACEMENT_3D ( 'NONE', #17336, #9244, #1848 ) ;
#38374 = CARTESIAN_POINT ( 'NONE',  ( -10.92506019527676209, -17.54181618899167105, 68.39162186085954431 ) ) ;
#38375 = CARTESIAN_POINT ( 'NONE',  ( -12.47486999026313015, -19.83014042270297494, 64.87234644051179089 ) ) ;
#38376 = VECTOR ( 'NONE', #31115, 1000.000000000000000 ) ;
#38377 = VECTOR ( 'NONE', #15638, 1000.000000000000000 ) ;
#38378 = VERTEX_POINT ( 'NONE', #27546 ) ;
#38379 = AXIS2_PLACEMENT_3D ( 'NONE', #5848, #40531, #17400 ) ;
#38380 = EDGE_CURVE ( 'NONE', #26170, #42514, #20155, .T. ) ;
#38381 = EDGE_CURVE ( 'NONE', #6140, #8644, #42183, .T. ) ;
#38382 = ORIENTED_EDGE ( 'NONE', *, *, #12476, .T. ) ;
#38383 = CARTESIAN_POINT ( 'NONE',  ( -24.47401588645412573, -14.84236399432835540, 59.39300237059229914 ) ) ;
#38384 = FACE_OUTER_BOUND ( 'NONE', #5760, .T. ) ;
#38385 = CARTESIAN_POINT ( 'NONE',  ( -14.91602154273002689, -21.82451726398313241, 65.24563297375915738 ) ) ;
#38386 = CARTESIAN_POINT ( 'NONE',  ( -11.40682184329331506, -18.48987001057684765, 65.04707367406611240 ) ) ;
#38387 = CIRCLE ( 'NONE', #34450, 5.249999999999998224 ) ;
#38388 = VERTEX_POINT ( 'NONE', #35165 ) ;
#38389 = DIRECTION ( 'NONE',  ( -1.000000000000000000, 0.000000000000000000, 5.466375705775733989E-17 ) ) ;
#38390 = CARTESIAN_POINT ( 'NONE',  ( -24.78816760170556677, -15.94238017617776215, 69.71962869939886787 ) ) ;
#38391 = EDGE_CURVE ( 'NONE', #25725, #12617, #1435, .T. ) ;
#38392 = VERTEX_POINT ( 'NONE', #15961 ) ;
#38393 = CARTESIAN_POINT ( 'NONE',  ( -12.83007325466668114, -20.09077588727113550, 72.10653676829758751 ) ) ;
#38394 = DIRECTION ( 'NONE',  ( -3.071710424422018668E-17, 6.404604876783312462E-16, 1.000000000000000000 ) ) ;
#38395 = ORIENTED_EDGE ( 'NONE', *, *, #3132, .T. ) ;
#38396 = CARTESIAN_POINT ( 'NONE',  ( -12.41315173547891781, -9.850077678253004621, 57.38935532239157311 ) ) ;
#38397 = ORIENTED_EDGE ( 'NONE', *, *, #12942, .T. ) ;
#38398 = CARTESIAN_POINT ( 'NONE',  ( -45.36800283045199933, -16.43194983366105077, 70.50000000000000000 ) ) ;
#38399 = CARTESIAN_POINT ( 'NONE',  ( -10.61330293760801879, -12.98832031645814844, 67.88832347272310130 ) ) ;
#38400 = EDGE_LOOP ( 'NONE', ( #32500, #20760, #12567 ) ) ;
#38401 = CARTESIAN_POINT ( 'NONE',  ( -13.35550522631041837, -8.568183888810063209, 57.15463030501995689 ) ) ;
#38402 = EDGE_CURVE ( 'NONE', #46585, #5353, #42824, .T. ) ;
#38403 = CARTESIAN_POINT ( 'NONE',  ( -18.24929096724884658, -21.81104555038653103, 68.82986815895560540 ) ) ;
#38404 = CARTESIAN_POINT ( 'NONE',  ( -18.67409385650551457, -9.792211528768504536, 50.49490371617623197 ) ) ;
#38405 = VECTOR ( 'NONE', #12320, 1000.000000000000227 ) ;
#38406 = CARTESIAN_POINT ( 'NONE',  ( -16.50258162057404832, -20.23145840177225807, 53.49999999999995026 ) ) ;
#38407 = COLOUR_RGB ( '', 0.31764706, 0.68627451, 0.89019608) ;
#38408 = CARTESIAN_POINT ( 'NONE',  ( -24.43375969181978036, -15.56263427672455713, 73.30303726254599894 ) ) ;
#38409 = LINE ( 'NONE', #8392, #29000 ) ;
#38410 = ORIENTED_EDGE ( 'NONE', *, *, #20048, .T. ) ;
#38411 = CARTESIAN_POINT ( 'NONE',  ( -19.15013325158599855, -21.59352074159554746, 58.54124067949265253 ) ) ;
#38412 = AXIS2_PLACEMENT_3D ( 'NONE', #43666, #46863, #17036 ) ;
#38413 = AXIS2_PLACEMENT_3D ( 'NONE', #20262, #35516, #31828 ) ;
#38414 = CARTESIAN_POINT ( 'NONE',  ( -18.11396434131172128, -21.77512919714542150, 65.34532159443909904 ) ) ;
#38415 = CARTESIAN_POINT ( 'NONE',  ( -19.98813035779708969, -21.37641423362171267, 72.55478737316022375 ) ) ;
#38416 = B_SPLINE_CURVE_WITH_KNOTS ( 'NONE', 1,
 ( #37585, #26527 ),
 .UNSPECIFIED., .F., .F.,
 ( 2, 2 ),
 ( 0.000000000000000000, 1.000000000000000000 ),
 .UNSPECIFIED. ) ;
#38417 = CARTESIAN_POINT ( 'NONE',  ( -18.38341875142146975, -21.74322078448643225, 69.10049320035381015 ) ) ;
#38418 = CARTESIAN_POINT ( 'NONE',  ( -12.25434429315920859, -20.17366997322574562, 65.05170215947674706 ) ) ;
#38419 = ORIENTED_EDGE ( 'NONE', *, *, #21006, .F. ) ;
#38420 = ORIENTED_EDGE ( 'NONE', *, *, #28736, .F. ) ;
#38421 = CARTESIAN_POINT ( 'NONE',  ( -18.46801905451614090, -7.836623195388690455, 74.12592262855558545 ) ) ;
#38422 = DIRECTION ( 'NONE',  ( -3.071710424422018668E-17, 6.404604876783312462E-16, 1.000000000000000000 ) ) ;
#38423 = ORIENTED_EDGE ( 'NONE', *, *, #2653, .F. ) ;
#38424 = CARTESIAN_POINT ( 'NONE',  ( -10.37255316239921044, -15.11044245508572459, 57.71225695896244190 ) ) ;
#38425 = CARTESIAN_POINT ( 'NONE',  ( -16.36834455927873222, -22.18410795223847387, 61.94063518049016182 ) ) ;
#38426 = AXIS2_PLACEMENT_3D ( 'NONE', #25692, #10928, #10681 ) ;
#38427 = CARTESIAN_POINT ( 'NONE',  ( -20.75235147695052262, -8.143923935286606408, 63.41847357668724072 ) ) ;
#38428 = FACE_OUTER_BOUND ( 'NONE', #20414, .T. ) ;
#38429 = CARTESIAN_POINT ( 'NONE',  ( -14.22441598498101989, -8.081217260141077219, 67.44470407312981308 ) ) ;
#38430 = CARTESIAN_POINT ( 'NONE',  ( -12.26157393735297596, -10.08170764524057894, 60.84452776435725951 ) ) ;
#38431 = CARTESIAN_POINT ( 'NONE',  ( -13.98092790585787171, -8.714500222849059341, 74.27242791210171902 ) ) ;
#38432 = ORIENTED_EDGE ( 'NONE', *, *, #26119, .F. ) ;
#38433 = CARTESIAN_POINT ( 'NONE',  ( -17.42409385541299471, -14.80920654474435771, 49.52966884056655772 ) ) ;
#38434 = EDGE_CURVE ( 'NONE', #25059, #27904, #18698, .T. ) ;
#38435 = DIRECTION ( 'NONE',  ( -3.071710424422018668E-17, 6.404604876783312462E-16, 1.000000000000000000 ) ) ;
#38436 = CARTESIAN_POINT ( 'NONE',  ( -15.50784783684063051, -8.076599273749138774, 74.07985659288991087 ) ) ;
#38437 = CARTESIAN_POINT ( 'NONE',  ( -13.77834346862332637, -20.78674830809137575, 68.56698313520011823 ) ) ;
#38438 = CARTESIAN_POINT ( 'NONE',  ( -17.46222794319647775, -7.759011850482251837, 67.03511641684839617 ) ) ;
#38439 = DIRECTION ( 'NONE',  ( 0.000000000000000000, 1.000000000000000000, 0.000000000000000000 ) ) ;
#38440 = ORIENTED_EDGE ( 'NONE', *, *, #16181, .F. ) ;
#38441 = VERTEX_POINT ( 'NONE', #2880 ) ;
#38442 = ADVANCED_FACE ( 'NONE', ( #6594 ), #25066, .T. ) ;
#38443 = CARTESIAN_POINT ( 'NONE',  ( -22.07409385650551670, -9.792211528768504536, 50.49490371617623197 ) ) ;
#38444 = EDGE_CURVE ( 'NONE', #28641, #25463, #44279, .T. ) ;
#38445 = VERTEX_POINT ( 'NONE', #47480 ) ;
#38446 = CARTESIAN_POINT ( 'NONE',  ( -17.56717618076180187, -7.360494862701306928, 63.73552352176282909 ) ) ;
#38447 = EDGE_CURVE ( 'NONE', #24840, #6635, #12047, .T. ) ;
#38448 = AXIS2_PLACEMENT_3D ( 'NONE', #43810, #10069, #47004 ) ;
#38449 = CARTESIAN_POINT ( 'NONE',  ( -24.10582418872880694, -12.72205642837049311, 69.77242970670894806 ) ) ;
#38450 = EDGE_CURVE ( 'NONE', #10157, #7981, #28276, .T. ) ;
#38451 = B_SPLINE_CURVE_WITH_KNOTS ( 'NONE', 1,
 ( #41514, #22823 ),
 .UNSPECIFIED., .F., .F.,
 ( 2, 2 ),
 ( 0.000000000000000000, 1.000000000000000000 ),
 .UNSPECIFIED. ) ;
#38452 = EDGE_LOOP ( 'NONE', ( #20965, #16772, #14514, #47424 ) ) ;
#38453 = VECTOR ( 'NONE', #28565, 1000.000000000000227 ) ;
#38454 = DIRECTION ( 'NONE',  ( -0.9979768094191907579, -0.06357898915123130767, 0.000000000000000000 ) ) ;
#38455 = CARTESIAN_POINT ( 'NONE',  ( -13.49909385759798930, -8.105421454601382081, 49.25000573077640098 ) ) ;
#38456 = CARTESIAN_POINT ( 'NONE',  ( -19.66559402580761784, -10.06176755239059695, 50.77966884056655772 ) ) ;
#38457 = EDGE_CURVE ( 'NONE', #35856, #19379, #22208, .T. ) ;
#38458 = EDGE_LOOP ( 'NONE', ( #4366, #25706, #41775, #39096, #38237, #19618, #46786 ) ) ;
#38459 = CARTESIAN_POINT ( 'NONE',  ( -13.89388974506275787, -21.36980381032900667, 72.11102993026078423 ) ) ;
#38460 = AXIS2_PLACEMENT_3D ( 'NONE', #8833, #37932, #46960 ) ;
#38461 = CARTESIAN_POINT ( 'NONE',  ( -10.46492739217203471, -14.05366762209630949, 57.52113007005035428 ) ) ;
#38462 = ORIENTED_EDGE ( 'NONE', *, *, #30311, .T. ) ;
#38463 = LINE ( 'NONE', #38710, #46176 ) ;
#38464 = FACE_OUTER_BOUND ( 'NONE', #1194, .T. ) ;
#38465 = ORIENTED_EDGE ( 'NONE', *, *, #43150, .T. ) ;
#38466 = CARTESIAN_POINT ( 'NONE',  ( -23.16117746674104438, -18.90708040007733359, 62.63934749780565880 ) ) ;
#38467 = CARTESIAN_POINT ( 'NONE',  ( -22.53655473247544805, -20.22829521909097394, 65.88917159596024931 ) ) ;
#38468 = CARTESIAN_POINT ( 'NONE',  ( -24.01409443880168126, -12.44853925549632301, 73.46898916292617798 ) ) ;
#38469 = ORIENTED_EDGE ( 'NONE', *, *, #47945, .F. ) ;
#38470 = CARTESIAN_POINT ( 'NONE',  ( -23.21283044961208830, -10.11939778159179859, 63.25681392212788268 ) ) ;
#38471 = CARTESIAN_POINT ( 'NONE',  ( -17.85939470442713883, -21.79572004712530386, 58.63226791514592406 ) ) ;
#38472 =( BOUNDED_CURVE ( )  B_SPLINE_CURVE ( 3, ( #40069, #20868, #29466, #21367 ),
 .UNSPECIFIED., .F., .F. ) 
 B_SPLINE_CURVE_WITH_KNOTS ( ( 4, 4 ),
 ( 0.000000000000000000, 0.4074455897393624570 ),
 .UNSPECIFIED. ) 
 CURVE ( )  GEOMETRIC_REPRESENTATION_ITEM ( )  RATIONAL_B_SPLINE_CURVE ( ( 1.000000000000000000, 0.4567392136813345216, 0.3561768502900312661, 0.6983129098260902889 ) ) 
 REPRESENTATION_ITEM ( '' )  );
#38473 = CARTESIAN_POINT ( 'NONE',  ( -16.22585566360328357, -7.910893225427095388, 63.85938213801649255 ) ) ;
#38474 = DIRECTION ( 'NONE',  ( 0.000000000000000000, 0.000000000000000000, -1.000000000000000000 ) ) ;
#38475 = B_SPLINE_CURVE_WITH_KNOTS ( 'NONE', 1,
 ( #38623, #34924 ),
 .UNSPECIFIED., .F., .F.,
 ( 2, 2 ),
 ( 0.000000000000000000, 1.000000000000000000 ),
 .UNSPECIFIED. ) ;
#38476 = CYLINDRICAL_SURFACE ( 'NONE', #2245, 7.500000000000001776 ) ;
#38477 = CARTESIAN_POINT ( 'NONE',  ( -14.66630222544869078, -8.320656262913125545, 63.80450889863892172 ) ) ;
#38478 = DIRECTION ( 'NONE',  ( 1.927470528863119542E-16, 0.000000000000000000, -1.000000000000000000 ) ) ;
#38479 = CARTESIAN_POINT ( 'NONE',  ( -6.424093855413055110, -25.10920654474410441, 45.99999999999998579 ) ) ;
#38480 = CYLINDRICAL_SURFACE ( 'NONE', #10281, 5.249999999999998224 ) ;
#38481 = CARTESIAN_POINT ( 'NONE',  ( -14.87409385650551741, -9.792211528768504536, 50.49490371617623197 ) ) ;
#38482 = VERTEX_POINT ( 'NONE', #36599 ) ;
#38483 = AXIS2_PLACEMENT_3D ( 'NONE', #27870, #24677, #16775 ) ;
#38484 = DIRECTION ( 'NONE',  ( 8.260587980841940012E-17, 0.000000000000000000, -1.000000000000000000 ) ) ;
#38485 = CARTESIAN_POINT ( 'NONE',  ( -10.46593773880539047, -17.47129530308245293, 64.72715759520706058 ) ) ;
#38486 = ORIENTED_EDGE ( 'NONE', *, *, #39548, .F. ) ;
#38487 = CARTESIAN_POINT ( 'NONE',  ( -13.84085632603101956, -17.84827948783496865, 49.52966884056656482 ) ) ;
#38488 = CARTESIAN_POINT ( 'NONE',  ( -10.61606246679250631, -17.83465121431504841, 71.76729389568697570 ) ) ;
#38489 = CARTESIAN_POINT ( 'NONE',  ( -22.36602013069261119, -13.03724021049842996, 52.02966884056656482 ) ) ;
#38490 = FACE_OUTER_BOUND ( 'NONE', #20481, .T. ) ;
#38491 = EDGE_CURVE ( 'NONE', #48314, #24620, #11650, .T. ) ;
#38492 =( BOUNDED_SURFACE ( )  B_SPLINE_SURFACE ( 3, 1, ( 
 ( #13130, #5541 ),
 ( #1586, #12668 ),
 ( #1833, #23771 ),
 ( #27693, #16595 ),
 ( #20061, #35065 ),
 ( #42723, #31636 ),
 ( #20563, #35556 ) ),
 .UNSPECIFIED., .T., .F., .F. ) 
 B_SPLINE_SURFACE_WITH_KNOTS ( ( 4, 3, 4 ),
 ( 2, 2 ),
 ( 0.000000000000000000, 0.5000000000000000000, 1.000000000000000000 ),
 ( 0.000000000000000000, 1.000000000000000000 ),
 .UNSPECIFIED. ) 
 GEOMETRIC_REPRESENTATION_ITEM ( )  RATIONAL_B_SPLINE_SURFACE ( (
 ( 1.000000000000000000, 1.000000000000000000),
 ( 0.3333333333333335369, 0.3333333333333330373),
 ( 0.3333333333333335369, 0.3333333333333330373),
 ( 1.000000000000000000, 1.000000000000000000),
 ( 0.3333333333333333703, 0.3333333333333333703),
 ( 0.3333333333333333703, 0.3333333333333333703),
 ( 1.000000000000000000, 1.000000000000000000) ) ) 
 REPRESENTATION_ITEM ( '' )  SURFACE ( )  );
#38493 = VERTEX_POINT ( 'NONE', #43306 ) ;
#38494 =( BOUNDED_CURVE ( )  B_SPLINE_CURVE ( 2, ( #44901, #15063, #33278, #7474, #30120, #18274, #22729, #47842, #7712 ),
 .UNSPECIFIED., .F., .F. ) 
 B_SPLINE_CURVE_WITH_KNOTS ( ( 3, 2, 2, 2, 3 ),
 ( 0.6249999999999998890, 0.6354166666666665186, 0.6458333333333332593, 0.6562499999999998890, 0.6666666666666665186 ),
 .UNSPECIFIED. ) 
 CURVE ( )  GEOMETRIC_REPRESENTATION_ITEM ( )  RATIONAL_B_SPLINE_CURVE ( ( 1.000000000000000888, 0.9238795325112859613, 1.000000000000000000, 0.9238795325112867385, 1.000000000000000000, 0.9238795325112867385, 1.000000000000000000, 0.9238795325112875156, 0.9999999999999992228 ) ) 
 REPRESENTATION_ITEM ( '' )  );
#38495 = PLANE ( 'NONE',  #346 ) ;
#38496 = AXIS2_PLACEMENT_3D ( 'NONE', #16187, #30994, #19671 ) ;
#38497 = VECTOR ( 'NONE', #16446, 1000.000000000000114 ) ;
#38498 = FACE_OUTER_BOUND ( 'NONE', #22184, .T. ) ;
#38499 = CARTESIAN_POINT ( 'NONE',  ( -18.95312625172554633, -7.978243212125802231, 63.62192339619330994 ) ) ;
#38500 = EDGE_CURVE ( 'NONE', #24292, #33660, #9812, .T. ) ;
#38501 = VERTEX_POINT ( 'NONE', #6103 ) ;
#38502 = AXIS2_PLACEMENT_3D ( 'NONE', #9629, #32270, #12813 ) ;
#38503 = DIRECTION ( 'NONE',  ( -9.637352644315596475E-17, 0.000000000000000000, -1.000000000000000000 ) ) ;
#38504 = CARTESIAN_POINT ( 'NONE',  ( -10.44216256679811217, -13.77595636612621988, 61.06254307272654813 ) ) ;
#38505 = CARTESIAN_POINT ( 'NONE',  ( -21.72478623736860470, -8.725751437694626134, 70.30849399937490318 ) ) ;
#38506 = CARTESIAN_POINT ( 'NONE',  ( -12.15399301493812878, -9.543295845094297292, 57.20440096431307353 ) ) ;
#38507 =( BOUNDED_CURVE ( )  B_SPLINE_CURVE ( 3, ( #35449, #1734, #31767, #44548 ),
 .UNSPECIFIED., .F., .F. ) 
 B_SPLINE_CURVE_WITH_KNOTS ( ( 4, 4 ),
 ( 0.5000000000000000000, 0.9074455897393640669 ),
 .UNSPECIFIED. ) 
 CURVE ( )  GEOMETRIC_REPRESENTATION_ITEM ( )  RATIONAL_B_SPLINE_CURVE ( ( 0.9999999999999911182, 0.4567392136813318571, 0.3561768502900363731, 0.6983129098260949519 ) ) 
 REPRESENTATION_ITEM ( '' )  );
#38508 = VERTEX_POINT ( 'NONE', #6351 ) ;
#38509 = ORIENTED_EDGE ( 'NONE', *, *, #15889, .T. ) ;
#38510 = CARTESIAN_POINT ( 'NONE',  ( -23.08659385541304587, -7.222650657624104298, 49.61879703869476543 ) ) ;
#38511 = CARTESIAN_POINT ( 'NONE',  ( -24.39763799706551950, -15.84669482609578317, 69.54779622430706354 ) ) ;
#38512 = ADVANCED_FACE ( 'NONE', ( #20887 ), #10293, .T. ) ;
#38513 = CARTESIAN_POINT ( 'NONE',  ( -10.45863924090583552, -14.11462608630872317, 61.21821294130609914 ) ) ;
#38514 = ADVANCED_FACE ( 'NONE', ( #17164 ), #30609, .T. ) ;
#38515 = EDGE_CURVE ( 'NONE', #15132, #6650, #33333, .T. ) ;
#38516 = CARTESIAN_POINT ( 'NONE',  ( -17.79108452803360763, -21.84994637594637723, 58.69081321602850920 ) ) ;
#38517 = DIRECTION ( 'NONE',  ( 6.374839753205896285E-22, 0.007114381193220324640, -0.9999746924698832418 ) ) ;
#38518 = AXIS2_PLACEMENT_3D ( 'NONE', #6858, #25094, #36875 ) ;
#38519 = CARTESIAN_POINT ( 'NONE',  ( -20.25445156252866497, -7.916983464207429932, 73.90751836168473687 ) ) ;
#38520 = CIRCLE ( 'NONE', #17289, 0.6570903894995150374 ) ;
#38521 = DIRECTION ( 'NONE',  ( -0.3478314405900309603, -0.9375570856950864451, 9.567072274253696421E-17 ) ) ;
#38522 = ADVANCED_FACE ( 'NONE', ( #29726 ), #37578, .T. ) ;
#38523 = ORIENTED_EDGE ( 'NONE', *, *, #32601, .F. ) ;
#38524 = CARTESIAN_POINT ( 'NONE',  ( -21.19335713336021243, -20.70964345786463312, 72.71373614481359482 ) ) ;
#38525 = CARTESIAN_POINT ( 'NONE',  ( -24.16575376147897458, -12.74704232990201547, 69.77243002240838621 ) ) ;
#38526 = ORIENTED_EDGE ( 'NONE', *, *, #18122, .F. ) ;
#38527 = CYLINDRICAL_SURFACE ( 'NONE', #46530, 0.1500000000000080158 ) ;
#38528 = CARTESIAN_POINT ( 'NONE',  ( -10.48067351556794158, -16.03044098841782628, 68.27767830705533925 ) ) ;
#38529 = VERTEX_POINT ( 'NONE', #22844 ) ;
#38530 = DIRECTION ( 'NONE',  ( -8.329294163758554984E-07, 2.487164605953353708E-06, -0.9999999999965601960 ) ) ;
#38531 = CARTESIAN_POINT ( 'NONE',  ( -10.00830686992707896, -15.52368892135347878, 57.74509703396581983 ) ) ;
#38532 = B_SPLINE_CURVE_WITH_KNOTS ( 'NONE', 3,
 ( #41876, #41135, #33979, #11580, #14747, #27088, #275, #22671, #3964, #15254 ),
 .UNSPECIFIED., .F., .F.,
 ( 4, 2, 2, 2, 4 ),
 ( 0.000000000000000000, 0.2500000000000000000, 0.5000000000000000000, 0.7500000000000000000, 1.000000000000000000 ),
 .UNSPECIFIED. ) ;
#38533 = CARTESIAN_POINT ( 'NONE',  ( -13.35819042472069107, -21.05197888995676436, 61.70141705377209007 ) ) ;
#38534 = DIRECTION ( 'NONE',  ( 0.000000000000000000, 0.000000000000000000, 1.000000000000000000 ) ) ;
#38535 = VERTEX_POINT ( 'NONE', #44511 ) ;
#38536 = CARTESIAN_POINT ( 'NONE',  ( -22.11925914797909343, -9.024813657292067859, 63.30658454184609241 ) ) ;
#38537 = CARTESIAN_POINT ( 'NONE',  ( -20.82598581164736018, -21.43720942579135524, 58.75201007894592919 ) ) ;
#38538 = LINE ( 'NONE', #4821, #29405 ) ;
#38539 = FACE_BOUND ( 'NONE', #46645, .T. ) ;
#38540 = CONTEXT_DEPENDENT_SHAPE_REPRESENTATION ( #43240, #5208 ) ;
#38541 = CARTESIAN_POINT ( 'NONE',  ( -27.42409385541305156, -14.65920654474411045, 47.99999999999997868 ) ) ;
#38542 = CARTESIAN_POINT ( 'NONE',  ( -17.42409385541299471, -14.80920654474435594, 52.02966884056656482 ) ) ;
#38543 = DIRECTION ( 'NONE',  ( 1.294152349642661695E-15, -0.8949343913984055821, -0.4461977533475101065 ) ) ;
#38544 = ORIENTED_EDGE ( 'NONE', *, *, #39795, .F. ) ;
#38545 = CARTESIAN_POINT ( 'NONE',  ( -24.47401588439613818, -14.84236418521736312, 59.54300237059217693 ) ) ;
#38546 = VERTEX_POINT ( 'NONE', #11496 ) ;
#38547 = CARTESIAN_POINT ( 'NONE',  ( -16.67409385541329669, -6.859212275519744217, 50.50378509014024075 ) ) ;
#38548 = CARTESIAN_POINT ( 'NONE',  ( -16.79748725893476546, -22.23297595151960238, 68.83414125832270258 ) ) ;
#38549 = ADVANCED_FACE ( 'NONE', ( #7339 ), #34137, .T. ) ;
#38550 = ORIENTED_EDGE ( 'NONE', *, *, #14225, .T. ) ;
#38551 = CARTESIAN_POINT ( 'NONE',  ( -24.35389707626741185, -16.10709931453380861, 62.87856533165624029 ) ) ;
#38552 = FACE_BOUND ( 'NONE', #30865, .T. ) ;
#38553 = ORIENTED_EDGE ( 'NONE', *, *, #45348, .T. ) ;
#38554 = ORIENTED_EDGE ( 'NONE', *, *, #21274, .F. ) ;
#38555 = ORIENTED_EDGE ( 'NONE', *, *, #19779, .F. ) ;
#38557 = CARTESIAN_POINT ( 'NONE',  ( -18.12717186014929283, -21.82707771419581633, 61.76047256604253732 ) ) ;
#38556 = VECTOR ( 'NONE', #37548, 1000.000000000000000 ) ;
#38558 = SURFACE_STYLE_USAGE ( .BOTH. , #17047 ) ;
#38559 = LINE ( 'NONE', #23081, #27153 ) ;
#38560 = CARTESIAN_POINT ( 'NONE',  ( -14.44809130310161471, -8.473323905341505480, 67.25975083863336579 ) ) ;
#38561 = CARTESIAN_POINT ( 'NONE',  ( -10.29385316490627211, -12.64970523595484231, 64.38340807599202265 ) ) ;
#38562 = LINE ( 'NONE', #42028, #25196 ) ;
#38563 = AXIS2_PLACEMENT_3D ( 'NONE', #6837, #33158, #32689 ) ;
#38564 = ORIENTED_EDGE ( 'NONE', *, *, #23563, .T. ) ;
#38565 = ORIENTED_EDGE ( 'NONE', *, *, #18074, .T. ) ;
#38566 = CARTESIAN_POINT ( 'NONE',  ( -22.33034385650551812, -9.794322478646142471, 51.19202720610083901 ) ) ;
#38567 = EDGE_CURVE ( 'NONE', #26370, #6587, #13701, .T. ) ;
#38568 = CARTESIAN_POINT ( 'NONE',  ( -10.38078070663892483, -14.50222156296672971, 67.85800126083267969 ) ) ;
#38569 = CARTESIAN_POINT ( 'NONE',  ( -16.15640231613377154, -10.29741749701175380, 49.52966884056655772 ) ) ;
#38570 = CARTESIAN_POINT ( 'NONE',  ( -21.62013850256694525, -9.204234574478094899, 70.24205721712547756 ) ) ;
#38571 = ORIENTED_EDGE ( 'NONE', *, *, #48522, .F. ) ;
#38572 = CARTESIAN_POINT ( 'NONE',  ( -13.24284385650551599, -8.811426318492348031, 52.18089403414752070 ) ) ;
#38573 = B_SPLINE_CURVE_WITH_KNOTS ( 'NONE', 3,
 ( #11610, #27357, #11864, #42390, #23192, #8659, #34008, #37700, #45123, #304 ),
 .UNSPECIFIED., .F., .F.,
 ( 4, 2, 2, 2, 4 ),
 ( 0.000000000000000000, 0.2500000000000000000, 0.5000000000000000000, 0.7500000000000000000, 1.000000000000000000 ),
 .UNSPECIFIED. ) ;
#38574 = B_SPLINE_CURVE_WITH_KNOTS ( 'NONE', 3,
 ( #33365, #47934, #7062, #48409, #29221, #41033, #32434, #7315, #22315, #25047 ),
 .UNSPECIFIED., .F., .F.,
 ( 4, 2, 2, 2, 4 ),
 ( 0.000000000000000000, 0.2500000000000000000, 0.5000000000000000000, 0.7500000000000000000, 1.000000000000000000 ),
 .UNSPECIFIED. ) ;
#38575 = ORIENTED_EDGE ( 'NONE', *, *, #14909, .F. ) ;
#38576 = ADVANCED_FACE ( 'NONE', ( #37333 ), #29006, .T. ) ;
#38577 = CARTESIAN_POINT ( 'NONE',  ( -13.60238606012557483, -8.884930320952351579, 56.96967755506135234 ) ) ;
#38578 = CARTESIAN_POINT ( 'NONE',  ( -10.99655737938916289, -18.57624151290433900, 57.99209991576458378 ) ) ;
#38579 = COLOUR_RGB ( '', 0.66274510, 0.83137255, 0.94901961) ;
#38580 = CARTESIAN_POINT ( 'NONE',  ( -24.84793640206982701, -14.18443463346696909, 69.83770693398628282 ) ) ;
#38581 =( BOUNDED_CURVE ( )  B_SPLINE_CURVE ( 3, ( #39526, #5569, #9743, #21056 ),
 .UNSPECIFIED., .F., .F. ) 
 B_SPLINE_CURVE_WITH_KNOTS ( ( 4, 4 ),
 ( 4.712388980384689674, 4.921828490624008623 ),
 .UNSPECIFIED. ) 
 CURVE ( )  GEOMETRIC_REPRESENTATION_ITEM ( )  RATIONAL_B_SPLINE_CURVE ( ( 1.000000000000000000, 0.9963479302455156006, 0.9963479302455156006, 1.000000000000000000 ) ) 
 REPRESENTATION_ITEM ( '' )  );
#38582 = EDGE_CURVE ( 'NONE', #24972, #46199, #11014, .T. ) ;
#38583 = VERTEX_POINT ( 'NONE', #26520 ) ;
#38584 = CARTESIAN_POINT ( 'NONE',  ( -20.72409385541304161, -9.359200813967568422, 50.49621490985803263 ) ) ;
#38585 = CIRCLE ( 'NONE', #11886, 2.500000000000000444 ) ;
#38586 = DIRECTION ( 'NONE',  ( -0.9687793358424819923, 0.2479245821708680464, 0.000000000000000000 ) ) ;
#38587 = CARTESIAN_POINT ( 'NONE',  ( -12.96596534320165972, -9.347742485070138940, 70.84925352874383009 ) ) ;
#38588 = CIRCLE ( 'NONE', #29923, 1.999999999999999556 ) ;
#38589 = ORIENTED_EDGE ( 'NONE', *, *, #31325, .F. ) ;
#38590 = DIRECTION ( 'NONE',  ( 0.7248509490090241369, -0.6889057277456160922, 1.880377065355303572E-09 ) ) ;
#38591 = ADVANCED_FACE ( 'NONE', ( #18137 ), #33152, .T. ) ;
#38592 = CARTESIAN_POINT ( 'NONE',  ( -22.61657813405388495, -16.66287387207217563, 53.88362224778187226 ) ) ;
#38593 = CARTESIAN_POINT ( 'NONE',  ( -11.38992724816770163, -18.36045063709194025, 61.46637994071404165 ) ) ;
#38594 = ORIENTED_EDGE ( 'NONE', *, *, #44869, .F. ) ;
#38595 = CARTESIAN_POINT ( 'NONE',  ( -15.96455646543153151, -7.503521033077919178, 63.86285157243441546 ) ) ;
#38596 = VECTOR ( 'NONE', #39552, 1000.000000000000000 ) ;
#38597 = EDGE_CURVE ( 'NONE', #24799, #35946, #15172, .T. ) ;
#38598 = ORIENTED_EDGE ( 'NONE', *, *, #36287, .T. ) ;
#38599 = CARTESIAN_POINT ( 'NONE',  ( -19.16507141099300782, -7.565355480308949332, 63.60806100508323624 ) ) ;
#38600 = PRODUCT ( 'Cylinder Alignment Washers', 'Cylinder Alignment Washers', '', ( #42005 ) ) ;
#38601 = CARTESIAN_POINT ( 'NONE',  ( -24.74044779172452024, -16.21442189768792375, 62.63682720862403386 ) ) ;
#38602 = VERTEX_POINT ( 'NONE', #29480 ) ;
#38603 = EDGE_CURVE ( 'NONE', #15059, #47792, #29979, .T. ) ;
#38604 = LINE ( 'NONE', #42791, #6930 ) ;
#38605 = CARTESIAN_POINT ( 'NONE',  ( -23.80139577239251736, -11.92276195191408839, 59.78235729430349465 ) ) ;
#38606 = DIRECTION ( 'NONE',  ( -1.616182858256117057E-16, -0.003028072113818697231, 0.9999954153791273948 ) ) ;
#38607 = ORIENTED_EDGE ( 'NONE', *, *, #2829, .T. ) ;
#38608 = DIRECTION ( 'NONE',  ( 0.5562740912439652075, 0.8309988781043535777, 7.851267780903552829E-08 ) ) ;
#38609 = AXIS2_PLACEMENT_3D ( 'NONE', #45750, #12000, #42036 ) ;
#38610 = PRODUCT_DEFINITION_CONTEXT ( 'detailed design', #6119, 'design' ) ;
#38611 = CARTESIAN_POINT ( 'NONE',  ( -15.17234920820390975, -21.91077519426012898, 68.77581698242099151 ) ) ;
#38612 = CARTESIAN_POINT ( 'NONE',  ( -48.17409385541305511, -15.80920654474410725, 61.49999999999999289 ) ) ;
#38613 = CARTESIAN_POINT ( 'NONE',  ( -23.43037763135286156, -19.21690358092465800, 62.54745201246257835 ) ) ;
#38614 = VERTEX_POINT ( 'NONE', #26276 ) ;
#38615 = CARTESIAN_POINT ( 'NONE',  ( -10.61994057853096862, -11.77494598563924733, 74.66501929302266660 ) ) ;
#38616 = DIRECTION ( 'NONE',  ( -0.3688590060343653887, 0.9294853595766531251, 0.000000000000000000 ) ) ;
#38617 = ORIENTED_EDGE ( 'NONE', *, *, #14804, .T. ) ;
#38618 = ORIENTED_EDGE ( 'NONE', *, *, #6779, .F. ) ;
#38619 = CARTESIAN_POINT ( 'NONE',  ( -10.47788155843228708, -15.67630068988790448, 61.33789014617833857 ) ) ;
#38620 = CARTESIAN_POINT ( 'NONE',  ( -19.12409385759799108, -9.359200813967568422, 50.49621490985803263 ) ) ;
#38621 = CARTESIAN_POINT ( 'NONE',  ( -10.42558329592169386, -14.65956671939337319, 71.32782690272046011 ) ) ;
#38622 = CARTESIAN_POINT ( 'NONE',  ( -21.11784385650551954, -9.790100578890868377, 49.79778022625163203 ) ) ;
#38623 = CARTESIAN_POINT ( 'NONE',  ( -23.80338573481879294, -11.80731802715296297, 59.76763678108634537 ) ) ;
#38624 = CARTESIAN_POINT ( 'NONE',  ( -12.26902364965855519, -19.54473725125994221, 57.92682373989410394 ) ) ;
#38625 = CARTESIAN_POINT ( 'NONE',  ( -19.78800712013224583, -21.87439760486632778, 65.62519571951479236 ) ) ;
#38626 = ORIENTED_EDGE ( 'NONE', *, *, #6199, .F. ) ;
#38627 = ORIENTED_EDGE ( 'NONE', *, *, #45144, .T. ) ;
#38629 = CARTESIAN_POINT ( 'NONE',  ( -12.40538999107997498, -20.31523868419091272, 68.52152871938794476 ) ) ;
#38628 = VECTOR ( 'NONE', #34703, 1000.000000000000000 ) ;
#38630 = AXIS2_PLACEMENT_3D ( 'NONE', #8059, #3359, #19114 ) ;
#38631 = CARTESIAN_POINT ( 'NONE',  ( -11.64235247690698749, -18.84330696305777408, 68.51689631558762983 ) ) ;
#38632 = CARTESIAN_POINT ( 'NONE',  ( -19.55442184481404766, -21.52995072282663358, 65.47958309245051112 ) ) ;
#38633 = CARTESIAN_POINT ( 'NONE',  ( -17.79084047922378531, -7.768752242298102573, 60.23060768310389790 ) ) ;
#38634 =( BOUNDED_SURFACE ( )  B_SPLINE_SURFACE ( 3, 1, ( 
 ( #1797, #35996 ),
 ( #10155, #39705 ),
 ( #28858, #21241 ),
 ( #39467, #32329 ),
 ( #47354, #14052 ),
 ( #28139, #47099 ),
 ( #25177, #2750 ) ),
 .UNSPECIFIED., .T., .F., .F. ) 
 B_SPLINE_SURFACE_WITH_KNOTS ( ( 4, 3, 4 ),
 ( 2, 2 ),
 ( 0.000000000000000000, 0.5000000000000000000, 1.000000000000000000 ),
 ( 0.000000000000000000, 1.000000000000000000 ),
 .UNSPECIFIED. ) 
 GEOMETRIC_REPRESENTATION_ITEM ( )  RATIONAL_B_SPLINE_SURFACE ( (
 ( 1.000000000000000000, 1.000000000000000000),
 ( 0.3333333333333335369, 0.3333333333333330373),
 ( 0.3333333333333335369, 0.3333333333333330373),
 ( 1.000000000000000000, 1.000000000000000000),
 ( 0.3333333333333333703, 0.3333333333333333703),
 ( 0.3333333333333333703, 0.3333333333333333703),
 ( 1.000000000000000000, 1.000000000000000000) ) ) 
 REPRESENTATION_ITEM ( '' )  SURFACE ( )  );
#38635 = VECTOR ( 'NONE', #18463, 1000.000000000000000 ) ;
#38636 = ORIENTED_EDGE ( 'NONE', *, *, #14617, .T. ) ;
#38637 = ORIENTED_EDGE ( 'NONE', *, *, #27465, .T. ) ;
#38638 = ADVANCED_FACE ( 'NONE', ( #41290 ), #7575, .T. ) ;
#38639 = LINE ( 'NONE', #26843, #46139 ) ;
#38640 = CARTESIAN_POINT ( 'NONE',  ( -23.63568631841604883, -11.45792465866591137, 73.50626392806049125 ) ) ;
#38641 = DIRECTION ( 'NONE',  ( 3.892913445306193086E-06, 4.639959643356220421E-06, 0.9999999999816580054 ) ) ;
#38642 = CARTESIAN_POINT ( 'NONE',  ( -24.44253391677669285, -17.31023895159264470, 73.06991310009190954 ) ) ;
#38643 = ORIENTED_EDGE ( 'NONE', *, *, #12314, .T. ) ;
#38644 =( BOUNDED_CURVE ( )  B_SPLINE_CURVE ( 3, ( #43893, #21705, #48049, #21948 ),
 .UNSPECIFIED., .F., .F. ) 
 B_SPLINE_CURVE_WITH_KNOTS ( ( 4, 4 ),
 ( 1.570796326794896780, 1.780235837034217283 ),
 .UNSPECIFIED. ) 
 CURVE ( )  GEOMETRIC_REPRESENTATION_ITEM ( )  RATIONAL_B_SPLINE_CURVE ( ( 1.000000000000000000, 0.9963479302455154896, 0.9963479302455154896, 1.000000000000000000 ) ) 
 REPRESENTATION_ITEM ( '' )  );
#38645 = CARTESIAN_POINT ( 'NONE',  ( -24.47853618617655158, -14.58602005854247174, 69.79708117814310242 ) ) ;
#38646 = CARTESIAN_POINT ( 'NONE',  ( -42.18144679658952612, -14.90920654474417972, 64.94117647058821774 ) ) ;
#38647 = VECTOR ( 'NONE', #9426, 1000.000000000000000 ) ;
#38648 = VERTEX_POINT ( 'NONE', #16636 ) ;
#38649 = B_SPLINE_CURVE_WITH_KNOTS ( 'NONE', 3,
 ( #45450, #626, #12193, #45214, #27213, #42238, #8501, #11459, #23530, #35562 ),
 .UNSPECIFIED., .F., .F.,
 ( 4, 2, 2, 2, 4 ),
 ( 0.1272669073658180550, 0.2522669073463211786, 0.3772669073268243300, 0.5022669073073273704, 0.6272669072878305219 ),
 .UNSPECIFIED. ) ;
#38650 = CARTESIAN_POINT ( 'NONE',  ( -17.01690395770326347, -19.47798354061844961, 49.52966884056656482 ) ) ;
#38651 = CARTESIAN_POINT ( 'NONE',  ( -22.17450840124994826, -19.95071447184853497, 65.70421734751553799 ) ) ;
#38652 = VERTEX_POINT ( 'NONE', #12937 ) ;
#38653 = CARTESIAN_POINT ( 'NONE',  ( -10.48085305489969521, -13.91959585118948617, 57.74825035244229809 ) ) ;
#38654 = EDGE_CURVE ( 'NONE', #10403, #20439, #21076, .T. ) ;
#38655 = ORIENTED_EDGE ( 'NONE', *, *, #18209, .F. ) ;
#38656 = CARTESIAN_POINT ( 'NONE',  ( -19.46797834413568040, -22.79580085574647441, 53.49999999999995026 ) ) ;
#38658 = CARTESIAN_POINT ( 'NONE',  ( -24.08907074505709645, -11.48026357735065872, 63.13713704106291402 ) ) ;
#38657 = AXIS2_PLACEMENT_3D ( 'NONE', #19143, #15424, #30731 ) ;
#38659 = ORIENTED_EDGE ( 'NONE', *, *, #46524, .F. ) ;
#38660 = CARTESIAN_POINT ( 'NONE',  ( -12.69763806180496601, -20.04058448603118592, 68.62185382311069759 ) ) ;
#38661 = EDGE_CURVE ( 'NONE', #18548, #4870, #38067, .T. ) ;
#38662 = EDGE_CURVE ( 'NONE', #42753, #14825, #25843, .T. ) ;
#38663 = CARTESIAN_POINT ( 'NONE',  ( -16.22409385541304871, -9.359200813967568422, 50.49621490985801842 ) ) ;
#38664 = CARTESIAN_POINT ( 'NONE',  ( -17.15534385650551741, -7.417179338643134834, 52.18511593390279302 ) ) ;
#38665 = CIRCLE ( 'NONE', #42594, 4.686499999999998778 ) ;
#38666 = CARTESIAN_POINT ( 'NONE',  ( -23.82448057917968143, -18.75384986479144800, 54.02312124697527906 ) ) ;
#38667 = DIRECTION ( 'NONE',  ( 0.000000000000000000, 0.9999954153791273948, 0.003028072113819836077 ) ) ;
#38668 = ORIENTED_EDGE ( 'NONE', *, *, #21062, .F. ) ;
#38669 = CARTESIAN_POINT ( 'NONE',  ( -16.22922801436599727, -7.911814901714118164, 60.20028431044633521 ) ) ;
#38670 = FACE_OUTER_BOUND ( 'NONE', #44241, .T. ) ;
#38671 = FACE_OUTER_BOUND ( 'NONE', #40596, .T. ) ;
#38672 = CARTESIAN_POINT ( 'NONE',  ( -20.56585955126247001, -8.054015989788005925, 66.88829919087760345 ) ) ;
#38673 = CARTESIAN_POINT ( 'NONE',  ( -12.55411140858086760, -19.90724249994213935, 65.15202838036978505 ) ) ;
#38674 = ORIENTED_EDGE ( 'NONE', *, *, #34838, .T. ) ;
#38675 = ORIENTED_EDGE ( 'NONE', *, *, #35231, .F. ) ;
#38676 = CARTESIAN_POINT ( 'NONE',  ( -18.46801905451614090, -7.836623195388690455, 74.12592262855558545 ) ) ;
#38677 = CARTESIAN_POINT ( 'NONE',  ( -22.09234465700630778, -20.09219189623108548, 62.23439162498055310 ) ) ;
#38678 = EDGE_LOOP ( 'NONE', ( #32120, #15326 ) ) ;
#38679 = CARTESIAN_POINT ( 'NONE',  ( -10.00761937521931522, -15.51608998476985946, 57.75288115419267854 ) ) ;
#38680 = AXIS2_PLACEMENT_3D ( 'NONE', #45148, #31078, #81 ) ;
#38681 = FACE_OUTER_BOUND ( 'NONE', #14067, .T. ) ;
#38682 = CARTESIAN_POINT ( 'NONE',  ( -21.71159385759798965, -8.990409506049200417, 49.61344411288074951 ) ) ;
#38683 = PLANE ( 'NONE',  #43105 ) ;
#38684 = CARTESIAN_POINT ( 'NONE',  ( -24.38391064099431915, -14.06024038319858960, 73.42271507915008044 ) ) ;
#38685 = DIRECTION ( 'NONE',  ( 3.652049423109068320E-16, -0.000000000000000000, 1.000000000000000000 ) ) ;
#38686 = CARTESIAN_POINT ( 'NONE',  ( -23.66263630406368534, -11.51900531544784911, 70.30699535439772774 ) ) ;
#38687 = VERTEX_POINT ( 'NONE', #42759 ) ;
#38688 = DIRECTION ( 'NONE',  ( 2.866981220435666553E-17, -1.000000000000000000, -1.190614954331866791E-16 ) ) ;
#38689 = EDGE_CURVE ( 'NONE', #34717, #47795, #18080, .T. ) ;
#38690 = CARTESIAN_POINT ( 'NONE',  ( -19.19444523719849371, -21.63346107625851644, 58.53067200039218676 ) ) ;
#38691 = CARTESIAN_POINT ( 'NONE',  ( -23.21283114448125673, -10.11939864774917908, 63.25681283445349123 ) ) ;
#38692 = CARTESIAN_POINT ( 'NONE',  ( -19.36683724782897897, -21.58655468785150688, 62.00975759738177118 ) ) ;
#38693 = PLANE ( 'NONE',  #958 ) ;
#38694 = ORIENTED_EDGE ( 'NONE', *, *, #11699, .F. ) ;
#38695 = ORIENTED_EDGE ( 'NONE', *, *, #27947, .F. ) ;
#38696 = CARTESIAN_POINT ( 'NONE',  ( -22.35534385650551670, -7.417179338643134834, 52.18511593390279302 ) ) ;
#38697 = VERTEX_POINT ( 'NONE', #38304 ) ;
#38698 = EDGE_CURVE ( 'NONE', #34217, #31055, #16342, .T. ) ;
#38699 = CARTESIAN_POINT ( 'NONE',  ( -11.99234491386792634, -9.710313501827961602, 60.75929282996435887 ) ) ;
#38700 = AXIS2_PLACEMENT_3D ( 'NONE', #44108, #2478, #25133 ) ;
#38701 = EDGE_CURVE ( 'NONE', #5342, #39291, #12226, .T. ) ;
#38702 = DIRECTION ( 'NONE',  ( -0.3739781583979218671, -0.9274375111247652459, -6.296758467538797382E-09 ) ) ;
#38703 = ORIENTED_EDGE ( 'NONE', *, *, #28067, .F. ) ;
#38704 = DIRECTION ( 'NONE',  ( 0.6827297667453423591, 0.7306709694519485376, 5.176517822219623819E-09 ) ) ;
#38705 = PLANE ( 'NONE',  #45368 ) ;
#38706 = ORIENTED_EDGE ( 'NONE', *, *, #38018, .F. ) ;
#38707 = FACE_OUTER_BOUND ( 'NONE', #43592, .T. ) ;
#38708 = DIRECTION ( 'NONE',  ( 8.719004453613161891E-07, -8.513143893533137515E-07, 0.9999999999992574828 ) ) ;
#38709 = ORIENTED_EDGE ( 'NONE', *, *, #16898, .F. ) ;
#38710 = CARTESIAN_POINT ( 'NONE',  ( -11.98246295270348405, -15.60836430055780433, 53.49899999999994549 ) ) ;
#38711 = CARTESIAN_POINT ( 'NONE',  ( -10.12038064680082172, -13.33925369334275324, 74.81671120912561435 ) ) ;
#38712 = VERTEX_POINT ( 'NONE', #4597 ) ;
#38713 = CARTESIAN_POINT ( 'NONE',  ( -23.50857174774670355, -19.10953103619692328, 62.46751498843644157 ) ) ;
#38714 = FACE_OUTER_BOUND ( 'NONE', #38973, .T. ) ;
#38715 = CARTESIAN_POINT ( 'NONE',  ( -18.24909385541303664, -8.112991634885936776, 51.74999426922422430 ) ) ;
#38716 = ORIENTED_EDGE ( 'NONE', *, *, #16016, .F. ) ;
#38717 = CARTESIAN_POINT ( 'NONE',  ( -10.37599212182869124, -14.63324797960940593, 71.34254748307667171 ) ) ;
#38718 = EDGE_CURVE ( 'NONE', #16341, #2752, #16871, .T. ) ;
#38719 = ADVANCED_FACE ( 'NONE', ( #38811 ), #17055, .T. ) ;
#38720 = CARTESIAN_POINT ( 'NONE',  ( -22.17130319910813085, -20.55096425825585982, 58.87947600183965591 ) ) ;
#38721 = CARTESIAN_POINT ( 'NONE',  ( -11.54683828446007254, -10.23068304809853935, 71.12926454345553395 ) ) ;
#38722 = CARTESIAN_POINT ( 'NONE',  ( -36.42409385541304800, -8.109206544743658540, 50.50000000000030553 ) ) ;
#38723 = DIRECTION ( 'NONE',  ( -3.071710424422018668E-17, 6.404604876783312462E-16, 1.000000000000000000 ) ) ;
#38724 = CARTESIAN_POINT ( 'NONE',  ( -12.76954176995949197, -15.35549139150514186, 49.52966884056655772 ) ) ;
#38725 = CARTESIAN_POINT ( 'NONE',  ( -17.59211730330735435, -7.811223398082945302, 63.85057029380297422 ) ) ;
#38726 = DIRECTION ( 'NONE',  ( -1.000000000000000000, -2.866981220435666553E-17, -0.000000000000000000 ) ) ;
#38727 = EDGE_CURVE ( 'NONE', #12198, #26904, #6330, .T. ) ;
#38728 = EDGE_CURVE ( 'NONE', #40177, #41701, #31829, .T. ) ;
#38729 = CARTESIAN_POINT ( 'NONE',  ( -45.92409385541306222, 12.69079345525585545, 69.25000000000000000 ) ) ;
#38730 = CARTESIAN_POINT ( 'NONE',  ( -14.81784385650551705, -9.790100578890868377, 49.79778022625163203 ) ) ;
#38732 = EDGE_CURVE ( 'NONE', #23794, #3957, #40461, .T. ) ;
#38731 = ORIENTED_EDGE ( 'NONE', *, *, #12231, .T. ) ;
#38733 = DIRECTION ( 'NONE',  ( -1.000000000000000000, -2.866981220435666553E-17, 0.000000000000000000 ) ) ;
#38734 = CARTESIAN_POINT ( 'NONE',  ( -10.99586697244644640, -11.04334986774487781, 60.86381167495338929 ) ) ;
#38735 = EDGE_LOOP ( 'NONE', ( #44074, #45789, #13401, #38804 ) ) ;
#38736 = CYLINDRICAL_SURFACE ( 'NONE', #11154, 2.000000000000001776 ) ;
#38737 = CARTESIAN_POINT ( 'NONE',  ( -14.47836531470152188, -7.966228403338186936, 64.04624744032878425 ) ) ;
#38738 = CARTESIAN_POINT ( 'NONE',  ( -19.80301194551662647, -21.44571530912113744, 68.93482476707502826 ) ) ;
#38739 = EDGE_CURVE ( 'NONE', #36187, #24622, #15119, .T. ) ;
#38740 = DIRECTION ( 'NONE',  ( -3.413470714839332458E-33, 1.190614954331866791E-16, -1.000000000000000000 ) ) ;
#38741 = CARTESIAN_POINT ( 'NONE',  ( -18.55957040452605611, -7.446158924837727788, 74.02559677774105751 ) ) ;
#38742 = ORIENTED_EDGE ( 'NONE', *, *, #41580, .F. ) ;
#38743 = FACE_OUTER_BOUND ( 'NONE', #24184, .T. ) ;
#38744 = DIRECTION ( 'NONE',  ( 2.209513395486314832E-06, -7.769005149436063369E-07, -0.9999999999972571940 ) ) ;
#38745 = B_SPLINE_CURVE_WITH_KNOTS ( 'NONE', 3,
 ( #24591, #39585, #5863, #28016, #1920, #20880, #35158, #43779, #46744, #46973 ),
 .UNSPECIFIED., .F., .F.,
 ( 4, 2, 2, 2, 4 ),
 ( 0.000000000000000000, 0.2500000000000000000, 0.5000000000000000000, 0.7500000000000000000, 1.000000000000000000 ),
 .UNSPECIFIED. ) ;
#38746 = CARTESIAN_POINT ( 'NONE',  ( -10.09291391017891115, -16.13494330055838333, 68.16263215882007387 ) ) ;
#38747 = EDGE_CURVE ( 'NONE', #39328, #18995, #43940, .T. ) ;
#38748 = ORIENTED_EDGE ( 'NONE', *, *, #23395, .F. ) ;
#38749 = CARTESIAN_POINT ( 'NONE',  ( -13.27770768808250956, -9.107454094634595876, 63.90946529206384241 ) ) ;
#38750 = DIRECTION ( 'NONE',  ( -0.8201047403141394909, 0.5722134347551369737, 7.883065731424289661E-08 ) ) ;
#38751 = CARTESIAN_POINT ( 'NONE',  ( -24.56285135521319773, -12.67774455940246803, 69.93389527165277286 ) ) ;
#38752 = CARTESIAN_POINT ( 'NONE',  ( -42.41968209070717677, -14.90920654474416907, 63.03529411764704804 ) ) ;
#38753 = DIRECTION ( 'NONE',  ( 0.000000000000000000, 0.000000000000000000, 1.000000000000000000 ) ) ;
#38754 = ORIENTED_EDGE ( 'NONE', *, *, #16884, .T. ) ;
#38755 = ORIENTED_EDGE ( 'NONE', *, *, #31363, .T. ) ;
#38756 = CARTESIAN_POINT ( 'NONE',  ( -20.78034385541304374, -9.360768649639302552, 51.01397948905921709 ) ) ;
#38757 = CARTESIAN_POINT ( 'NONE',  ( -19.92736644894527842, -21.34646251977703102, 72.40478735915066011 ) ) ;
#38758 = VECTOR ( 'NONE', #22806, 1000.000000000000000 ) ;
#38759 = B_SPLINE_CURVE_WITH_KNOTS ( 'NONE', 3,
 ( #38780, #46426, #4817, #11714, #41999, #26742, #41761, #34840, #1340, #30685 ),
 .UNSPECIFIED., .F., .F.,
 ( 4, 2, 2, 2, 4 ),
 ( 0.6272669072877610219, 0.7522669073072782986, 0.8772669073267956863, 1.002266907346313074, 1.127266907365830351 ),
 .UNSPECIFIED. ) ;
#38760 = CARTESIAN_POINT ( 'NONE',  ( -17.46222794319647775, -7.759011850482251837, 67.03511641684839617 ) ) ;
#38761 = CARTESIAN_POINT ( 'NONE',  ( -17.52077441883401576, -21.86154573861348283, 58.82041992746825798 ) ) ;
#38762 = CARTESIAN_POINT ( 'NONE',  ( -20.90753508896134960, -8.676468725517494818, 60.25614029449676678 ) ) ;
#38763 = CARTESIAN_POINT ( 'NONE',  ( -14.13242279744181751, -8.574497162196566435, 74.21426705364891063 ) ) ;
#38764 = CARTESIAN_POINT ( 'NONE',  ( -23.91467064781584995, -17.58181910956628613, 69.55772506159280510 ) ) ;
#38765 =( BOUNDED_CURVE ( )  B_SPLINE_CURVE ( 2, ( #17535, #6224, #47591, #20758, #5508, #17762, #6472, #9690, #9445 ),
 .UNSPECIFIED., .F., .F. ) 
 B_SPLINE_CURVE_WITH_KNOTS ( ( 3, 2, 2, 2, 3 ),
 ( 0.03934058936362840042, 0.04032418838537540212, 0.04130778740712241076, 0.04229138642886941940, 0.04327498545061642110 ),
 .UNSPECIFIED. ) 
 CURVE ( )  GEOMETRIC_REPRESENTATION_ITEM ( )  RATIONAL_B_SPLINE_CURVE ( ( 1.000000000000098144, 0.9238795325111885948, 1.000000000000000000, 0.9238795325112867385, 1.000000000000000000, 0.9238795325112867385, 1.000000000000000000, 0.9238795325114607104, 0.9999999999998260281 ) ) 
 REPRESENTATION_ITEM ( '' )  );
#38766 = EDGE_CURVE ( 'NONE', #16419, #2504, #32468, .T. ) ;
#38767 = EDGE_LOOP ( 'NONE', ( #33973, #35812 ) ) ;
#38768 = CARTESIAN_POINT ( 'NONE',  ( -21.63336539757928634, -9.153348366551478321, 66.94677872351418557 ) ) ;
#38769 = CARTESIAN_POINT ( 'NONE',  ( -16.16828274592561243, -21.75012765010984239, 61.84748396296113526 ) ) ;
#38770 = ORIENTED_EDGE ( 'NONE', *, *, #40964, .T. ) ;
#38771 = CARTESIAN_POINT ( 'NONE',  ( -13.35101845555447042, -21.04725863074550674, 61.62307991559396214 ) ) ;
#38772 = CARTESIAN_POINT ( 'NONE',  ( -23.08487763607990928, -19.01185175973044039, 62.36879011380454330 ) ) ;
#38773 = ORIENTED_EDGE ( 'NONE', *, *, #45555, .T. ) ;
#38774 = LINE ( 'NONE', #390, #6534 ) ;
#38775 = EDGE_CURVE ( 'NONE', #24436, #15477, #19230, .T. ) ;
#38776 = CARTESIAN_POINT ( 'NONE',  ( -11.98712258119491203, -10.32100680013864569, 67.79337086303625881 ) ) ;
#38777 = B_SPLINE_CURVE_WITH_KNOTS ( 'NONE', 3,
 ( #44614, #33251, #8169, #19235, #30339, #10870, #11122, #45347, #38172, #11601 ),
 .UNSPECIFIED., .F., .F.,
 ( 4, 2, 2, 2, 4 ),
 ( 0.6272669072783292332, 0.7522669073002161699, 0.8772669073221032177, 1.002266907343990265, 1.127266907365877202 ),
 .UNSPECIFIED. ) ;
#38778 =( BOUNDED_CURVE ( )  B_SPLINE_CURVE ( 3, ( #16963, #28324, #5680, #36165 ),
 .UNSPECIFIED., .F., .F. ) 
 B_SPLINE_CURVE_WITH_KNOTS ( ( 4, 4 ),
 ( 0.000000000000000000, 0.4074455897393680637 ),
 .UNSPECIFIED. ) 
 CURVE ( )  GEOMETRIC_REPRESENTATION_ITEM ( )  RATIONAL_B_SPLINE_CURVE ( ( 1.000000000000000000, 0.4567392136813319126, 0.3561768502900302669, 0.6983129098260951739 ) ) 
 REPRESENTATION_ITEM ( '' )  );
#38779 = DIRECTION ( 'NONE',  ( 0.000000000000000000, 1.000000000000000000, 3.469446951953614189E-15 ) ) ;
#38780 = CARTESIAN_POINT ( 'NONE',  ( -24.48810908846319734, -17.17637088580320537, 73.06831457992643664 ) ) ;
#38781 = ORIENTED_EDGE ( 'NONE', *, *, #15368, .T. ) ;
#38782 = FACE_OUTER_BOUND ( 'NONE', #34114, .T. ) ;
#38783 = DIRECTION ( 'NONE',  ( 2.696738943264045022E-06, 1.002714486673431828E-05, 0.9999999999460920108 ) ) ;
#38784 =( BOUNDED_CURVE ( )  B_SPLINE_CURVE ( 3, ( #23034, #38019, #34817, #42217 ),
 .UNSPECIFIED., .F., .F. ) 
 B_SPLINE_CURVE_WITH_KNOTS ( ( 4, 4 ),
 ( 0.000000000000000000, 0.4074455897393673975 ),
 .UNSPECIFIED. ) 
 CURVE ( )  GEOMETRIC_REPRESENTATION_ITEM ( )  RATIONAL_B_SPLINE_CURVE ( ( 1.000000000000000000, 0.4567392136813303027, 0.3561768502900297118, 0.6983129098260982826 ) ) 
 REPRESENTATION_ITEM ( '' )  );
#38785 = CARTESIAN_POINT ( 'NONE',  ( -10.88594323032443967, -11.23743189042336788, 64.28735501138554298 ) ) ;
#38786 = DIRECTION ( 'NONE',  ( -0.5729733056696844073, 0.8195740302071246042, 7.403245352187747277E-08 ) ) ;
#38787 = PRODUCT_CONTEXT ( 'NONE', #5489, 'mechanical' ) ;
#38788 = CARTESIAN_POINT ( 'NONE',  ( -10.78031428196279329, -11.32923628920978310, 54.27966884056655061 ) ) ;
#38789 = CARTESIAN_POINT ( 'NONE',  ( -17.36015951656348832, -7.359395083792595216, 67.20534920880687935 ) ) ;
#38790 = CIRCLE ( 'NONE', #30935, 1.999999999999998446 ) ;
#38791 = EDGE_CURVE ( 'NONE', #31554, #29013, #27140, .T. ) ;
#38792 = DIRECTION ( 'NONE',  ( 1.000000000000000000, -4.164305804376849172E-17, 1.614929280266638808E-16 ) ) ;
#38793 = ORIENTED_EDGE ( 'NONE', *, *, #12337, .F. ) ;
#38794 = CARTESIAN_POINT ( 'NONE',  ( -43.04835856129541583, -14.80920654474410547, 58.00588235294116402 ) ) ;
#38795 = EDGE_CURVE ( 'NONE', #44533, #5874, #31631, .T. ) ;
#38796 = ORIENTED_EDGE ( 'NONE', *, *, #18486, .F. ) ;
#38797 = CARTESIAN_POINT ( 'NONE',  ( -11.15030165360094117, -11.70430893863018262, 67.84537925602023734 ) ) ;
#38798 = CARTESIAN_POINT ( 'NONE',  ( -13.21199625013959178, -9.217751934154737370, 67.66326273853178463 ) ) ;
#38799 = VERTEX_POINT ( 'NONE', #39295 ) ;
#38800 = LINE ( 'NONE', #5317, #13773 ) ;
#38801 =( BOUNDED_CURVE ( )  B_SPLINE_CURVE ( 3, ( #26426, #42429, #34784, #45162 ),
 .UNSPECIFIED., .F., .F. ) 
 B_SPLINE_CURVE_WITH_KNOTS ( ( 4, 4 ),
 ( 0.9074455897393678416, 1.000000000000000000 ),
 .UNSPECIFIED. ) 
 CURVE ( )  GEOMETRIC_REPRESENTATION_ITEM ( )  RATIONAL_B_SPLINE_CURVE ( ( 0.6983129098261183776, 0.7760317562607200736, 0.8765941196520139478, 1.000000000000000000 ) ) 
 REPRESENTATION_ITEM ( '' )  );
#38802 = FACE_BOUND ( 'NONE', #4900, .T. ) ;
#38803 = ORIENTED_EDGE ( 'NONE', *, *, #21210, .F. ) ;
#38804 = ORIENTED_EDGE ( 'NONE', *, *, #46680, .T. ) ;
#38805 = VERTEX_POINT ( 'NONE', #32158 ) ;
#38806 = CARTESIAN_POINT ( 'NONE',  ( -17.98424483515344718, -22.23819686138322638, 61.91890007431585019 ) ) ;
#38807 = CARTESIAN_POINT ( 'NONE',  ( -21.73659385541302314, -8.995762431863237651, 51.38120296130587406 ) ) ;
#38809 = EDGE_CURVE ( 'NONE', #32553, #23509, #18509, .T. ) ;
#38808 = CARTESIAN_POINT ( 'NONE',  ( -13.44265069500541898, -7.318461398084003200, 54.49999999999995026 ) ) ;
#38810 = CARTESIAN_POINT ( 'NONE',  ( -14.48363557501458132, -8.456628546212041186, 67.55975083097567335 ) ) ;
#38811 = FACE_OUTER_BOUND ( 'NONE', #37839, .T. ) ;
#38812 = DIRECTION ( 'NONE',  ( -3.071710424422018668E-17, 6.404604876783312462E-16, 1.000000000000000000 ) ) ;
#38813 = EDGE_LOOP ( 'NONE', ( #902, #36415, #36921, #12125, #6190 ) ) ;
#38814 = ORIENTED_EDGE ( 'NONE', *, *, #38998, .F. ) ;
#38815 = CARTESIAN_POINT ( 'NONE',  ( -20.69909385650551670, -8.114302828567740988, 52.18300498402516041 ) ) ;
#38816 = PRODUCT_RELATED_PRODUCT_CATEGORY ( 'part', '', ( #859 ) ) ;
#38817 = CARTESIAN_POINT ( 'NONE',  ( -17.70776835051902864, -22.25388969026799657, 58.52057945155585372 ) ) ;
#38818 = DIRECTION ( 'NONE',  ( 4.116680954457742276E-07, 3.835121109574216710E-07, 0.9999999999998415712 ) ) ;
#38819 = CARTESIAN_POINT ( 'NONE',  ( -21.53009296270428052, -9.139787401108153020, 70.43132584625033132 ) ) ;
#38820 = ORIENTED_EDGE ( 'NONE', *, *, #27753, .F. ) ;
#38821 = CARTESIAN_POINT ( 'NONE',  ( -20.92409385650551812, -6.426201560718813433, 50.50509628382439331 ) ) ;
#38822 = VERTEX_POINT ( 'NONE', #33510 ) ;
#38823 = LINE ( 'NONE', #39549, #6023 ) ;
#38824 = CARTESIAN_POINT ( 'NONE',  ( -19.06702665442182365, -7.953160677532423506, 63.72529421800381044 ) ) ;
#38825 = AXIS2_PLACEMENT_3D ( 'NONE', #23899, #13919, #5179 ) ;
#38826 = FACE_OUTER_BOUND ( 'NONE', #30702, .T. ) ;
#38827 = ADVANCED_FACE ( 'NONE', ( #6957 ), #32176, .T. ) ;
#38828 = ORIENTED_EDGE ( 'NONE', *, *, #16130, .F. ) ;
#38829 = CARTESIAN_POINT ( 'NONE',  ( -18.53556552080321751, -22.17591605216722428, 72.40015545304112266 ) ) ;
#38830 = CARTESIAN_POINT ( 'NONE',  ( -21.52726260838264949, -9.076274878514674072, 70.13132538915753855 ) ) ;
#38831 = CARTESIAN_POINT ( 'NONE',  ( -22.07021550121272568, -8.985394110722673133, 63.29815443424653409 ) ) ;
#38832 = CARTESIAN_POINT ( 'NONE',  ( -17.42409385541299471, -14.80920654474435594, 52.02966884056656482 ) ) ;
#38833 = VERTEX_POINT ( 'NONE', #48309 ) ;
#38834 = CARTESIAN_POINT ( 'NONE',  ( -16.19814381282456495, -21.75179583453235210, 58.58585572026735377 ) ) ;
#38835 = CARTESIAN_POINT ( 'NONE',  ( -17.33262245845742910, -7.759502110702281463, 67.30567542699309058 ) ) ;
#38836 = CARTESIAN_POINT ( 'NONE',  ( -20.11638923031699022, -7.862561834400525029, 73.84283875516227624 ) ) ;
#38837 = ORIENTED_EDGE ( 'NONE', *, *, #29269, .F. ) ;
#38838 = DIRECTION ( 'NONE',  ( -7.652304188939491606E-06, -2.165757507092278517E-06, -0.9999999999683759633 ) ) ;
#38839 = VERTEX_POINT ( 'NONE', #42990 ) ;
#38840 = CARTESIAN_POINT ( 'NONE',  ( -9.974591638057805909, -14.71890188683600087, 71.43444401210939532 ) ) ;
#38841 = PLANE ( 'NONE',  #45329 ) ;
#38842 = VERTEX_POINT ( 'NONE', #23438 ) ;
#38843 = CARTESIAN_POINT ( 'NONE',  ( -20.32907747881911575, -11.13165948213017131, 49.52966884056655772 ) ) ;
#38844 = CARTESIAN_POINT ( 'NONE',  ( -24.64686309199095859, -12.98257247058134212, 62.97117624809372671 ) ) ;
#38845 = CYLINDRICAL_SURFACE ( 'NONE', #27325, 5.249999999999998224 ) ;
#38846 = EDGE_CURVE ( 'NONE', #21817, #20066, #15286, .T. ) ;
#38847 = CARTESIAN_POINT ( 'NONE',  ( -17.81160558974998764, -14.71003671187603956, 2.029618040566568027 ) ) ;
#38848 = ORIENTED_EDGE ( 'NONE', *, *, #34713, .T. ) ;
#38849 = CARTESIAN_POINT ( 'NONE',  ( -23.71561414012218094, -17.99693426085591952, 59.41867086777731544 ) ) ;
#38850 = EDGE_CURVE ( 'NONE', #44349, #35620, #42058, .T. ) ;
#38851 = CARTESIAN_POINT ( 'NONE',  ( -20.75714322117456945, -21.47287265741918461, 58.83130466214971221 ) ) ;
#38852 = DIRECTION ( 'NONE',  ( -3.071710424422018668E-17, 6.404604876783312462E-16, 1.000000000000000000 ) ) ;
#38853 = CARTESIAN_POINT ( 'NONE',  ( -17.77921064978749044, -22.25082400685520057, 58.59048811498988840 ) ) ;
#38854 = ORIENTED_EDGE ( 'NONE', *, *, #33815, .F. ) ;
#38855 = B_SPLINE_CURVE_WITH_KNOTS ( 'NONE', 1,
 ( #1653, #46230 ),
 .UNSPECIFIED., .F., .F.,
 ( 2, 2 ),
 ( 0.000000000000000000, 1.000000000000000000 ),
 .UNSPECIFIED. ) ;
#38856 = CARTESIAN_POINT ( 'NONE',  ( -15.82103535061131261, -7.533639916251397395, 67.39653228388428374 ) ) ;
#38857 = AXIS2_PLACEMENT_3D ( 'NONE', #39716, #42697, #46135 ) ;
#38858 = B_SPLINE_CURVE_WITH_KNOTS ( 'NONE', 1,
 ( #35242, #5474 ),
 .UNSPECIFIED., .F., .F.,
 ( 2, 2 ),
 ( 0.000000000000000000, 1.000000000000000000 ),
 .UNSPECIFIED. ) ;
#38859 = EDGE_CURVE ( 'NONE', #12742, #31052, #4003, .T. ) ;
#38860 = CARTESIAN_POINT ( 'NONE',  ( -29.92409385541305156, -6.859206544744110623, 63.99999999999998579 ) ) ;
#38861 = CIRCLE ( 'NONE', #5058, 1.250000000000001998 ) ;
#38862 = ORIENTED_EDGE ( 'NONE', *, *, #48243, .F. ) ;
#38863 = ORIENTED_EDGE ( 'NONE', *, *, #37955, .T. ) ;
#38864 = CARTESIAN_POINT ( 'NONE',  ( -21.23484681875272528, -20.74088929683185611, 69.33978048267414351 ) ) ;
#38865 = CARTESIAN_POINT ( 'NONE',  ( -10.99655682251556144, -18.57624055219563175, 57.99209882808910521 ) ) ;
#38866 = EDGE_CURVE ( 'NONE', #14458, #17537, #22967, .T. ) ;
#38867 = CARTESIAN_POINT ( 'NONE',  ( -21.39909385650551599, -8.114302828567740988, 52.18300498402516041 ) ) ;
#38868 = CARTESIAN_POINT ( 'NONE',  ( -12.41953831520651264, -9.914705408137539422, 57.38935537466883119 ) ) ;
#38869 = EDGE_CURVE ( 'NONE', #31039, #16383, #35702, .T. ) ;
#38870 = CARTESIAN_POINT ( 'NONE',  ( -24.72409385541305582, -14.90920654474426321, 72.08823529411763786 ) ) ;
#38871 = CARTESIAN_POINT ( 'NONE',  ( -18.63018970549565978, -7.457396494496333794, 73.95569010969242640 ) ) ;
#38872 = ORIENTED_EDGE ( 'NONE', *, *, #40941, .F. ) ;
#38873 = EDGE_LOOP ( 'NONE', ( #41375, #14319, #29474, #17826, #28590 ) ) ;
#38874 = CARTESIAN_POINT ( 'NONE',  ( -12.35909018435058471, -20.27262818183478998, 68.52995730439641875 ) ) ;
#38875 = CARTESIAN_POINT ( 'NONE',  ( -16.06904075904983031, -7.890656793283916670, 63.97011029956861705 ) ) ;
#38876 = B_SPLINE_CURVE_WITH_KNOTS ( 'NONE', 3,
 ( #46574, #39412, #9633, #20941, #5694, #13529, #24649, #20703, #1978, #31540 ),
 .UNSPECIFIED., .F., .F.,
 ( 4, 2, 2, 2, 4 ),
 ( 0.000000000000000000, 0.2500000000000000000, 0.5000000000000000000, 0.7500000000000000000, 1.000000000000000000 ),
 .UNSPECIFIED. ) ;
#38877 = DIRECTION ( 'NONE',  ( 3.071710424422018668E-17, -6.404604876783312462E-16, -1.000000000000000000 ) ) ;
#38878 =( BOUNDED_SURFACE ( )  B_SPLINE_SURFACE ( 3, 1, ( 
 ( #8678, #42161 ),
 ( #552, #4483 ),
 ( #38197, #1039 ),
 ( #7961, #5218 ),
 ( #16033, #31074 ),
 ( #26907, #34998 ),
 ( #41917, #45864 ) ),
 .UNSPECIFIED., .T., .F., .F. ) 
 B_SPLINE_SURFACE_WITH_KNOTS ( ( 4, 3, 4 ),
 ( 2, 2 ),
 ( 0.000000000000000000, 0.5000000000000000000, 1.000000000000000000 ),
 ( 0.000000000000000000, 1.000000000000000000 ),
 .UNSPECIFIED. ) 
 GEOMETRIC_REPRESENTATION_ITEM ( )  RATIONAL_B_SPLINE_SURFACE ( (
 ( 1.000000000000000000, 1.000000000000000000),
 ( 0.3333333333333335369, 0.3333333333333330373),
 ( 0.3333333333333335369, 0.3333333333333330373),
 ( 1.000000000000000000, 1.000000000000000000),
 ( 0.3333333333333333703, 0.3333333333333333703),
 ( 0.3333333333333333703, 0.3333333333333333703),
 ( 1.000000000000000000, 1.000000000000000000) ) ) 
 REPRESENTATION_ITEM ( '' )  SURFACE ( )  );
#38879 = CARTESIAN_POINT ( 'NONE',  ( -18.92901792560347829, -7.918630368440815026, 70.78556921992733919 ) ) ;
#38880 = EDGE_CURVE ( 'NONE', #42696, #37693, #64, .T. ) ;
#38881 = ORIENTED_EDGE ( 'NONE', *, *, #15687, .F. ) ;
#38882 = CARTESIAN_POINT ( 'NONE',  ( -15.05422094890265683, -21.39590065587122325, 61.70888574689368511 ) ) ;
#38883 = LINE ( 'NONE', #9100, #8771 ) ;
#38884 = CARTESIAN_POINT ( 'NONE',  ( -22.17374636168253943, -9.068608547125135644, 63.37809084343794552 ) ) ;
#38885 = DIRECTION ( 'NONE',  ( -3.071710424422018668E-17, 6.404604876783312462E-16, 1.000000000000000000 ) ) ;
#38886 = EDGE_CURVE ( 'NONE', #32391, #20038, #13882, .T. ) ;
#38887 = ORIENTED_EDGE ( 'NONE', *, *, #32046, .T. ) ;
#38888 = VECTOR ( 'NONE', #26899, 1000.000000000000000 ) ;
#38889 = FACE_OUTER_BOUND ( 'NONE', #25152, .T. ) ;
#38890 = VECTOR ( 'NONE', #16727, 1000.000000000000000 ) ;
#38891 = VERTEX_POINT ( 'NONE', #42152 ) ;
#38892 = CARTESIAN_POINT ( 'NONE',  ( -11.42587710518540334, -11.10406226247761019, 57.49431069621225276 ) ) ;
#38893 = CARTESIAN_POINT ( 'NONE',  ( -16.16748626245079379, -22.20318634978239203, 54.27966884056655061 ) ) ;
#38894 = EDGE_LOOP ( 'NONE', ( #25212, #5082, #45627, #2362 ) ) ;
#38895 = EDGE_CURVE ( 'NONE', #17121, #10137, #4592, .T. ) ;
#38896 = CARTESIAN_POINT ( 'NONE',  ( -13.14320010650797776, -9.203067583597343670, 71.14925540519338654 ) ) ;
#38897 = EDGE_LOOP ( 'NONE', ( #17507, #8842, #1777, #27802, #4305 ) ) ;
#38898 = DIRECTION ( 'NONE',  ( -0.4749924142254752235, -0.8799898899579782219, -8.916637576350563827E-09 ) ) ;
#38899 = CARTESIAN_POINT ( 'NONE',  ( -18.57335281209669375, -21.76520412651811043, 72.57038810541313012 ) ) ;
#38900 = VERTEX_POINT ( 'NONE', #15291 ) ;
#38901 = CARTESIAN_POINT ( 'NONE',  ( -18.10946867608448940, -21.82882885753907942, 69.23003497527133732 ) ) ;
#38902 = CARTESIAN_POINT ( 'NONE',  ( -15.63659385650551670, -6.915538690918075382, 49.31353937987644542 ) ) ;
#38903 = ORIENTED_EDGE ( 'NONE', *, *, #19631, .T. ) ;
#38904 = CARTESIAN_POINT ( 'NONE',  ( -24.42872760227104578, -14.00939437836273349, 73.41711714289721158 ) ) ;
#38905 = CARTESIAN_POINT ( 'NONE',  ( -14.65746096889331263, -8.316078616448901784, 57.00567256703398300 ) ) ;
#38906 = DIRECTION ( 'NONE',  ( -0.8604039311673230550, -0.5096126717731922495, 7.110477544621476444E-08 ) ) ;
#38907 = VERTEX_POINT ( 'NONE', #45365 ) ;
#38908 = CARTESIAN_POINT ( 'NONE',  ( -17.42409385541299471, -14.80920654474434883, 62.02966884056656482 ) ) ;
#38909 = CARTESIAN_POINT ( 'NONE',  ( -11.77169895589660342, -10.59578386207264700, 74.43885051664024388 ) ) ;
#38910 = B_SPLINE_CURVE_WITH_KNOTS ( 'NONE', 1,
 ( #8767, #24026 ),
 .UNSPECIFIED., .F., .F.,
 ( 2, 2 ),
 ( 0.000000000000000000, 1.000000000000000000 ),
 .UNSPECIFIED. ) ;
#38911 = EDGE_CURVE ( 'NONE', #7864, #31485, #30898, .T. ) ;
#38912 = CARTESIAN_POINT ( 'NONE',  ( -24.61402911129809112, -12.85776555077031880, 66.40972601524751440 ) ) ;
#38913 = CARTESIAN_POINT ( 'NONE',  ( -15.09544305450467938, -21.46351983957133669, 65.40596681500470311 ) ) ;
#38914 = ORIENTED_EDGE ( 'NONE', *, *, #45976, .T. ) ;
#38915 = ORIENTED_EDGE ( 'NONE', *, *, #13741, .T. ) ;
#38916 = EDGE_CURVE ( 'NONE', #34444, #29137, #21596, .T. ) ;
#38917 = CARTESIAN_POINT ( 'NONE',  ( -18.62860737289870983, -7.457144689169211027, 74.09710349057253609 ) ) ;
#38918 = CARTESIAN_POINT ( 'NONE',  ( -14.60479746972646886, -7.913168098764732150, 60.50491608655884335 ) ) ;
#38919 = ORIENTED_EDGE ( 'NONE', *, *, #8190, .F. ) ;
#38920 = CARTESIAN_POINT ( 'NONE',  ( -15.75439910800316845, -7.548642891367095764, 67.18361323375314953 ) ) ;
#38921 = CARTESIAN_POINT ( 'NONE',  ( -10.68551981713787136, -12.73596763222149164, 64.28308208171728211 ) ) ;
#38922 = CARTESIAN_POINT ( 'NONE',  ( -21.82409385759798681, -9.359200813967568422, 50.49621490985803263 ) ) ;
#38923 = CARTESIAN_POINT ( 'NONE',  ( -18.85724798917316392, -7.906108138700305155, 67.18599644112759961 ) ) ;
#38924 =( BOUNDED_CURVE ( )  B_SPLINE_CURVE ( 3, ( #33015, #11363, #41157, #33495 ),
 .UNSPECIFIED., .F., .F. ) 
 B_SPLINE_CURVE_WITH_KNOTS ( ( 4, 4 ),
 ( 0.9074455897393701731, 1.000000000000000000 ),
 .UNSPECIFIED. ) 
 CURVE ( )  GEOMETRIC_REPRESENTATION_ITEM ( )  RATIONAL_B_SPLINE_CURVE ( ( 0.6983129098261113832, 0.7760317562607140784, 0.8765941196520102840, 1.000000000000000000 ) ) 
 REPRESENTATION_ITEM ( '' )  );
#38925 = CARTESIAN_POINT ( 'NONE',  ( -10.95917937052863245, -17.62195967018737264, 71.58190244267143498 ) ) ;
#38926 = CARTESIAN_POINT ( 'NONE',  ( -41.55277032600130127, -14.90920654474423124, 69.97058823529410176 ) ) ;
#38927 = AXIS2_PLACEMENT_3D ( 'NONE', #24539, #17595, #20593 ) ;
#38928 = VERTEX_POINT ( 'NONE', #7953 ) ;
#38929 = CARTESIAN_POINT ( 'NONE',  ( -22.63674339536608926, -20.13198319316658313, 69.43063894133570102 ) ) ;
#38930 = CIRCLE ( 'NONE', #9064, 2.000000000000001776 ) ;
#38931 = DIRECTION ( 'NONE',  ( -3.071710424422018668E-17, 6.404604876783312462E-16, 1.000000000000000000 ) ) ;
#38932 = CARTESIAN_POINT ( 'NONE',  ( -22.71334156758821265, -10.13600392596141475, 63.22752948238618842 ) ) ;
#38933 = CARTESIAN_POINT ( 'NONE',  ( -26.80819156775448420, -19.72453833035618942, 53.49999999999995026 ) ) ;
#38934 = CARTESIAN_POINT ( 'NONE',  ( -21.46445858442271870, -9.092811667914396878, 70.43132491394226236 ) ) ;
#38935 = EDGE_CURVE ( 'NONE', #39661, #18572, #14159, .T. ) ;
#38936 =( BOUNDED_SURFACE ( )  B_SPLINE_SURFACE ( 3, 1, ( 
 ( #14866, #41244 ),
 ( #33847, #144 ),
 ( #43994, #10250 ),
 ( #25263, #40282 ),
 ( #6549, #4082 ),
 ( #861, #30669 ),
 ( #5042, #12182 ) ),
 .UNSPECIFIED., .T., .F., .F. ) 
 B_SPLINE_SURFACE_WITH_KNOTS ( ( 4, 3, 4 ),
 ( 2, 2 ),
 ( 0.000000000000000000, 0.5000000000000000000, 1.000000000000000000 ),
 ( 0.000000000000000000, 1.000000000000000000 ),
 .UNSPECIFIED. ) 
 GEOMETRIC_REPRESENTATION_ITEM ( )  RATIONAL_B_SPLINE_SURFACE ( (
 ( 1.000000000000000000, 1.000000000000000000),
 ( 0.3333333333333335369, 0.3333333333333330373),
 ( 0.3333333333333335369, 0.3333333333333330373),
 ( 1.000000000000000000, 1.000000000000000000),
 ( 0.3333333333333333703, 0.3333333333333333703),
 ( 0.3333333333333333703, 0.3333333333333333703),
 ( 1.000000000000000000, 1.000000000000000000) ) ) 
 REPRESENTATION_ITEM ( '' )  SURFACE ( )  );
#38938 = ORIENTED_EDGE ( 'NONE', *, *, #24802, .T. ) ;
#38937 = EDGE_CURVE ( 'NONE', #8715, #11147, #38103, .T. ) ;
#38939 = ORIENTED_EDGE ( 'NONE', *, *, #23618, .F. ) ;
#38940 = VERTEX_POINT ( 'NONE', #12107 ) ;
#38941 = EDGE_CURVE ( 'NONE', #14012, #6698, #1965, .T. ) ;
#38942 = EDGE_CURVE ( 'NONE', #16853, #24862, #12322, .T. ) ;
#38943 = CARTESIAN_POINT ( 'NONE',  ( -11.00375763999895007, -18.58866327377100447, 57.96747934402117153 ) ) ;
#38944 = ORIENTED_EDGE ( 'NONE', *, *, #42062, .F. ) ;
#38945 = CARTESIAN_POINT ( 'NONE',  ( -21.52107272639815960, -9.068161724387254097, 66.54661176836198422 ) ) ;
#38946 = DIRECTION ( 'NONE',  ( -8.478320030308545538E-07, 8.009068449373887445E-06, -0.9999999999675679430 ) ) ;
#38947 = VERTEX_POINT ( 'NONE', #5213 ) ;
#38948 = CARTESIAN_POINT ( 'NONE',  ( -23.13707066727631556, -18.94018274121504319, 62.65406854393442160 ) ) ;
#38949 = CARTESIAN_POINT ( 'NONE',  ( -19.03984369153074141, -21.67464089235836511, 58.93996235972087305 ) ) ;
#38950 = EDGE_LOOP ( 'NONE', ( #8, #7610, #47067, #25501, #2868 ) ) ;
#38951 = CARTESIAN_POINT ( 'NONE',  ( -16.78411497196904278, -21.83009869597352903, 68.69560651670111895 ) ) ;
#38952 = DIRECTION ( 'NONE',  ( -0.003782665018460030538, -0.9999928456970870183, -9.532993539451315208E-09 ) ) ;
#38953 = AXIS2_PLACEMENT_3D ( 'NONE', #8415, #41412, #19255 ) ;
#38954 = VERTEX_POINT ( 'NONE', #39423 ) ;
#38955 = DIRECTION ( 'NONE',  ( -3.071710424422018668E-17, 6.404604876783312462E-16, 1.000000000000000000 ) ) ;
#38956 = FACE_OUTER_BOUND ( 'NONE', #422, .T. ) ;
#38957 = FACE_OUTER_BOUND ( 'NONE', #9827, .T. ) ;
#38958 = VERTEX_POINT ( 'NONE', #35703 ) ;
#38959 = CARTESIAN_POINT ( 'NONE',  ( -24.26156011361375420, -17.76763406014958591, 62.58022692647417529 ) ) ;
#38960 = EDGE_CURVE ( 'NONE', #23831, #828, #37469, .T. ) ;
#38961 = CARTESIAN_POINT ( 'NONE',  ( -14.64754011156049174, -7.895932636330921461, 60.52007478328511780 ) ) ;
#38962 = CARTESIAN_POINT ( 'NONE',  ( -24.09941705946771862, -11.50122934708656608, 63.05194655968659845 ) ) ;
#38963 = B_SPLINE_CURVE_WITH_KNOTS ( 'NONE', 3,
 ( #4058, #41458, #22507, #37019, #11191, #7506, #40726, #38001, #41217, #37257 ),
 .UNSPECIFIED., .F., .F.,
 ( 4, 2, 2, 2, 4 ),
 ( 0.6272669072877513630, 0.7522669073072626444, 0.8772669073267738149, 1.002266907346285096, 1.127266907365796378 ),
 .UNSPECIFIED. ) ;
#38964 = CARTESIAN_POINT ( 'NONE',  ( -14.53471675559079834, -21.67622060161817643, 58.28900965065733430 ) ) ;
#38965 = LINE ( 'NONE', #9904, #32375 ) ;
#38966 = CARTESIAN_POINT ( 'NONE',  ( -19.24947176484442224, -8.051269630034916247, 59.96092964444785167 ) ) ;
#38967 = EDGE_LOOP ( 'NONE', ( #39827, #34270, #43574, #47732, #21971 ) ) ;
#38968 = CARTESIAN_POINT ( 'NONE',  ( -24.40947378145952129, -13.83047763063617630, 73.33091373203986052 ) ) ;
#38969 = CARTESIAN_POINT ( 'NONE',  ( -22.78190067944302299, -10.22696095015725604, 66.84182243026252479 ) ) ;
#38970 = CARTESIAN_POINT ( 'NONE',  ( -23.34288396506439867, -19.33377296368179543, 59.06906041190286771 ) ) ;
#38971 = CARTESIAN_POINT ( 'NONE',  ( -14.20982565386415963, -21.02760505633974120, 72.03493667776581333 ) ) ;
#38972 = CARTESIAN_POINT ( 'NONE',  ( -15.54909385650551634, -8.104110260919579645, 48.81699501597546487 ) ) ;
#38973 = EDGE_LOOP ( 'NONE', ( #11510, #14583, #37289, #4831, #36765 ) ) ;
#38974 = EDGE_CURVE ( 'NONE', #3630, #29446, #42650, .T. ) ;
#38975 = CARTESIAN_POINT ( 'NONE',  ( -10.42822707016751416, -13.93690136499678900, 57.74825009391801700 ) ) ;
#38976 = CARTESIAN_POINT ( 'NONE',  ( -10.81170448216924740, -12.36318809540519048, 57.34329390664808557 ) ) ;
#38977 = ORIENTED_EDGE ( 'NONE', *, *, #45154, .F. ) ;
#38978 = DIRECTION ( 'NONE',  ( -3.071710424422018668E-17, 6.404604876783312462E-16, 1.000000000000000000 ) ) ;
#38979 = CARTESIAN_POINT ( 'NONE',  ( -12.18170095131842068, -10.17053037870675780, 64.02914326641410980 ) ) ;
#38980 = CARTESIAN_POINT ( 'NONE',  ( -17.90041350441808632, -22.24413145357778987, 62.03682421940214908 ) ) ;
#38981 = CARTESIAN_POINT ( 'NONE',  ( -24.46479344177693349, -14.44719919422189491, 66.18292729247950490 ) ) ;
#38982 = CARTESIAN_POINT ( 'NONE',  ( -13.07932274695846964, -16.56597809083076100, 49.52966884056655772 ) ) ;
#38983 = ORIENTED_EDGE ( 'NONE', *, *, #31958, .F. ) ;
#38984 = CYLINDRICAL_SURFACE ( 'NONE', #38857, 1.249999999999998668 ) ;
#38985 = DIRECTION ( 'NONE',  ( -0.1648596854219665231, -0.9863170302304251624, 7.074492695208254125E-08 ) ) ;
#38986 = CARTESIAN_POINT ( 'NONE',  ( -12.23301264461619553, -10.03852782535897958, 60.84446034103241630 ) ) ;
#38987 = ORIENTED_EDGE ( 'NONE', *, *, #18074, .F. ) ;
#38988 = CARTESIAN_POINT ( 'NONE',  ( -18.54404894011023686, -22.17459442116309631, 72.47849261052394354 ) ) ;
#38989 = B_SPLINE_CURVE_WITH_KNOTS ( 'NONE', 1,
 ( #41988, #22294 ),
 .UNSPECIFIED., .F., .F.,
 ( 2, 2 ),
 ( 0.000000000000000000, 1.000000000000000000 ),
 .UNSPECIFIED. ) ;
#38990 = CARTESIAN_POINT ( 'NONE',  ( -10.42255780831017553, -12.26328212591781686, 57.52195625194215012 ) ) ;
#38991 = CARTESIAN_POINT ( 'NONE',  ( -12.58019717620059197, -16.04882945559874585, 53.27966884056655061 ) ) ;
#38992 = CARTESIAN_POINT ( 'NONE',  ( -13.73970650151387751, -20.76112128469266693, 64.98628881673506896 ) ) ;
#38993 = CARTESIAN_POINT ( 'NONE',  ( -10.75313395769540747, -12.68406982142872153, 64.49665988512677472 ) ) ;
#38994 = ORIENTED_EDGE ( 'NONE', *, *, #43765, .T. ) ;
#38995 = ORIENTED_EDGE ( 'NONE', *, *, #19985, .T. ) ;
#38996 = VECTOR ( 'NONE', #605, 1000.000000000000000 ) ;
#38997 = CARTESIAN_POINT ( 'NONE',  ( -22.24284385541303877, -7.587656875400192291, 49.25157356644813689 ) ) ;
#38998 = EDGE_CURVE ( 'NONE', #27411, #39949, #17350, .T. ) ;
#38999 = ADVANCED_FACE ( 'NONE', ( #5702 ), #37168, .T. ) ;
#39000 = CYLINDRICAL_SURFACE ( 'NONE', #16199, 1.500000000000001332 ) ;
#39001 = CARTESIAN_POINT ( 'NONE',  ( -20.06397218905901880, -8.325598534408126028, 73.73713175987984414 ) ) ;
#39002 = EDGE_CURVE ( 'NONE', #35531, #9195, #5714, .T. ) ;
#39003 = EDGE_CURVE ( 'NONE', #16707, #48003, #18944, .T. ) ;
#39004 = B_SPLINE_CURVE_WITH_KNOTS ( 'NONE', 3,
 ( #10725, #25743, #22058, #23045, #38266, #4324, #30436, #4093, #5055, #12429 ),
 .UNSPECIFIED., .F., .F.,
 ( 4, 2, 2, 2, 4 ),
 ( 0.000000000000000000, 0.2500000000000000000, 0.5000000000000000000, 0.7500000000000000000, 1.000000000000000000 ),
 .UNSPECIFIED. ) ;
#39005 = DIRECTION ( 'NONE',  ( -6.336017706050180129E-14, 0.000000000000000000, -1.000000000000000000 ) ) ;
#39006 = CARTESIAN_POINT ( 'NONE',  ( -12.12304913700627829, -10.15599584246782783, 60.76738117878467449 ) ) ;
#39007 = VERTEX_POINT ( 'NONE', #27848 ) ;
#39008 = CARTESIAN_POINT ( 'NONE',  ( -33.52409385541305653, -6.359206544744109735, 48.79999999999998295 ) ) ;
#39009 = CARTESIAN_POINT ( 'NONE',  ( -17.91414045948978639, -21.84516348726148394, 65.76020891215902964 ) ) ;
#39010 = ORIENTED_EDGE ( 'NONE', *, *, #3826, .T. ) ;
#39011 = CARTESIAN_POINT ( 'NONE',  ( -21.84256997353123353, -8.809979007422205299, 66.77494628644626573 ) ) ;
#39012 = CARTESIAN_POINT ( 'NONE',  ( -12.84719740098974583, -9.512790884556105553, 74.61923006383901225 ) ) ;
#39013 = VERTEX_POINT ( 'NONE', #1503 ) ;
#39014 = CARTESIAN_POINT ( 'NONE',  ( -18.57746183813887697, -21.71359645443963515, 72.57045538883467373 ) ) ;
#39015 = ORIENTED_EDGE ( 'NONE', *, *, #11390, .T. ) ;
#39016 = CARTESIAN_POINT ( 'NONE',  ( -12.38445583493520630, -13.33796604008351316, 52.02966884056656482 ) ) ;
#39017 = EDGE_CURVE ( 'NONE', #38546, #7285, #46582, .T. ) ;
#39018 = DIRECTION ( 'NONE',  ( 0.5351595679979623821, 0.8447509909909750592, 0.000000000000000000 ) ) ;
#39019 = CARTESIAN_POINT ( 'NONE',  ( -21.25455046938168735, -8.881090050001144931, 70.28699408244519020 ) ) ;
#39020 = DIRECTION ( 'NONE',  ( -1.000000000000000000, 0.000000000000000000, 0.000000000000000000 ) ) ;
#39021 = ORIENTED_EDGE ( 'NONE', *, *, #42783, .T. ) ;
#39022 = CARTESIAN_POINT ( 'NONE',  ( -18.60622096112062707, -22.16490860957766529, 72.47006221837980888 ) ) ;
#39023 = CARTESIAN_POINT ( 'NONE',  ( -10.98557813051190202, -17.68114236276378293, 71.56718193507127523 ) ) ;
#39024 = LINE ( 'NONE', #24985, #31762 ) ;
#39025 = AXIS2_PLACEMENT_3D ( 'NONE', #39628, #13257, #9359 ) ;
#39026 = VECTOR ( 'NONE', #16460, 1000.000000000000000 ) ;
#39027 = CARTESIAN_POINT ( 'NONE',  ( -19.16034511560328824, -20.04212228129345874, 53.69233794759168177 ) ) ;
#39028 = CARTESIAN_POINT ( 'NONE',  ( -20.86738180659939701, -20.96527767495129879, 58.85295087929227265 ) ) ;
#39029 = CARTESIAN_POINT ( 'NONE',  ( -17.42409385541299471, -14.80920654474435594, 52.02966884056656482 ) ) ;
#39030 = CARTESIAN_POINT ( 'NONE',  ( -16.27095827323975996, -7.851109476482911909, 64.08499918177189159 ) ) ;
#39031 = EDGE_LOOP ( 'NONE', ( #23963, #34929 ) ) ;
#39032 = CARTESIAN_POINT ( 'NONE',  ( -23.74619265052512418, -11.68934008440960426, 62.95218278636776432 ) ) ;
#39033 = EDGE_LOOP ( 'NONE', ( #15845, #528, #27418, #25069, #38060 ) ) ;
#39034 = CARTESIAN_POINT ( 'NONE',  ( -11.21157534608376061, -11.58358818987947814, 67.91864608155252370 ) ) ;
#39035 = CARTESIAN_POINT ( 'NONE',  ( -22.93319430828029581, -10.48995392174254526, 63.08802662987923782 ) ) ;
#39036 = ORIENTED_EDGE ( 'NONE', *, *, #16424, .F. ) ;
#39037 = FACE_BOUND ( 'NONE', #23230, .T. ) ;
#39038 = ORIENTED_EDGE ( 'NONE', *, *, #13673, .F. ) ;
#39039 = VERTEX_POINT ( 'NONE', #42880 ) ;
#39040 = EDGE_LOOP ( 'NONE', ( #38887, #8728, #6606, #18978 ) ) ;
#39041 = CARTESIAN_POINT ( 'NONE',  ( -15.46621039653938112, -10.55127575485719582, 52.02966884056656482 ) ) ;
#39042 = CARTESIAN_POINT ( 'NONE',  ( -22.48430581236326731, -20.27711595259535571, 65.81926302645771898 ) ) ;
#39043 = CARTESIAN_POINT ( 'NONE',  ( -45.92409385541306932, -12.76354662275040042, 70.50000000000000000 ) ) ;
#39044 = CARTESIAN_POINT ( 'NONE',  ( -23.44980453451081104, -18.46889374286061525, 73.06368236440982855 ) ) ;
#39045 = ORIENTED_EDGE ( 'NONE', *, *, #42578, .F. ) ;
#39046 = ORIENTED_EDGE ( 'NONE', *, *, #10091, .F. ) ;
#39047 = CARTESIAN_POINT ( 'NONE',  ( -20.75534385650551528, -7.417179338643134834, 52.18511593390279302 ) ) ;
#39048 = EDGE_CURVE ( 'NONE', #12811, #32800, #42248, .T. ) ;
#39049 = LINE ( 'NONE', #46211, #14951 ) ;
#39050 = CARTESIAN_POINT ( 'NONE',  ( -18.24390634433515856, -19.99480269976908176, 50.77966884056656482 ) ) ;
#39051 = CARTESIAN_POINT ( 'NONE',  ( -24.05059673655033947, -17.06518960458298650, 73.18336032079744768 ) ) ;
#39052 =( BOUNDED_CURVE ( )  B_SPLINE_CURVE ( 3, ( #14953, #18658, #3405, #39326 ),
 .UNSPECIFIED., .F., .F. ) 
 B_SPLINE_CURVE_WITH_KNOTS ( ( 4, 4 ),
 ( 0.9074455897393621795, 1.000000000000000000 ),
 .UNSPECIFIED. ) 
 CURVE ( )  GEOMETRIC_REPRESENTATION_ITEM ( )  RATIONAL_B_SPLINE_CURVE ( ( 0.6983129098260896228, 0.7760317562606953157, 0.8765941196519987377, 1.000000000000000000 ) ) 
 REPRESENTATION_ITEM ( '' )  );
#39053 = CARTESIAN_POINT ( 'NONE',  ( -13.41159385650551528, -6.922745924619793101, 51.69366785382590024 ) ) ;
#39054 = VECTOR ( 'NONE', #7402, 1000.000000000000114 ) ;
#39056 = ORIENTED_EDGE ( 'NONE', *, *, #2858, .T. ) ;
#39055 = ADVANCED_FACE ( 'NONE', ( #24166 ), #45051, .T. ) ;
#39057 = CARTESIAN_POINT ( 'NONE',  ( -23.05109822670184272, -10.64471945476145898, 59.88586922199753104 ) ) ;
#39058 = CARTESIAN_POINT ( 'NONE',  ( -26.59010385426081413, -19.80682416827059455, 54.49999999999995026 ) ) ;
#39059 = ADVANCED_FACE ( 'NONE', ( #19660 ), #23993, .T. ) ;
#39060 = CARTESIAN_POINT ( 'NONE',  ( -21.68202464530013529, -12.85132308587069794, 49.52966884056655772 ) ) ;
#39061 = AXIS2_PLACEMENT_3D ( 'NONE', #40318, #47473, #21376 ) ;
#39062 = EDGE_CURVE ( 'NONE', #39384, #21434, #36206, .T. ) ;
#39063 = B_SPLINE_CURVE_WITH_KNOTS ( 'NONE', 1,
 ( #928, #15192 ),
 .UNSPECIFIED., .F., .F.,
 ( 2, 2 ),
 ( 0.000000000000000000, 1.000000000000000000 ),
 .UNSPECIFIED. ) ;
#39064 = ORIENTED_EDGE ( 'NONE', *, *, #3947, .F. ) ;
#39065 = CARTESIAN_POINT ( 'NONE',  ( -10.37795889460693033, -14.56696403379599225, 68.14328054657653411 ) ) ;
#39066 =( BOUNDED_CURVE ( )  B_SPLINE_CURVE ( 3, ( #30537, #972, #23377, #22648 ),
 .UNSPECIFIED., .F., .F. ) 
 B_SPLINE_CURVE_WITH_KNOTS ( ( 4, 4 ),
 ( 0.5000000000000000000, 0.9074455897393653991 ),
 .UNSPECIFIED. ) 
 CURVE ( )  GEOMETRIC_REPRESENTATION_ITEM ( )  RATIONAL_B_SPLINE_CURVE ( ( 1.000000000000007327, 0.4567392136813294146, 0.3561768502900241606, 0.6983129098260996148 ) ) 
 REPRESENTATION_ITEM ( '' )  );
#39067 = DIRECTION ( 'NONE',  ( 1.000000000000000000, -0.000000000000000000, -0.000000000000000000 ) ) ;
#39068 = CARTESIAN_POINT ( 'NONE',  ( -11.56806251476610115, -18.73522173559940995, 65.03234934376791898 ) ) ;
#39069 = CARTESIAN_POINT ( 'NONE',  ( -18.97210877009940688, -7.521729958488855061, 66.94425830142937173 ) ) ;
#39070 = B_SPLINE_CURVE_WITH_KNOTS ( 'NONE', 3,
 ( #25589, #40598, #40373, #2931, #48235, #36649, #6641, #29530, #32958, #37380 ),
 .UNSPECIFIED., .F., .F.,
 ( 4, 2, 2, 2, 4 ),
 ( 0.000000000000000000, 0.2500000000000000000, 0.5000000000000000000, 0.7500000000000000000, 1.000000000000000000 ),
 .UNSPECIFIED. ) ;
#39071 = VERTEX_POINT ( 'NONE', #45531 ) ;
#39072 = LINE ( 'NONE', #34653, #10793 ) ;
#39073 = CARTESIAN_POINT ( 'NONE',  ( -22.29619887594318683, -17.36118473213641167, 53.49999999999995026 ) ) ;
#39074 = DIRECTION ( 'NONE',  ( 0.9687793358424822143, -0.2479245821708672415, 0.000000000000000000 ) ) ;
#39075 = ORIENTED_EDGE ( 'NONE', *, *, #33588, .T. ) ;
#39076 = CARTESIAN_POINT ( 'NONE',  ( -6.424093855413055110, -25.10920654474410441, 47.99999999999998579 ) ) ;
#39077 =( BOUNDED_CURVE ( )  B_SPLINE_CURVE ( 3, ( #33125, #48402, #19102, #7056 ),
 .UNSPECIFIED., .F., .F. ) 
 B_SPLINE_CURVE_WITH_KNOTS ( ( 4, 4 ),
 ( 0.4074455897393615689, 0.5000000000000000000 ),
 .UNSPECIFIED. ) 
 CURVE ( )  GEOMETRIC_REPRESENTATION_ITEM ( )  RATIONAL_B_SPLINE_CURVE ( ( 0.6983129098260875134, 0.7760317562606922071, 0.8765941196519960732, 0.9999999999999981126 ) ) 
 REPRESENTATION_ITEM ( '' )  );
#39078 = ORIENTED_EDGE ( 'NONE', *, *, #43236, .F. ) ;
#39079 = LINE ( 'NONE', #9060, #20296 ) ;
#39080 = CARTESIAN_POINT ( 'NONE',  ( -10.37873872693602273, -15.23103030436339544, 74.95345861988057834 ) ) ;
#39081 = VERTEX_POINT ( 'NONE', #15207 ) ;
#39082 = CARTESIAN_POINT ( 'NONE',  ( -24.41553149706675896, -15.71832598455623398, 69.81835354388927328 ) ) ;
#39083 = CARTESIAN_POINT ( 'NONE',  ( -10.90323534495222546, -12.10858216263579124, 57.47290069719868910 ) ) ;
#39084 = CARTESIAN_POINT ( 'NONE',  ( -24.23115020962818278, -13.17656271950065161, 62.83264225666157188 ) ) ;
#39085 = LINE ( 'NONE', #11593, #36093 ) ;
#39086 = ORIENTED_EDGE ( 'NONE', *, *, #21805, .F. ) ;
#39087 = DIRECTION ( 'NONE',  ( -0.3478314405900308492, -0.9375570856950864451, 0.000000000000000000 ) ) ;
#39088 = CARTESIAN_POINT ( 'NONE',  ( -20.88270717056239789, -21.40782548341276481, 58.82970473467946704 ) ) ;
#39089 = CARTESIAN_POINT ( 'NONE',  ( -10.09263637371726041, -16.13336529236863015, 68.02121877882343881 ) ) ;
#39090 = ORIENTED_EDGE ( 'NONE', *, *, #9006, .F. ) ;
#39091 = CARTESIAN_POINT ( 'NONE',  ( -11.45027127459337279, -18.55327342931734691, 61.57151016578320935 ) ) ;
#39092 = CIRCLE ( 'NONE', #17070, 2.000000000000000888 ) ;
#39093 = CIRCLE ( 'NONE', #10764, 1.250000000000001110 ) ;
#39094 = FACE_OUTER_BOUND ( 'NONE', #26972, .T. ) ;
#39095 = B_SPLINE_CURVE_WITH_KNOTS ( 'NONE', 3,
 ( #21695, #33474, #7419, #26360, #45332, #22187, #37171, #44360, #40637, #14274 ),
 .UNSPECIFIED., .F., .F.,
 ( 4, 2, 2, 2, 4 ),
 ( 0.1272669073658244943, 0.2522669073463070233, 0.3772669073267895801, 0.5022669073072720813, 0.6272669072877545826 ),
 .UNSPECIFIED. ) ;
#39096 = ORIENTED_EDGE ( 'NONE', *, *, #22491, .F. ) ;
#39097 = ORIENTED_EDGE ( 'NONE', *, *, #1828, .T. ) ;
#39098 = CARTESIAN_POINT ( 'NONE',  ( -20.43749099114212342, -18.39845715627588874, 52.02966884056656482 ) ) ;
#39099 = DIRECTION ( 'NONE',  ( -3.071710424422018668E-17, 6.404604876783312462E-16, 1.000000000000000000 ) ) ;
#39100 = DIRECTION ( 'NONE',  ( -1.000000000000000000, -2.866981220435666553E-17, 0.000000000000000000 ) ) ;
#39101 = VECTOR ( 'NONE', #45642, 1000.000000000000000 ) ;
#39102 = CARTESIAN_POINT ( 'NONE',  ( -17.96784385650551741, -6.428312510596451368, 51.20221977374900035 ) ) ;
#39103 = CARTESIAN_POINT ( 'NONE',  ( -11.85162103594838001, -10.49015045520576983, 71.25420998615621215 ) ) ;
#39104 = EDGE_CURVE ( 'NONE', #34125, #48039, #48499, .T. ) ;
#39105 = DIRECTION ( 'NONE',  ( -3.071710424422018668E-17, 6.404604876783312462E-16, 1.000000000000000000 ) ) ;
#39106 = CARTESIAN_POINT ( 'NONE',  ( -23.23016983938471824, -18.72167312165286646, 69.36542358921913376 ) ) ;
#39107 = CARTESIAN_POINT ( 'NONE',  ( -13.89389072038462025, -21.36980434119256600, 72.11103101793651149 ) ) ;
#39108 = VERTEX_POINT ( 'NONE', #41578 ) ;
#39109 = ORIENTED_EDGE ( 'NONE', *, *, #4312, .F. ) ;
#39110 = CARTESIAN_POINT ( 'NONE',  ( -10.40277073914389661, -15.44443991871667166, 57.56792809063193062 ) ) ;
#39111 = CARTESIAN_POINT ( 'NONE',  ( -26.42409385541305511, -25.10920654474410441, 52.99999999999997158 ) ) ;
#39112 = CARTESIAN_POINT ( 'NONE',  ( -22.42700276027757411, -19.70584140869366863, 72.66017131446398025 ) ) ;
#39113 = DIRECTION ( 'NONE',  ( -1.081321489524789733E-05, -7.211308818607114576E-06, 0.9999999999155356756 ) ) ;
#39114 = B_SPLINE_CURVE_WITH_KNOTS ( 'NONE', 1,
 ( #15176, #18894 ),
 .UNSPECIFIED., .F., .F.,
 ( 2, 2 ),
 ( 0.000000000000000000, 1.000000000000000000 ),
 .UNSPECIFIED. ) ;
#39115 = ORIENTED_EDGE ( 'NONE', *, *, #27878, .F. ) ;
#39116 = CARTESIAN_POINT ( 'NONE',  ( -20.17979545193272273, -21.30158238988698116, 72.28990119599492914 ) ) ;
#39117 = CARTESIAN_POINT ( 'NONE',  ( -24.86601949095794239, -14.46076817688473071, 66.43938638393159124 ) ) ;
#39118 = ADVANCED_FACE ( 'NONE', ( #7862 ), #22883, .T. ) ;
#39119 = APPLICATION_CONTEXT ( 'automotive_design' ) ;
#39120 = CARTESIAN_POINT ( 'NONE',  ( -22.79734351242366941, -10.24514170768878962, 66.69182257473532616 ) ) ;
#39121 = CARTESIAN_POINT ( 'NONE',  ( -45.92409385541306222, -14.80920654474410902, 70.50000000000000000 ) ) ;
#39122 = EDGE_CURVE ( 'NONE', #24230, #15059, #41831, .T. ) ;
#39123 = ORIENTED_EDGE ( 'NONE', *, *, #25703, .F. ) ;
#39124 = CARTESIAN_POINT ( 'NONE',  ( -24.41485940220508510, -14.44976662329334616, 66.18292729254385165 ) ) ;
#39125 = AXIS2_PLACEMENT_3D ( 'NONE', #29502, #48214, #44534 ) ;
#39126 = EDGE_CURVE ( 'NONE', #38697, #26255, #3549, .T. ) ;
#39127 = LINE ( 'NONE', #30795, #46376 ) ;
#39128 = CARTESIAN_POINT ( 'NONE',  ( -24.42331094741535580, -14.99212712107751955, 59.35373227113915107 ) ) ;
#39129 = VECTOR ( 'NONE', #16429, 1000.000000000000114 ) ;
#39130 = CARTESIAN_POINT ( 'NONE',  ( -14.31284414862750864, -10.25749249327297896, 53.88362224778187226 ) ) ;
#39131 = EDGE_CURVE ( 'NONE', #39358, #20248, #10736, .T. ) ;
#39132 = CARTESIAN_POINT ( 'NONE',  ( -18.90996479553717791, -7.968725069611966916, 66.90071784165556323 ) ) ;
#39133 = VERTEX_POINT ( 'NONE', #16175 ) ;
#39134 = CARTESIAN_POINT ( 'NONE',  ( -10.49786192289579922, -13.78684457455405088, 57.51995378590393670 ) ) ;
#39135 = ORIENTED_EDGE ( 'NONE', *, *, #4349, .T. ) ;
#39136 = CARTESIAN_POINT ( 'NONE',  ( -10.00806915883838855, -14.09796239111615890, 61.11095435805616205 ) ) ;
#39137 = DIRECTION ( 'NONE',  ( 9.637352644315596475E-17, -0.000000000000000000, 1.000000000000000000 ) ) ;
#39138 = ORIENTED_EDGE ( 'NONE', *, *, #42475, .F. ) ;
#39139 = CARTESIAN_POINT ( 'NONE',  ( -24.42549660922115251, -13.91739599595199728, 69.80842429065324950 ) ) ;
#39140 = CARTESIAN_POINT ( 'NONE',  ( -18.39951258112534305, -22.19516185762106275, 69.00009993223443416 ) ) ;
#39141 = CARTESIAN_POINT ( 'NONE',  ( -16.36784385650551954, -6.428312510596451368, 51.20221977374900035 ) ) ;
#39142 = ORIENTED_EDGE ( 'NONE', *, *, #3461, .F. ) ;
#39143 = CARTESIAN_POINT ( 'NONE',  ( -11.93102524044397938, -10.47028995287008257, 71.26893105764186487 ) ) ;
#39144 = CARTESIAN_POINT ( 'NONE',  ( -14.77897477670383353, -8.270997283837589364, 56.73511376018900876 ) ) ;
#39145 = B_SPLINE_CURVE_WITH_KNOTS ( 'NONE', 1,
 ( #4269, #11403 ),
 .UNSPECIFIED., .F., .F.,
 ( 2, 2 ),
 ( 0.000000000000000000, 1.000000000000000000 ),
 .UNSPECIFIED. ) ;
#39146 = CARTESIAN_POINT ( 'NONE',  ( -10.89682964601354698, -17.33834430218308498, 64.62739378818586999 ) ) ;
#39147 = ORIENTED_EDGE ( 'NONE', *, *, #40964, .F. ) ;
#39148 = CARTESIAN_POINT ( 'NONE',  ( -18.24390634433515856, -19.99480269976908176, 52.02966884056656482 ) ) ;
#39149 = CARTESIAN_POINT ( 'NONE',  ( -19.36557164464469594, -19.08778335711046026, 49.52966884056656482 ) ) ;
#39150 = CARTESIAN_POINT ( 'NONE',  ( -10.93232766038821424, -17.55941949638709687, 68.38249893951126523 ) ) ;
#39151 = DIRECTION ( 'NONE',  ( -0.7107718805962432995, -0.7034225854731134264, -7.722840056494082694E-09 ) ) ;
#39152 = DIRECTION ( 'NONE',  ( 0.8603613874411328855, -0.3191920208248662516, -0.3973597071195153485 ) ) ;
#39153 = VERTEX_POINT ( 'NONE', #705 ) ;
#39154 = ORIENTED_EDGE ( 'NONE', *, *, #32752, .T. ) ;
#39155 = CARTESIAN_POINT ( 'NONE',  ( -11.68335768792166185, -18.81469630946190819, 68.51689631952916670 ) ) ;
#39156 = CARTESIAN_POINT ( 'NONE',  ( -13.27770768808250956, -9.107454094634595876, 63.90946529206384241 ) ) ;
#39157 = ORIENTED_EDGE ( 'NONE', *, *, #46345, .T. ) ;
#39159 = CARTESIAN_POINT ( 'NONE',  ( -15.82103535061131261, -7.533639916251397395, 67.39653228388428374 ) ) ;
#39158 = VECTOR ( 'NONE', #36219, 1000.000000000000227 ) ;
#39160 = CYLINDRICAL_SURFACE ( 'NONE', #29472, 4.686499999999997002 ) ;
#39161 = CARTESIAN_POINT ( 'NONE',  ( -17.77409385759798965, -6.859212275519751323, 50.50378509014259265 ) ) ;
#39162 = CARTESIAN_POINT ( 'NONE',  ( -13.06442264889613192, -8.767972821088468649, 64.10284853510081859 ) ) ;
#39163 = EDGE_CURVE ( 'NONE', #18099, #27374, #12027, .T. ) ;
#39164 = LINE ( 'NONE', #24652, #45585 ) ;
#39165 = CARTESIAN_POINT ( 'NONE',  ( -15.69736356130078647, -8.025520047610617880, 70.90989840317035942 ) ) ;
#39166 = AXIS2_PLACEMENT_3D ( 'NONE', #31761, #39391, #20445 ) ;
#39167 = ORIENTED_EDGE ( 'NONE', *, *, #40240, .T. ) ;
#39168 = CARTESIAN_POINT ( 'NONE',  ( -13.00210270896756803, -8.813292789292800578, 64.04799975586527694 ) ) ;
#39169 = DIRECTION ( 'NONE',  ( -0.1738928961406289164, 0.9847645711904029486, 7.871847295470929299E-08 ) ) ;
#39170 = AXIS2_PLACEMENT_3D ( 'NONE', #35746, #42010, #35517 ) ;
#39171 = DIRECTION ( 'NONE',  ( -1.411223638961666279E-06, -4.279116281890322592E-06, -0.9999999999898487868 ) ) ;
#39172 = CARTESIAN_POINT ( 'NONE',  ( -14.09638704727594138, -8.593948190025162859, 74.19954651715224259 ) ) ;
#39173 = EDGE_CURVE ( 'NONE', #19371, #25718, #30751, .T. ) ;
#39174 = ORIENTED_EDGE ( 'NONE', *, *, #14822, .F. ) ;
#39175 = ORIENTED_EDGE ( 'NONE', *, *, #2600, .F. ) ;
#39176 = EDGE_LOOP ( 'NONE', ( #17593, #33559, #10153, #8135 ) ) ;
#39177 = CARTESIAN_POINT ( 'NONE',  ( -24.87123163304818974, -14.59964195235338735, 62.89791815715346956 ) ) ;
#39178 = DIRECTION ( 'NONE',  ( 0.000000000000000000, 1.000000000000000000, -0.000000000000000000 ) ) ;
#39179 = EDGE_CURVE ( 'NONE', #21955, #6964, #29773, .T. ) ;
#39180 = CARTESIAN_POINT ( 'NONE',  ( -14.78754730678460660, -8.270772302057270764, 60.46996282000571199 ) ) ;
#39181 = VERTEX_POINT ( 'NONE', #24081 ) ;
#39182 = LINE ( 'NONE', #35486, #37643 ) ;
#39183 = ADVANCED_FACE ( 'NONE', ( #31458 ), #24277, .T. ) ;
#39184 = CARTESIAN_POINT ( 'NONE',  ( -22.53429313110963150, -9.952421254863264011, 73.78161091678163075 ) ) ;
#39185 = VERTEX_POINT ( 'NONE', #9553 ) ;
#39186 = CARTESIAN_POINT ( 'NONE',  ( -10.99575410903449679, -18.57485570963264010, 57.85068653066719691 ) ) ;
#39187 = AXIS2_PLACEMENT_3D ( 'NONE', #399, #22554, #29215 ) ;
#39188 = EDGE_CURVE ( 'NONE', #47654, #28368, #34030, .T. ) ;
#39189 = CARTESIAN_POINT ( 'NONE',  ( -17.59211729576255934, -7.811223397794364587, 63.55057029380298417 ) ) ;
#39190 = ORIENTED_EDGE ( 'NONE', *, *, #14610, .F. ) ;
#39191 = CARTESIAN_POINT ( 'NONE',  ( -10.78771056441093101, -12.58245623652513068, 57.43743428873830936 ) ) ;
#39192 = ORIENTED_EDGE ( 'NONE', *, *, #20171, .T. ) ;
#39193 = CARTESIAN_POINT ( 'NONE',  ( -10.12501222943673085, -13.31701186804058601, 74.78479332379183120 ) ) ;
#39194 = AXIS2_PLACEMENT_3D ( 'NONE', #14287, #44610, #48285 ) ;
#39195 = VECTOR ( 'NONE', #38052, 1000.000000000000000 ) ;
#39196 = EDGE_LOOP ( 'NONE', ( #7891, #1745 ) ) ;
#39197 = CARTESIAN_POINT ( 'NONE',  ( -14.22938784291135406, -8.524548850093141894, 71.02957622767809198 ) ) ;
#39198 = CARTESIAN_POINT ( 'NONE',  ( -12.52524223387102253, -19.88411517873010226, 61.60498656843740406 ) ) ;
#39199 = CARTESIAN_POINT ( 'NONE',  ( -24.05845721068777010, -12.57644527891515551, 73.54225570276561541 ) ) ;
#39200 = ORIENTED_EDGE ( 'NONE', *, *, #43310, .F. ) ;
#39201 = DIRECTION ( 'NONE',  ( -2.866981220435666553E-17, 1.000000000000000000, 1.190614954331866791E-16 ) ) ;
#39202 = CARTESIAN_POINT ( 'NONE',  ( -14.68443175557002434, -7.881056518746638595, 60.45962889931271178 ) ) ;
#39203 = CARTESIAN_POINT ( 'NONE',  ( -24.11734051643545484, -11.53754943384703147, 63.05944116141331790 ) ) ;
#39204 = VECTOR ( 'NONE', #12141, 1000.000000000000000 ) ;
#39205 =( BOUNDED_CURVE ( )  B_SPLINE_CURVE ( 3, ( #20741, #39207, #9672, #5492 ),
 .UNSPECIFIED., .F., .F. ) 
 B_SPLINE_CURVE_WITH_KNOTS ( ( 4, 4 ),
 ( 0.4074455897279358751, 0.5000000000000000000 ),
 .UNSPECIFIED. ) 
 CURVE ( )  GEOMETRIC_REPRESENTATION_ITEM ( )  RATIONAL_B_SPLINE_CURVE ( ( 0.6983129097972999855, 0.7760317562358755028, 0.8765941196367799115, 1.000000000000023315 ) ) 
 REPRESENTATION_ITEM ( '' )  );
#39206 = ADVANCED_FACE ( 'NONE', ( #35861 ), #31704, .T. ) ;
#39207 = CARTESIAN_POINT ( 'NONE',  ( -11.17819277842271930, -11.53937649752676720, 67.61864623736559565 ) ) ;
#39208 = CARTESIAN_POINT ( 'NONE',  ( -10.45720024584091945, -15.50224739959347175, 61.26618945053532173 ) ) ;
#39209 = CARTESIAN_POINT ( 'NONE',  ( -10.38541819892233597, -17.25046345042985507, 61.25768869185118604 ) ) ;
#39210 = ORIENTED_EDGE ( 'NONE', *, *, #43070, .F. ) ;
#39211 = CARTESIAN_POINT ( 'NONE',  ( -10.41569439578338496, -15.57669382292980131, 61.05261153187079515 ) ) ;
#39212 = ADVANCED_FACE ( 'NONE', ( #39572 ), #13454, .F. ) ;
#39213 = CARTESIAN_POINT ( 'NONE',  ( -17.72634075389897035, -21.85272461700124680, 58.55553378267870812 ) ) ;
#39214 = CARTESIAN_POINT ( 'NONE',  ( -24.86566085326441211, -14.45379301838039865, 66.37631023280182774 ) ) ;
#39215 = CARTESIAN_POINT ( 'NONE',  ( -17.42409385541305511, -14.80920654474410725, 48.99999999999997868 ) ) ;
#39216 = CARTESIAN_POINT ( 'NONE',  ( -14.07761835836965858, -20.95746660330474143, 72.22607703844037985 ) ) ;
#39217 = EDGE_CURVE ( 'NONE', #5635, #4167, #12972, .T. ) ;
#39218 = CARTESIAN_POINT ( 'NONE',  ( -17.91159385650551528, -6.922745924619793101, 51.69366785382590024 ) ) ;
#39219 = ORIENTED_EDGE ( 'NONE', *, *, #31495, .T. ) ;
#39220 = CARTESIAN_POINT ( 'NONE',  ( -24.47371109942907808, -14.90716652360855576, 59.25772288469824645 ) ) ;
#39221 = DIRECTION ( 'NONE',  ( -8.226841962295982234E-06, 2.386003339349608660E-06, 0.9999999999633130132 ) ) ;
#39222 = EDGE_LOOP ( 'NONE', ( #21384, #2440, #42464, #12489, #40244 ) ) ;
#39223 = DIRECTION ( 'NONE',  ( -2.168404344971008375E-16, 0.000000000000000000, 1.000000000000000000 ) ) ;
#39224 = CARTESIAN_POINT ( 'NONE',  ( -23.99312320239454976, -11.29471777418100231, 66.60709819448160829 ) ) ;
#39225 = CARTESIAN_POINT ( 'NONE',  ( -17.90018989731357735, -22.24414728290300047, 62.01502546368934077 ) ) ;
#39226 = CARTESIAN_POINT ( 'NONE',  ( -12.74057395449646712, -20.01165780218009971, 68.62192124028820217 ) ) ;
#39227 = CARTESIAN_POINT ( 'NONE',  ( -15.03764954898300488, -21.45148416623199594, 58.32185190926050211 ) ) ;
#39228 = EDGE_LOOP ( 'NONE', ( #8692, #42992, #7076, #15275 ) ) ;
#39229 = CARTESIAN_POINT ( 'NONE',  ( -22.35906936724365579, -19.84913318925590175, 72.94400511917729091 ) ) ;
#39230 =( BOUNDED_SURFACE ( )  B_SPLINE_SURFACE ( 3, 1, ( 
 ( #727, #30533 ),
 ( #45553, #23142 ),
 ( #4408, #19426 ),
 ( #1436, #16451 ),
 ( #20156, #32456 ),
 ( #43307, #16927 ),
 ( #31484, #1927 ) ),
 .UNSPECIFIED., .T., .F., .F. ) 
 B_SPLINE_SURFACE_WITH_KNOTS ( ( 4, 3, 4 ),
 ( 2, 2 ),
 ( 0.000000000000000000, 0.5000000000000000000, 1.000000000000000000 ),
 ( 0.000000000000000000, 1.000000000000000000 ),
 .UNSPECIFIED. ) 
 GEOMETRIC_REPRESENTATION_ITEM ( )  RATIONAL_B_SPLINE_SURFACE ( (
 ( 1.000000000000000000, 1.000000000000000000),
 ( 0.3333333333333335369, 0.3333333333333330373),
 ( 0.3333333333333335369, 0.3333333333333330373),
 ( 1.000000000000000000, 1.000000000000000000),
 ( 0.3333333333333333703, 0.3333333333333333703),
 ( 0.3333333333333333703, 0.3333333333333333703),
 ( 1.000000000000000000, 1.000000000000000000) ) ) 
 REPRESENTATION_ITEM ( '' )  SURFACE ( )  );
#39231 = CARTESIAN_POINT ( 'NONE',  ( -11.50273385864769438, -11.07591097799543256, 57.50903212538073461 ) ) ;
#39232 = LINE ( 'NONE', #12399, #17299 ) ;
#39233 = VERTEX_POINT ( 'NONE', #32195 ) ;
#39234 = CARTESIAN_POINT ( 'NONE',  ( -17.40545348791034286, -7.756229321676927135, 70.90524440011041918 ) ) ;
#39235 = B_SPLINE_CURVE_WITH_KNOTS ( 'NONE', 3,
 ( #36553, #36081, #43996, #20842, #10251, #36796, #2365, #24786, #21335, #17377 ),
 .UNSPECIFIED., .F., .F.,
 ( 4, 2, 2, 2, 4 ),
 ( 0.6272669072877758989, 0.7522669073072892898, 0.8772669073268026807, 1.002266907346315961, 1.127266907365829463 ),
 .UNSPECIFIED. ) ;
#39236 = CIRCLE ( 'NONE', #718, 2.500000000000002220 ) ;
#39237 = CARTESIAN_POINT ( 'NONE',  ( -13.37043603341178688, -9.101843825305518720, 64.19330030611368443 ) ) ;
#39238 =( GEOMETRIC_REPRESENTATION_CONTEXT ( 3 ) GLOBAL_UNCERTAINTY_ASSIGNED_CONTEXT ( ( #10025 ) ) GLOBAL_UNIT_ASSIGNED_CONTEXT ( ( #43856, #19432, #34693 ) ) REPRESENTATION_CONTEXT ( 'NONE', 'WORKASPACE' ) );
#39239 = CARTESIAN_POINT ( 'NONE',  ( -24.54003134496739946, -12.60314121952208311, 69.96517145308561680 ) ) ;
#39240 = CARTESIAN_POINT ( 'NONE',  ( -21.93588290314558265, -13.54151500546508657, 49.52966884056655772 ) ) ;
#39241 = CARTESIAN_POINT ( 'NONE',  ( -10.75313422144682463, -12.68406895456895889, 64.34006388750040628 ) ) ;
#39242 = VECTOR ( 'NONE', #18760, 1000.000000000000114 ) ;
#39243 = CIRCLE ( 'NONE', #6192, 2.000000000000000444 ) ;
#39244 = ORIENTED_EDGE ( 'NONE', *, *, #41951, .F. ) ;
#39245 = VERTEX_POINT ( 'NONE', #27522 ) ;
#39246 = CARTESIAN_POINT ( 'NONE',  ( -19.88034385541304871, -9.360768649639302552, 51.01397948905922419 ) ) ;
#39247 = DIRECTION ( 'NONE',  ( -0.5088156898428700670, -0.8608754809899751281, -5.922709712363688559E-08 ) ) ;
#39248 = CARTESIAN_POINT ( 'NONE',  ( -14.81535805098777736, -7.777528402031247623, 53.89198173725363716 ) ) ;
#39249 = AXIS2_PLACEMENT_3D ( 'NONE', #28257, #20387, #13206 ) ;
#39250 = CARTESIAN_POINT ( 'NONE',  ( -11.60006141122767609, -10.16330251221877390, 71.08397807149754044 ) ) ;
#39251 = ADVANCED_FACE ( 'NONE', ( #42562 ), #20832, .F. ) ;
#39252 = CARTESIAN_POINT ( 'NONE',  ( -22.92107871295896970, -10.47515356817426202, 59.82876682489222020 ) ) ;
#39253 = FACE_OUTER_BOUND ( 'NONE', #22858, .T. ) ;
#39254 = ORIENTED_EDGE ( 'NONE', *, *, #28521, .F. ) ;
#39255 = CARTESIAN_POINT ( 'NONE',  ( -10.39538363539702104, -14.16717768424945412, 68.00232930279112509 ) ) ;
#39256 = CARTESIAN_POINT ( 'NONE',  ( -24.46146587544552276, -14.38248120490118609, 66.46820668217904426 ) ) ;
#39257 = ORIENTED_EDGE ( 'NONE', *, *, #10376, .F. ) ;
#39258 = FACE_OUTER_BOUND ( 'NONE', #41159, .T. ) ;
#39259 = DIRECTION ( 'NONE',  ( 0.9687793358424821033, -0.2479245821708677133, 0.000000000000000000 ) ) ;
#39260 = VERTEX_POINT ( 'NONE', #6079 ) ;
#39261 = B_SPLINE_CURVE_WITH_KNOTS ( 'NONE', 3,
 ( #33902, #4598, #19617, #41292, #12227, #30475, #34625, #30953, #7827, #45964 ),
 .UNSPECIFIED., .F., .F.,
 ( 4, 2, 2, 2, 4 ),
 ( 0.000000000000000000, 0.2500000000000000000, 0.5000000000000000000, 0.7500000000000000000, 1.000000000000000000 ),
 .UNSPECIFIED. ) ;
#39262 = CARTESIAN_POINT ( 'NONE',  ( -13.33866014084052409, -21.03912497029407902, 61.61622683954244195 ) ) ;
#39263 = CARTESIAN_POINT ( 'NONE',  ( -15.95285335075216970, -19.84884456522215146, 49.52966884056656482 ) ) ;
#39264 = EDGE_LOOP ( 'NONE', ( #9527, #14331, #7933, #30920, #28209 ) ) ;
#39265 = CARTESIAN_POINT ( 'NONE',  ( -17.39128687056474121, -21.86710222072322907, 58.54986106076864161 ) ) ;
#39266 = B_SPLINE_CURVE_WITH_KNOTS ( 'NONE', 3,
 ( #19080, #42470, #23517, #15862, #34326, #8489, #31133, #19321, #4543, #613 ),
 .UNSPECIFIED., .F., .F.,
 ( 4, 2, 2, 2, 4 ),
 ( 0.000000000000000000, 0.2500000000000000000, 0.5000000000000000000, 0.7500000000000000000, 1.000000000000000000 ),
 .UNSPECIFIED. ) ;
#39267 = DIRECTION ( 'NONE',  ( 3.071710424422018668E-17, -6.404604876783312462E-16, -1.000000000000000000 ) ) ;
#39268 = VECTOR ( 'NONE', #45002, 1000.000000000000114 ) ;
#39269 = CARTESIAN_POINT ( 'NONE',  ( -19.11145711862998553, -7.964113067175272676, 63.58089235102941217 ) ) ;
#39270 = CARTESIAN_POINT ( 'NONE',  ( -18.50517187854146783, -19.38160480531894692, 49.52966884056656482 ) ) ;
#39271 = ORIENTED_EDGE ( 'NONE', *, *, #41183, .F. ) ;
#39272 = CYLINDRICAL_SURFACE ( 'NONE', #18911, 0.1499999999999979128 ) ;
#39273 = DIRECTION ( 'NONE',  ( 0.9862050927915949616, 0.1655279884246635413, 7.765682856207886445E-08 ) ) ;
#39274 = VECTOR ( 'NONE', #14911, 1000.000000000000000 ) ;
#39275 = VECTOR ( 'NONE', #32265, 1000.000000000000000 ) ;
#39276 = EDGE_CURVE ( 'NONE', #3179, #8795, #34459, .T. ) ;
#39277 = CARTESIAN_POINT ( 'NONE',  ( -12.27604185553471616, -19.62628656662749549, 58.21210303282668264 ) ) ;
#39278 = EDGE_CURVE ( 'NONE', #25294, #46160, #21109, .T. ) ;
#39279 = EDGE_CURVE ( 'NONE', #47942, #4057, #24473, .T. ) ;
#39280 = DIRECTION ( 'NONE',  ( 0.9687793358424821033, -0.2479245821708679909, 0.000000000000000000 ) ) ;
#39281 = CARTESIAN_POINT ( 'NONE',  ( -6.424093855413055110, -6.859206544744110623, 47.99999999999998579 ) ) ;
#39282 = LINE ( 'NONE', #4828, #27436 ) ;
#39283 = VERTEX_POINT ( 'NONE', #21594 ) ;
#39284 = CARTESIAN_POINT ( 'NONE',  ( -24.72409385541305582, -15.80920654474410725, 65.99999999999998579 ) ) ;
#39285 = CARTESIAN_POINT ( 'NONE',  ( -11.17650184932293733, -11.65192102369769422, 67.90399238740950238 ) ) ;
#39286 = DIRECTION ( 'NONE',  ( -3.071710424422018668E-17, 6.404604876783312462E-16, 1.000000000000000000 ) ) ;
#39287 = ORIENTED_EDGE ( 'NONE', *, *, #2167, .T. ) ;
#39288 = CARTESIAN_POINT ( 'NONE',  ( -19.99669925590731268, -21.37628624441394010, 68.81993804536961079 ) ) ;
#39289 = ORIENTED_EDGE ( 'NONE', *, *, #23553, .F. ) ;
#39290 = VERTEX_POINT ( 'NONE', #17634 ) ;
#39291 = VERTEX_POINT ( 'NONE', #44492 ) ;
#39292 = DIRECTION ( 'NONE',  ( 1.000000000000000000, -0.000000000000000000, -0.000000000000000000 ) ) ;
#39293 = CARTESIAN_POINT ( 'NONE',  ( -23.17271923358804031, -18.80355860159679082, 66.12389479708080842 ) ) ;
#39294 = CARTESIAN_POINT ( 'NONE',  ( -17.42308114789593532, -7.359157070716391580, 67.21377881820035327 ) ) ;
#39295 = CARTESIAN_POINT ( 'NONE',  ( -18.11889358109259973, -21.82488563948435711, 65.64532159284070190 ) ) ;
#39296 = CARTESIAN_POINT ( 'NONE',  ( -45.92409385541305511, -17.80920654474410370, 71.75000000000000000 ) ) ;
#39297 = ORIENTED_EDGE ( 'NONE', *, *, #31680, .T. ) ;
#39298 = ORIENTED_EDGE ( 'NONE', *, *, #29300, .F. ) ;
#39299 = CARTESIAN_POINT ( 'NONE',  ( -23.00534385650551528, -8.801233750844183135, 48.81488406609782515 ) ) ;
#39300 = EDGE_CURVE ( 'NONE', #23723, #36238, #33131, .T. ) ;
#39301 = CARTESIAN_POINT ( 'NONE',  ( -13.86064791321372880, -8.266642500320580567, 74.39228826228381308 ) ) ;
#39302 = VECTOR ( 'NONE', #25563, 1000.000000000000000 ) ;
#39303 = CARTESIAN_POINT ( 'NONE',  ( -21.12749503816145591, -21.27438112535048376, 62.22816062766979428 ) ) ;
#39304 =( BOUNDED_SURFACE ( )  B_SPLINE_SURFACE ( 3, 1, ( 
 ( #15716, #30773 ),
 ( #22391, #26577 ),
 ( #41343, #7880 ),
 ( #7391, #45548 ),
 ( #18941, #37384 ),
 ( #19185, #41848 ),
 ( #3676, #22641 ) ),
 .UNSPECIFIED., .T., .F., .F. ) 
 B_SPLINE_SURFACE_WITH_KNOTS ( ( 4, 3, 4 ),
 ( 2, 2 ),
 ( 0.000000000000000000, 0.5000000000000000000, 1.000000000000000000 ),
 ( 0.000000000000000000, 1.000000000000000000 ),
 .UNSPECIFIED. ) 
 GEOMETRIC_REPRESENTATION_ITEM ( )  RATIONAL_B_SPLINE_SURFACE ( (
 ( 1.000000000000000000, 1.000000000000000000),
 ( 0.3333333333333335369, 0.3333333333333330373),
 ( 0.3333333333333335369, 0.3333333333333330373),
 ( 1.000000000000000000, 1.000000000000000000),
 ( 0.3333333333333333703, 0.3333333333333333703),
 ( 0.3333333333333333703, 0.3333333333333333703),
 ( 1.000000000000000000, 1.000000000000000000) ) ) 
 REPRESENTATION_ITEM ( '' )  SURFACE ( )  );
#39305 = CARTESIAN_POINT ( 'NONE',  ( -20.84119837601463487, -20.97572066283330727, 62.26471400470415318 ) ) ;
#39306 = CARTESIAN_POINT ( 'NONE',  ( -13.58034385650551812, -6.424090610841176385, 49.80797279389977916 ) ) ;
#39307 = VECTOR ( 'NONE', #36368, 1000.000000000000000 ) ;
#39308 = B_SPLINE_CURVE_WITH_KNOTS ( 'NONE', 3,
 ( #29249, #21619, #48195, #10770, #13953, #13718, #43795, #14425, #32919, #40093 ),
 .UNSPECIFIED., .F., .F.,
 ( 4, 2, 2, 2, 4 ),
 ( 0.000000000000000000, 0.2500000000000000000, 0.5000000000000000000, 0.7500000000000000000, 1.000000000000000000 ),
 .UNSPECIFIED. ) ;
#39309 = ORIENTED_EDGE ( 'NONE', *, *, #30922, .T. ) ;
#39310 = CARTESIAN_POINT ( 'NONE',  ( -14.72034176431206198, -21.75144939791099929, 61.77567047156098567 ) ) ;
#39311 = PLANE ( 'NONE',  #33944 ) ;
#39312 = DIRECTION ( 'NONE',  ( -3.597453700672850830E-07, -4.264980243973025121E-06, 0.9999999999908403270 ) ) ;
#39313 = AXIS2_PLACEMENT_3D ( 'NONE', #47265, #40575, #28781 ) ;
#39314 = ORIENTED_EDGE ( 'NONE', *, *, #48438, .F. ) ;
#39315 = CARTESIAN_POINT ( 'NONE',  ( -24.31482301288783532, -13.31912224170856618, 59.66267924674057355 ) ) ;
#39316 = CARTESIAN_POINT ( 'NONE',  ( -22.84886394736722792, -9.702774549906752810, 73.59665770010028041 ) ) ;
#39317 = CARTESIAN_POINT ( 'NONE',  ( -11.01020281012788971, -12.00512747626467025, 74.84374947347477303 ) ) ;
#39318 = DIRECTION ( 'NONE',  ( 3.549360974551883545E-17, -6.371834667872732552E-18, -1.000000000000000000 ) ) ;
#39319 = ORIENTED_EDGE ( 'NONE', *, *, #31082, .F. ) ;
#39320 = DIRECTION ( 'NONE',  ( 0.2664710960620865765, -0.9638429098994649724, 4.833213314675752896E-08 ) ) ;
#39321 = CARTESIAN_POINT ( 'NONE',  ( -24.82995637329867122, -15.61904065536996278, 73.20292520421178040 ) ) ;
#39322 = CARTESIAN_POINT ( 'NONE',  ( -17.96469556627129194, -21.78991212287910884, 65.53459228959106042 ) ) ;
#39323 = VERTEX_POINT ( 'NONE', #29702 ) ;
#39324 = CARTESIAN_POINT ( 'NONE',  ( -19.42896739221782809, -21.56812523091047851, 62.29503644570711174 ) ) ;
#39325 = EDGE_LOOP ( 'NONE', ( #35671, #12361, #41975, #1861 ) ) ;
#39326 = CARTESIAN_POINT ( 'NONE',  ( -24.47432067347917695, -14.77756146504815327, 59.52828185648635184 ) ) ;
#39327 = DIRECTION ( 'NONE',  ( 0.1571515419521612722, -0.9875744999047174622, 7.433889655140131751E-08 ) ) ;
#39328 = VERTEX_POINT ( 'NONE', #32891 ) ;
#39329 = EDGE_CURVE ( 'NONE', #22802, #28574, #29460, .T. ) ;
#39330 = LINE ( 'NONE', #42307, #8526 ) ;
#39331 = DIRECTION ( 'NONE',  ( 0.9687793358424821033, -0.2479245821708677133, 0.000000000000000000 ) ) ;
#39332 = VECTOR ( 'NONE', #47927, 1000.000000000000000 ) ;
#39333 = FACE_OUTER_BOUND ( 'NONE', #43970, .T. ) ;
#39334 = ORIENTED_EDGE ( 'NONE', *, *, #29163, .F. ) ;
#39335 = CARTESIAN_POINT ( 'NONE',  ( -24.18037252889021005, -17.94870914462638822, 59.18873732074431615 ) ) ;
#39336 = VECTOR ( 'NONE', #6675, 1000.000000000000000 ) ;
#39337 = DIRECTION ( 'NONE',  ( -3.071710424422018668E-17, 6.404604876783312462E-16, 1.000000000000000000 ) ) ;
#39338 = CARTESIAN_POINT ( 'NONE',  ( -46.42632161746406894, -13.24559821555319061, 70.87000000000000455 ) ) ;
#39339 = ORIENTED_EDGE ( 'NONE', *, *, #27492, .T. ) ;
#39340 = CARTESIAN_POINT ( 'NONE',  ( -11.21783165637758550, -18.93062460193366192, 64.93202459354702683 ) ) ;
#39341 = CIRCLE ( 'NONE', #25986, 2.000000000000003109 ) ;
#39342 = EDGE_CURVE ( 'NONE', #44748, #35674, #26015, .T. ) ;
#39343 = ADVANCED_FACE ( 'NONE', ( #44742 ), #13692, .F. ) ;
#39344 = DIRECTION ( 'NONE',  ( -3.071710424422018668E-17, 6.404604876783312462E-16, 1.000000000000000000 ) ) ;
#39345 = EDGE_LOOP ( 'NONE', ( #18664, #3906, #25150, #34275 ) ) ;
#39346 = ORIENTED_EDGE ( 'NONE', *, *, #23060, .F. ) ;
#39347 = EDGE_CURVE ( 'NONE', #3920, #6656, #40942, .T. ) ;
#39348 = CARTESIAN_POINT ( 'NONE',  ( -24.05813527555462628, -11.41757595432783745, 63.06562998582658253 ) ) ;
#39349 = CARTESIAN_POINT ( 'NONE',  ( 18.57590614458695200, 0.6299963676414561675, 50.77646420411990391 ) ) ;
#39350 = PLANE ( 'NONE',  #12307 ) ;
#39351 = CIRCLE ( 'NONE', #34634, 0.5000000000000004441 ) ;
#39352 = CARTESIAN_POINT ( 'NONE',  ( -17.29284385650551670, -7.406986770994973490, 48.81910596585309747 ) ) ;
#39353 = EDGE_CURVE ( 'NONE', #37344, #21796, #38574, .T. ) ;
#39354 =( BOUNDED_CURVE ( )  B_SPLINE_CURVE ( 3, ( #35268, #38969, #34791, #42188 ),
 .UNSPECIFIED., .F., .F. ) 
 B_SPLINE_CURVE_WITH_KNOTS ( ( 4, 4 ),
 ( 0.9074455897393628456, 1.000000000000000000 ),
 .UNSPECIFIED. ) 
 CURVE ( )  GEOMETRIC_REPRESENTATION_ITEM ( )  RATIONAL_B_SPLINE_CURVE ( ( 0.6983129098260694168, 0.7760317562606778852, 0.8765941196519880796, 1.000000000000000000 ) ) 
 REPRESENTATION_ITEM ( '' )  );
#39355 = DIRECTION ( 'NONE',  ( 0.000000000000000000, 0.000000000000000000, 1.000000000000000000 ) ) ;
#39356 = CARTESIAN_POINT ( 'NONE',  ( -20.48780003469585154, -11.24700778661463474, 52.02966884056656482 ) ) ;
#39357 = DIRECTION ( 'NONE',  ( -3.071710424422018668E-17, 6.404604876783312462E-16, 1.000000000000000000 ) ) ;
#39358 = VERTEX_POINT ( 'NONE', #40062 ) ;
#39359 = ORIENTED_EDGE ( 'NONE', *, *, #13750, .F. ) ;
#39360 = CARTESIAN_POINT ( 'NONE',  ( -11.39127492490111315, -11.16067319722467666, 60.69357916181100876 ) ) ;
#39361 = ADVANCED_FACE ( 'NONE', ( #10994 ), #47686, .T. ) ;
#39362 = DIRECTION ( 'NONE',  ( 1.000000000000000000, 0.000000000000000000, 0.000000000000000000 ) ) ;
#39363 = CARTESIAN_POINT ( 'NONE',  ( -23.61204160381034711, -11.53669949605622769, 66.42214514747726639 ) ) ;
#39364 = DIRECTION ( 'NONE',  ( -0.2479245821708678799, -0.9687793358424819923, -2.626836608253746575E-18 ) ) ;
#39365 = CARTESIAN_POINT ( 'NONE',  ( -13.42948644998191732, -8.996466925491649391, 56.85478874482843992 ) ) ;
#39366 = FACE_OUTER_BOUND ( 'NONE', #17591, .T. ) ;
#39367 =( BOUNDED_SURFACE ( )  B_SPLINE_SURFACE ( 3, 1, ( 
 ( #28346, #43611 ),
 ( #39424, #20711 ),
 ( #9643, #16985 ),
 ( #47051, #5930 ),
 ( #20951, #36659 ),
 ( #44569, #14482 ),
 ( #13775, #25371 ) ),
 .UNSPECIFIED., .T., .F., .F. ) 
 B_SPLINE_SURFACE_WITH_KNOTS ( ( 4, 3, 4 ),
 ( 2, 2 ),
 ( 0.000000000000000000, 0.5000000000000000000, 1.000000000000000000 ),
 ( 0.000000000000000000, 1.000000000000000000 ),
 .UNSPECIFIED. ) 
 GEOMETRIC_REPRESENTATION_ITEM ( )  RATIONAL_B_SPLINE_SURFACE ( (
 ( 1.000000000000000000, 1.000000000000000000),
 ( 0.3333333333333335369, 0.3333333333333330373),
 ( 0.3333333333333335369, 0.3333333333333330373),
 ( 1.000000000000000000, 1.000000000000000000),
 ( 0.3333333333333333703, 0.3333333333333333703),
 ( 0.3333333333333333703, 0.3333333333333333703),
 ( 1.000000000000000000, 1.000000000000000000) ) ) 
 REPRESENTATION_ITEM ( '' )  SURFACE ( )  );
#39368 = EDGE_LOOP ( 'NONE', ( #10213, #7439 ) ) ;
#39369 = FACE_OUTER_BOUND ( 'NONE', #31071, .T. ) ;
#39370 = AXIS2_PLACEMENT_3D ( 'NONE', #37423, #18723, #34472 ) ;
#39371 = CARTESIAN_POINT ( 'NONE',  ( -20.66696806162329025, -21.06910005082376358, 58.79475164909958096 ) ) ;
#39372 = DIRECTION ( 'NONE',  ( 1.224646799147353207E-16, 1.000000000000000000, -1.912410701131276611E-32 ) ) ;
#39373 = ORIENTED_EDGE ( 'NONE', *, *, #15261, .F. ) ;
#39374 = VECTOR ( 'NONE', #16554, 1000.000000000000000 ) ;
#39375 = CARTESIAN_POINT ( 'NONE',  ( -11.25622321624083355, -18.98904307544693282, 64.86051675911045322 ) ) ;
#39376 =( BOUNDED_SURFACE ( )  B_SPLINE_SURFACE ( 3, 1, ( 
 ( #22598, #26292 ),
 ( #41071, #15681 ),
 ( #34390, #22352 ),
 ( #11514, #18399 ),
 ( #45760, #19145 ),
 ( #37595, #48445 ),
 ( #3899, #26536 ) ),
 .UNSPECIFIED., .T., .F., .F. ) 
 B_SPLINE_SURFACE_WITH_KNOTS ( ( 4, 3, 4 ),
 ( 2, 2 ),
 ( 0.000000000000000000, 0.5000000000000000000, 1.000000000000000000 ),
 ( 0.000000000000000000, 1.000000000000000000 ),
 .UNSPECIFIED. ) 
 GEOMETRIC_REPRESENTATION_ITEM ( )  RATIONAL_B_SPLINE_SURFACE ( (
 ( 1.000000000000000000, 1.000000000000000000),
 ( 0.3333333333333335369, 0.3333333333333330373),
 ( 0.3333333333333335369, 0.3333333333333330373),
 ( 1.000000000000000000, 1.000000000000000000),
 ( 0.3333333333333333703, 0.3333333333333333703),
 ( 0.3333333333333333703, 0.3333333333333333703),
 ( 1.000000000000000000, 1.000000000000000000) ) ) 
 REPRESENTATION_ITEM ( '' )  SURFACE ( )  );
#39377 = CARTESIAN_POINT ( 'NONE',  ( -21.49816216734858898, -9.116934002111024782, 70.13132539266752019 ) ) ;
#39378 = CARTESIAN_POINT ( 'NONE',  ( -27.42409385541305511, -15.80920654474410725, 48.99999999999997868 ) ) ;
#39379 = DIRECTION ( 'NONE',  ( 1.000000000000000000, 0.000000000000000000, 0.000000000000000000 ) ) ;
#39380 = AXIS2_PLACEMENT_3D ( 'NONE', #7091, #33644, #22109 ) ;
#39381 = CARTESIAN_POINT ( 'NONE',  ( -22.64171105389675276, -20.12707350008254892, 69.36756280019827159 ) ) ;
#39382 = CARTESIAN_POINT ( 'NONE',  ( -18.98647511214439731, -7.985344313229808755, 67.18455284397973060 ) ) ;
#39383 = ADVANCED_FACE ( 'NONE', ( #43767 ), #20818, .T. ) ;
#39384 = VERTEX_POINT ( 'NONE', #36822 ) ;
#39385 = CARTESIAN_POINT ( 'NONE',  ( -23.65719169145585710, -18.88999977852593659, 69.41655123612174805 ) ) ;
#39386 = ORIENTED_EDGE ( 'NONE', *, *, #13969, .F. ) ;
#39387 = CARTESIAN_POINT ( 'NONE',  ( -17.85728874018076340, -21.84618329174708151, 61.89007996730683203 ) ) ;
#39388 = CARTESIAN_POINT ( 'NONE',  ( -21.31115985637654120, -8.927249709250721921, 73.88656608925673197 ) ) ;
#39389 = ORIENTED_EDGE ( 'NONE', *, *, #22985, .F. ) ;
#39390 = EDGE_CURVE ( 'NONE', #28, #7220, #43305, .T. ) ;
#39391 = DIRECTION ( 'NONE',  ( -3.071710424422018668E-17, 6.404604876783312462E-16, 1.000000000000000000 ) ) ;
#39392 = AXIS2_PLACEMENT_3D ( 'NONE', #33113, #27806, #10726 ) ;
#39393 = CARTESIAN_POINT ( 'NONE',  ( -11.42117823542190358, -10.39672530145416829, 74.57738459077027926 ) ) ;
#39394 = B_SPLINE_CURVE_WITH_KNOTS ( 'NONE', 1,
 ( #31662, #42509 ),
 .UNSPECIFIED., .F., .F.,
 ( 2, 2 ),
 ( 0.000000000000000000, 1.000000000000000000 ),
 .UNSPECIFIED. ) ;
#39395 = ORIENTED_EDGE ( 'NONE', *, *, #21616, .T. ) ;
#39396 = CARTESIAN_POINT ( 'NONE',  ( -15.19396558280303822, -21.91766586989539434, 68.61946996636811491 ) ) ;
#39397 = CARTESIAN_POINT ( 'NONE',  ( -10.64225270876709217, -11.72539899671273211, 74.75178466342971717 ) ) ;
#39398 = CARTESIAN_POINT ( 'NONE',  ( -10.93128702722934698, -17.42536716698162280, 64.70027491337052084 ) ) ;
#39399 = ORIENTED_EDGE ( 'NONE', *, *, #14546, .F. ) ;
#39400 = DIRECTION ( 'NONE',  ( 3.071710424422018668E-17, -6.404604876783312462E-16, -1.000000000000000000 ) ) ;
#39401 = CARTESIAN_POINT ( 'NONE',  ( -10.85841931818429629, -17.37798394237199062, 64.91267318220633342 ) ) ;
#39402 = DIRECTION ( 'NONE',  ( 0.000000000000000000, 1.000000000000000000, -0.000000000000000000 ) ) ;
#39403 = VECTOR ( 'NONE', #6112, 1000.000000000000000 ) ;
#39404 = CARTESIAN_POINT ( 'NONE',  ( -45.92409385541305511, -14.80920654474410725, 70.50000000000000000 ) ) ;
#39405 = VERTEX_POINT ( 'NONE', #28872 ) ;
#39406 = VERTEX_POINT ( 'NONE', #48069 ) ;
#39407 = EDGE_CURVE ( 'NONE', #31360, #10683, #376, .T. ) ;
#39408 = VECTOR ( 'NONE', #44024, 1000.000000000000114 ) ;
#39409 = CARTESIAN_POINT ( 'NONE',  ( -11.77030184709744454, -18.93651027082609417, 68.32575532107205163 ) ) ;
#39410 = ORIENTED_EDGE ( 'NONE', *, *, #5470, .T. ) ;
#39411 = CARTESIAN_POINT ( 'NONE',  ( -15.67484944857656082, -7.976566202440097619, 67.02518389757648265 ) ) ;
#39412 = CARTESIAN_POINT ( 'NONE',  ( -19.37709741767962157, -21.53135792448401986, 61.99503678469526591 ) ) ;
#39413 = CARTESIAN_POINT ( 'NONE',  ( -18.56159385759799108, -7.228003583438117552, 51.38655588711986155 ) ) ;
#39414 = ADVANCED_FACE ( 'NONE', ( #10885 ), #43916, .T. ) ;
#39415 = CARTESIAN_POINT ( 'NONE',  ( -12.48160889263952811, -19.84176915467957869, 68.63657425450733740 ) ) ;
#39416 = CARTESIAN_POINT ( 'NONE',  ( -10.57723003925373106, -17.74759380694297306, 71.75373442408677249 ) ) ;
#39417 = AXIS2_PLACEMENT_3D ( 'NONE', #20793, #10204, #47625 ) ;
#39418 = EDGE_LOOP ( 'NONE', ( #24643, #13452, #34868, #12093 ) ) ;
#39419 = ADVANCED_FACE ( 'NONE', ( #40207 ), #21724, .T. ) ;
#39420 = CARTESIAN_POINT ( 'NONE',  ( -22.42594789675818845, -19.77792426076253918, 69.45945937764655298 ) ) ;
#39421 = CARTESIAN_POINT ( 'NONE',  ( -20.83485745854687821, -8.694536277584232309, 60.03052354408486480 ) ) ;
#39422 = CIRCLE ( 'NONE', #4844, 5.249999999999998224 ) ;
#39423 = CARTESIAN_POINT ( 'NONE',  ( -13.40763370604777371, -17.22402126197652805, 52.02966884056656482 ) ) ;
#39424 = CARTESIAN_POINT ( 'NONE',  ( -24.47559319016939483, -14.50700548578266513, 59.39867536442299212 ) ) ;
#39425 = DIRECTION ( 'NONE',  ( -4.115385489420004910E-17, -0.9999954153791273948, -0.003028072113811714535 ) ) ;
#39426 = EDGE_CURVE ( 'NONE', #27258, #6094, #40921, .T. ) ;
#39427 = EDGE_LOOP ( 'NONE', ( #20382, #46572, #44571, #24308, #27805 ) ) ;
#39428 = ORIENTED_EDGE ( 'NONE', *, *, #48257, .F. ) ;
#39429 = ORIENTED_EDGE ( 'NONE', *, *, #36469, .F. ) ;
#39430 = LINE ( 'NONE', #16757, #38242 ) ;
#39431 = AXIS2_PLACEMENT_3D ( 'NONE', #17805, #102, #21765 ) ;
#39432 = CARTESIAN_POINT ( 'NONE',  ( -12.55198883488284878, -12.25722835735234639, 54.07175714974878389 ) ) ;
#39433 = CARTESIAN_POINT ( 'NONE',  ( -50.42609385541305755, -14.80920654474421205, 67.05882352941175384 ) ) ;
#39434 = ORIENTED_EDGE ( 'NONE', *, *, #4037, .F. ) ;
#39435 = CARTESIAN_POINT ( 'NONE',  ( -45.92409385541306222, -13.51240245935757578, 70.50000000000000000 ) ) ;
#39436 = VECTOR ( 'NONE', #38254, 1000.000000000000114 ) ;
#39437 = CARTESIAN_POINT ( 'NONE',  ( -22.57893663749957369, -9.999394138389961384, 73.49633153340955971 ) ) ;
#39438 = ORIENTED_EDGE ( 'NONE', *, *, #612, .F. ) ;
#39439 = VECTOR ( 'NONE', #18552, 1000.000000000000227 ) ;
#39440 = CARTESIAN_POINT ( 'NONE',  ( -11.22150886908280931, -18.16670198096008093, 58.22203402163793839 ) ) ;
#39441 = DIRECTION ( 'NONE',  ( -0.06306825763707681054, 0.9980092158285026605, 2.415158932891090200E-08 ) ) ;
#39442 = VERTEX_POINT ( 'NONE', #25189 ) ;
#39443 = CARTESIAN_POINT ( 'NONE',  ( -19.80301227694363675, -21.44571519258606074, 69.08482476707463604 ) ) ;
#39444 = EDGE_CURVE ( 'NONE', #3865, #20439, #44167, .T. ) ;
#39445 = ORIENTED_EDGE ( 'NONE', *, *, #26722, .T. ) ;
#39446 = CARTESIAN_POINT ( 'NONE',  ( 22.62590614458706639, 1.890747609047893185, 50.53028072113869484 ) ) ;
#39447 = ORIENTED_EDGE ( 'NONE', *, *, #13871, .T. ) ;
#39448 = FACE_OUTER_BOUND ( 'NONE', #42790, .T. ) ;
#39449 = CARTESIAN_POINT ( 'NONE',  ( -8.424093855413067544, -8.109206544744111511, 50.49999999999999289 ) ) ;
#39450 = ORIENTED_EDGE ( 'NONE', *, *, #14215, .F. ) ;
#39451 = CARTESIAN_POINT ( 'NONE',  ( -12.76954176995949375, -15.35549139150514009, 52.02966884056656482 ) ) ;
#39452 = CARTESIAN_POINT ( 'NONE',  ( -14.67819097860952482, -7.883573037801185457, 60.44279363819690332 ) ) ;
#39453 = CARTESIAN_POINT ( 'NONE',  ( -45.55409385541306477, -14.20920654474410760, 70.91501325280044910 ) ) ;
#39454 = CARTESIAN_POINT ( 'NONE',  ( -15.43182990062313564, -8.046249867383863830, 74.36513541778452918 ) ) ;
#39455 = CARTESIAN_POINT ( 'NONE',  ( -17.65810221059773610, -7.762793303104816189, 63.56529088875731759 ) ) ;
#39456 = DIRECTION ( 'NONE',  ( 1.000000000000000000, 2.866981220435666553E-17, 0.000000000000000000 ) ) ;
#39457 = ORIENTED_EDGE ( 'NONE', *, *, #14859, .F. ) ;
#39458 = CARTESIAN_POINT ( 'NONE',  ( -17.55068613527580723, -7.810228624652221896, 63.85057029484593727 ) ) ;
#39459 = CARTESIAN_POINT ( 'NONE',  ( -24.66123687018043498, -13.04105289088702158, 63.03275384083246990 ) ) ;
#39460 = DIRECTION ( 'NONE',  ( 2.866981220435666553E-17, -1.000000000000000000, -1.190614954331866791E-16 ) ) ;
#39461 = LINE ( 'NONE', #15642, #6945 ) ;
#39462 = DIRECTION ( 'NONE',  ( -3.071710424422018668E-17, 6.404604876783312462E-16, 1.000000000000000000 ) ) ;
#39463 = CARTESIAN_POINT ( 'NONE',  ( -15.77409385650551954, -9.792211528768504536, 50.49490371617623197 ) ) ;
#39464 = AXIS2_PLACEMENT_3D ( 'NONE', #25883, #7427, #30083 ) ;
#39465 = EDGE_LOOP ( 'NONE', ( #12682, #34945, #25739, #35341, #28725 ) ) ;
#39466 = ADVANCED_FACE ( 'NONE', ( #6951 ), #10168, .T. ) ;
#39467 = CARTESIAN_POINT ( 'NONE',  ( -20.95545100651803594, -20.91135505560678709, 65.59926067308570907 ) ) ;
#39468 = DIRECTION ( 'NONE',  ( -1.000000000000000000, -2.866981220435666553E-17, -0.000000000000000000 ) ) ;
#39469 = ORIENTED_EDGE ( 'NONE', *, *, #44277, .T. ) ;
#39470 = CARTESIAN_POINT ( 'NONE',  ( -16.71957921250844592, -21.82421608262117729, 68.71032757591046902 ) ) ;
#39471 = CARTESIAN_POINT ( 'NONE',  ( -10.66160605790631344, -13.00123564105898666, 68.03832347539896830 ) ) ;
#39472 = CARTESIAN_POINT ( 'NONE',  ( -14.55661340756572741, -8.423408737790397893, 64.07513534474681194 ) ) ;
#39473 = CARTESIAN_POINT ( 'NONE',  ( -19.44376822123183146, -7.638105259791415413, 60.07597700946195829 ) ) ;
#39474 = ADVANCED_FACE ( 'NONE', ( #37203 ), #17540, .T. ) ;
#39475 = CARTESIAN_POINT ( 'NONE',  ( -10.90323534495222546, -12.10858216263579124, 57.47290069719868910 ) ) ;
#39476 = VERTEX_POINT ( 'NONE', #2762 ) ;
#39477 = B_SPLINE_CURVE_WITH_KNOTS ( 'NONE', 3,
 ( #40574, #10787, #44787, #6854, #25809, #22358, #40826, #7111, #30975, #8565 ),
 .UNSPECIFIED., .F., .F.,
 ( 4, 2, 2, 2, 4 ),
 ( 0.000000000000000000, 0.2500000000000000000, 0.5000000000000000000, 0.7500000000000000000, 1.000000000000000000 ),
 .UNSPECIFIED. ) ;
#39478 = CARTESIAN_POINT ( 'NONE',  ( -29.92409385541305156, -6.359206544744109735, 52.99999999999997158 ) ) ;
#39479 = DIRECTION ( 'NONE',  ( 9.593247862241308766E-06, 5.650837229295286289E-06, -0.9999999999380186910 ) ) ;
#39480 = EDGE_CURVE ( 'NONE', #12385, #17470, #35893, .T. ) ;
#39481 = CARTESIAN_POINT ( 'NONE',  ( -22.11801487708262215, -20.07437006378957989, 58.76442739134373028 ) ) ;
#39482 = VERTEX_POINT ( 'NONE', #41167 ) ;
#39483 = CARTESIAN_POINT ( 'NONE',  ( -24.72409385541305582, -14.80920654474416764, 63.93529411764704662 ) ) ;
#39484 = ADVANCED_FACE ( 'NONE', ( #32566 ), #33027, .T. ) ;
#39485 = CARTESIAN_POINT ( 'NONE',  ( -10.41686238704247103, -12.27912473904753021, 57.52868529117814234 ) ) ;
#39486 = CARTESIAN_POINT ( 'NONE',  ( -24.30998853687411554, -13.26019858907717897, 66.44679832887018733 ) ) ;
#39487 = CARTESIAN_POINT ( 'NONE',  ( -10.93244803288776090, -12.03909807633519513, 71.24428013274216198 ) ) ;
#39488 = LINE ( 'NONE', #8972, #47227 ) ;
#39489 = VERTEX_POINT ( 'NONE', #47827 ) ;
#39490 = ORIENTED_EDGE ( 'NONE', *, *, #14910, .F. ) ;
#39491 = CARTESIAN_POINT ( 'NONE',  ( -17.68659385541304374, -7.222650657624104298, 49.61879703869476543 ) ) ;
#39492 = CARTESIAN_POINT ( 'NONE',  ( 18.57590614458695200, 2.144561833755798563, 49.27104351578929453 ) ) ;
#39493 = CARTESIAN_POINT ( 'NONE',  ( -14.10937626179043924, -8.137098231162246620, 70.85240724826557823 ) ) ;
#39494 = EDGE_CURVE ( 'NONE', #4523, #4476, #14462, .T. ) ;
#39495 = ADVANCED_FACE ( 'NONE', ( #30592 ), #34749, .T. ) ;
#39496 = DIRECTION ( 'NONE',  ( -0.9410372374137779827, -0.3383029970317210644, -1.029646047569396398E-09 ) ) ;
#39497 = ADVANCED_FACE ( 'NONE', ( #46080, #30351 ), #45850, .T. ) ;
#39498 = CARTESIAN_POINT ( 'NONE',  ( -12.05806040642128707, -10.23620046216302448, 67.51368956197082127 ) ) ;
#39499 = ORIENTED_EDGE ( 'NONE', *, *, #15705, .T. ) ;
#39500 = DIRECTION ( 'NONE',  ( 3.840743001415272461E-07, -4.934726759164745929E-06, 0.9999999999877503543 ) ) ;
#39501 = CARTESIAN_POINT ( 'NONE',  ( -18.19389323530821301, -22.21941482433020809, 65.53027461949925225 ) ) ;
#39502 = VERTEX_POINT ( 'NONE', #57 ) ;
#39503 =( BOUNDED_CURVE ( )  B_SPLINE_CURVE ( 3, ( #7795, #7542, #34105, #6799 ),
 .UNSPECIFIED., .F., .F. ) 
 B_SPLINE_CURVE_WITH_KNOTS ( ( 4, 4 ),
 ( 0.4074455897393655657, 0.5000000000000000000 ),
 .UNSPECIFIED. ) 
 CURVE ( )  GEOMETRIC_REPRESENTATION_ITEM ( )  RATIONAL_B_SPLINE_CURVE ( ( 0.6983129098260920653, 0.7760317562606952047, 0.8765941196519972944, 0.9999999999999966693 ) ) 
 REPRESENTATION_ITEM ( '' )  );
#39504 = CARTESIAN_POINT ( 'NONE',  ( -24.41687585340592648, -14.48898466279928954, 66.48292730085977098 ) ) ;
#39505 = CARTESIAN_POINT ( 'NONE',  ( -12.94846201263913521, -9.425283042519069454, 74.39093336797685652 ) ) ;
#39506 = VERTEX_POINT ( 'NONE', #18754 ) ;
#39507 = CARTESIAN_POINT ( 'NONE',  ( -20.54979434103954361, -8.489990112051950533, 63.61121512946457557 ) ) ;
#39508 = CARTESIAN_POINT ( 'NONE',  ( -18.57780522812731050, -21.71353757645834648, 72.30013330437641628 ) ) ;
#39509 = ORIENTED_EDGE ( 'NONE', *, *, #12475, .F. ) ;
#39510 = DIRECTION ( 'NONE',  ( 0.000000000000000000, 0.9999954153791273948, 0.003028072113819836077 ) ) ;
#39511 = CARTESIAN_POINT ( 'NONE',  ( -22.68646480449111635, -20.08284195570847430, 69.35913425646373298 ) ) ;
#39512 = CARTESIAN_POINT ( 'NONE',  ( -14.25548580596218429, -11.33998781794830535, 52.02966884056656482 ) ) ;
#39513 = CARTESIAN_POINT ( 'NONE',  ( -10.89280197141400919, -11.22507430941316642, 64.33377434530349603 ) ) ;
#39514 = VERTEX_POINT ( 'NONE', #45359 ) ;
#39515 = DIRECTION ( 'NONE',  ( -0.6380325334150320771, 0.7700094066334488563, 0.000000000000000000 ) ) ;
#39516 = FACE_OUTER_BOUND ( 'NONE', #2287, .T. ) ;
#39518 =( BOUNDED_CURVE ( )  B_SPLINE_CURVE ( 3, ( #30755, #22624, #41835, #234 ),
 .UNSPECIFIED., .F., .F. ) 
 B_SPLINE_CURVE_WITH_KNOTS ( ( 4, 4 ),
 ( 0.4074455897393584602, 0.5000000000000000000 ),
 .UNSPECIFIED. ) 
 CURVE ( )  GEOMETRIC_REPRESENTATION_ITEM ( )  RATIONAL_B_SPLINE_CURVE ( ( 0.6983129098260868473, 0.7760317562606771080, 0.8765941196519766443, 0.9999999999999747979 ) ) 
 REPRESENTATION_ITEM ( '' )  );
#39517 = CARTESIAN_POINT ( 'NONE',  ( -24.53780083649505173, -12.59584922708229904, 69.95738295622972203 ) ) ;
#39519 = CARTESIAN_POINT ( 'NONE',  ( -11.96181355942711910, -19.87549434724351727, 58.11177690156993947 ) ) ;
#39520 = FACE_OUTER_BOUND ( 'NONE', #4143, .T. ) ;
#39521 = CARTESIAN_POINT ( 'NONE',  ( -11.47771180081793574, -11.11285131991801478, 60.78958965739695230 ) ) ;
#39522 = CARTESIAN_POINT ( 'NONE',  ( -16.45013838383832550, -21.79965580723203189, 68.83993634381745608 ) ) ;
#39523 = ORIENTED_EDGE ( 'NONE', *, *, #39017, .F. ) ;
#39524 = CARTESIAN_POINT ( 'NONE',  ( -10.45863951484398946, -14.11462368554138536, 60.91821294131582931 ) ) ;
#39525 = CARTESIAN_POINT ( 'NONE',  ( -14.30213453930070244, -8.044712385003874644, 67.39941695810342992 ) ) ;
#39526 = CARTESIAN_POINT ( 'NONE',  ( -21.35673258969864818, -10.96416394607318878, 53.49999999999995026 ) ) ;
#39527 = ORIENTED_EDGE ( 'NONE', *, *, #30292, .F. ) ;
#39528 = DIRECTION ( 'NONE',  ( -4.115385489420004294E-17, -0.9999954153791273948, -0.003028072113811714535 ) ) ;
#39529 = EDGE_CURVE ( 'NONE', #8589, #24799, #11614, .T. ) ;
#39530 = VERTEX_POINT ( 'NONE', #19248 ) ;
#39531 = ORIENTED_EDGE ( 'NONE', *, *, #45569, .F. ) ;
#39532 = ORIENTED_EDGE ( 'NONE', *, *, #29668, .T. ) ;
#39533 = EDGE_CURVE ( 'NONE', #15132, #6650, #4474, .T. ) ;
#39534 = CARTESIAN_POINT ( 'NONE',  ( -15.46331485788676297, -8.033501021233417916, 70.60989570331041421 ) ) ;
#39535 = CARTESIAN_POINT ( 'NONE',  ( -23.11919465953077690, -18.88152036183635119, 65.89559798510001087 ) ) ;
#39536 = CARTESIAN_POINT ( 'NONE',  ( -17.43865353846181421, -7.359098165012483150, 67.19852322307089310 ) ) ;
#39537 = CARTESIAN_POINT ( 'NONE',  ( -17.05968203966123298, -22.25103879409192231, 72.27887915399999486 ) ) ;
#39538 = CARTESIAN_POINT ( 'NONE',  ( -22.91296630721855720, -15.15889098507616950, 54.07175714974879099 ) ) ;
#39539 = ORIENTED_EDGE ( 'NONE', *, *, #7324, .F. ) ;
#39540 = VERTEX_POINT ( 'NONE', #45127 ) ;
#39541 = CARTESIAN_POINT ( 'NONE',  ( -19.40534385650551741, -8.801233750844183135, 48.81488406609782515 ) ) ;
#39542 = CARTESIAN_POINT ( 'NONE',  ( -12.26902364965855519, -19.54473725125994221, 57.92682373989410394 ) ) ;
#39543 = CARTESIAN_POINT ( 'NONE',  ( -16.58751095051766100, -21.80939428823196025, 65.22564390318967753 ) ) ;
#39544 = CARTESIAN_POINT ( 'NONE',  ( -22.21784385650551741, -9.790100578890868377, 49.79778022625163203 ) ) ;
#39545 = EDGE_CURVE ( 'NONE', #34400, #19139, #32633, .T. ) ;
#39546 = ORIENTED_EDGE ( 'NONE', *, *, #39883, .F. ) ;
#39547 = EDGE_CURVE ( 'NONE', #21025, #45248, #20542, .T. ) ;
#39548 = EDGE_CURVE ( 'NONE', #45424, #20159, #46807, .T. ) ;
#39549 = CARTESIAN_POINT ( 'NONE',  ( -24.06787342886325121, -18.28917680027896608, 47.99999999999994316 ) ) ;
#39550 = ADVANCED_FACE ( 'NONE', ( #7697 ), #37448, .T. ) ;
#39551 = PLANE ( 'NONE',  #4865 ) ;
#39552 = DIRECTION ( 'NONE',  ( 3.549360974554993999E-17, -6.371834667797928663E-18, -1.000000000000000000 ) ) ;
#39553 = EDGE_LOOP ( 'NONE', ( #27371, #19988, #30562, #5268, #37872 ) ) ;
#39554 = DIRECTION ( 'NONE',  ( -0.7300417127692488961, -0.6834025882427879894, -6.612978995310452690E-09 ) ) ;
#39555 = B_SPLINE_CURVE_WITH_KNOTS ( 'NONE', 1,
 ( #34524, #26418 ),
 .UNSPECIFIED., .F., .F.,
 ( 2, 2 ),
 ( 0.000000000000000000, 1.000000000000000000 ),
 .UNSPECIFIED. ) ;
#39556 = B_SPLINE_CURVE_WITH_KNOTS ( 'NONE', 3,
 ( #37723, #19263, #34266, #554, #45631, #26909, #23213, #19501, #35716, #8680 ),
 .UNSPECIFIED., .F., .F.,
 ( 4, 2, 2, 2, 4 ),
 ( 0.000000000000000000, 0.2500000000000000000, 0.5000000000000000000, 0.7500000000000000000, 1.000000000000000000 ),
 .UNSPECIFIED. ) ;
#39557 = FACE_OUTER_BOUND ( 'NONE', #13378, .T. ) ;
#39558 = CARTESIAN_POINT ( 'NONE',  ( -45.92409385541305511, -15.80920654474410725, 71.75000000000000000 ) ) ;
#39559 = CARTESIAN_POINT ( 'NONE',  ( -50.42609385541305755, -14.80920654474414810, 61.92352941176469727 ) ) ;
#39560 = AXIS2_PLACEMENT_3D ( 'NONE', #44200, #44426, #41202 ) ;
#39561 = ORIENTED_EDGE ( 'NONE', *, *, #25495, .F. ) ;
#39562 = CYLINDRICAL_SURFACE ( 'NONE', #21071, 0.1499999999999956923 ) ;
#39563 = CARTESIAN_POINT ( 'NONE',  ( -22.85826336087821176, -10.39655209224729226, 63.37185958068533864 ) ) ;
#39564 = DIRECTION ( 'NONE',  ( 0.9687793358424821033, -0.2479245821708677133, 0.000000000000000000 ) ) ;
#39565 = ORIENTED_EDGE ( 'NONE', *, *, #19567, .T. ) ;
#39566 = CARTESIAN_POINT ( 'NONE',  ( -24.43113031232903865, -15.58634216689856622, 73.30303748141028564 ) ) ;
#39567 = ORIENTED_EDGE ( 'NONE', *, *, #37330, .F. ) ;
#39568 = CARTESIAN_POINT ( 'NONE',  ( -14.77890319739905145, -21.35274797201484276, 65.25029445929627059 ) ) ;
#39569 = DIRECTION ( 'NONE',  ( 1.206829990107966821E-05, 1.995688255855010801E-06, 0.9999999999251867333 ) ) ;
#39570 = ORIENTED_EDGE ( 'NONE', *, *, #4077, .T. ) ;
#39571 = CARTESIAN_POINT ( 'NONE',  ( -18.68070144837527735, -7.415226739706411330, 54.27966884056654351 ) ) ;
#39573 = EDGE_CURVE ( 'NONE', #34284, #11137, #34497, .T. ) ;
#39572 = FACE_OUTER_BOUND ( 'NONE', #24173, .T. ) ;
#39574 = CARTESIAN_POINT ( 'NONE',  ( -16.79871736827016449, -7.783984993247369921, 73.84529564069914898 ) ) ;
#39575 = DIRECTION ( 'NONE',  ( 3.549360974554993999E-17, -6.371834667797928663E-18, -1.000000000000000000 ) ) ;
#39576 = ORIENTED_EDGE ( 'NONE', *, *, #15721, .T. ) ;
#39577 = CARTESIAN_POINT ( 'NONE',  ( -10.46253608402116519, -14.07554757472905571, 60.91821325758270689 ) ) ;
#39578 = PRODUCT_DEFINITION_CONTEXT ( 'detailed design', #39119, 'design' ) ;
#39579 = CARTESIAN_POINT ( 'NONE',  ( -42.30718209070717961, -14.80920654474416764, 63.93529411764704662 ) ) ;
#39580 = ORIENTED_EDGE ( 'NONE', *, *, #32645, .F. ) ;
#39581 = CARTESIAN_POINT ( 'NONE',  ( -21.39914427356725213, -17.29159580171669219, 49.52966884056655772 ) ) ;
#39582 = DIRECTION ( 'NONE',  ( 5.517078692044801135E-07, 1.257343604232908019E-06, 0.9999999999990574207 ) ) ;
#39583 = ORIENTED_EDGE ( 'NONE', *, *, #10234, .T. ) ;
#39584 = ORIENTED_EDGE ( 'NONE', *, *, #30149, .T. ) ;
#39585 = CARTESIAN_POINT ( 'NONE',  ( -14.78518025053764440, -21.29286684132125984, 58.16617891046453082 ) ) ;
#39586 = CARTESIAN_POINT ( 'NONE',  ( -23.22909885928854834, -6.086929677699679075, 53.49999999999995026 ) ) ;
#39587 = EDGE_CURVE ( 'NONE', #22244, #42348, #22437, .T. ) ;
#39588 = CARTESIAN_POINT ( 'NONE',  ( -13.55325570056783491, -20.70509005021970594, 57.93161203092463296 ) ) ;
#39589 = CARTESIAN_POINT ( 'NONE',  ( -18.58659385650551599, -9.302874398569244363, 51.68646062012417985 ) ) ;
#39590 = CARTESIAN_POINT ( 'NONE',  ( -24.45201643071094111, -14.25170847814747077, 69.65275273439885950 ) ) ;
#39591 = B_SPLINE_CURVE_WITH_KNOTS ( 'NONE', 3,
 ( #27455, #19335, #34344, #23535, #31147, #45711, #31646, #24022, #16361, #23287 ),
 .UNSPECIFIED., .F., .F.,
 ( 4, 2, 2, 2, 4 ),
 ( 0.6272669072977269389, 0.7522669073147544294, 0.8772669073317820310, 1.002266907348809521, 1.127266907365837012 ),
 .UNSPECIFIED. ) ;
#39592 = CARTESIAN_POINT ( 'NONE',  ( -19.55776627226465791, -21.47609803464143852, 62.10389610901621182 ) ) ;
#39593 = DIRECTION ( 'NONE',  ( 0.3111098983483954195, 0.8385765505603234304, -0.4472135954999584273 ) ) ;
#39594 = DIRECTION ( 'NONE',  ( -3.071710424422018668E-17, 6.404604876783312462E-16, 1.000000000000000000 ) ) ;
#39595 = CARTESIAN_POINT ( 'NONE',  ( -45.92409385541306222, 12.69079345525585545, 70.50000000000000000 ) ) ;
#39596 = VERTEX_POINT ( 'NONE', #27116 ) ;
#39597 = ORIENTED_EDGE ( 'NONE', *, *, #10002, .F. ) ;
#39598 = CARTESIAN_POINT ( 'NONE',  ( -10.91133513969588087, -12.10202850713728218, 74.44351760842475585 ) ) ;
#39599 = DIRECTION ( 'NONE',  ( 1.000000000000000000, 0.000000000000000000, 0.000000000000000000 ) ) ;
#39600 = AXIS2_PLACEMENT_3D ( 'NONE', #44363, #40640, #43638 ) ;
#39601 = CARTESIAN_POINT ( 'NONE',  ( -22.58034385541118994, -9.360768649651129536, 51.01397948904742208 ) ) ;
#39602 = CARTESIAN_POINT ( 'NONE',  ( -11.40217217410143391, -18.47541073860962513, 61.28270649782702151 ) ) ;
#39603 = DIRECTION ( 'NONE',  ( 0.000000000000000000, -0.007114381193220190198, 0.9999746924698832418 ) ) ;
#39604 = DIRECTION ( 'NONE',  ( -3.071710424422018668E-17, 6.404604876783312462E-16, 1.000000000000000000 ) ) ;
#39605 = CARTESIAN_POINT ( 'NONE',  ( -21.45534385650551812, -7.417179338643134834, 52.18511593390279302 ) ) ;
#39606 = ORIENTED_EDGE ( 'NONE', *, *, #38036, .F. ) ;
#39607 = EDGE_CURVE ( 'NONE', #14112, #10001, #22394, .T. ) ;
#39608 = EDGE_CURVE ( 'NONE', #25391, #4116, #43688, .T. ) ;
#39609 = CARTESIAN_POINT ( 'NONE',  ( -45.92409385541306222, 12.69079345525585545, 73.00000000000001421 ) ) ;
#39610 = CARTESIAN_POINT ( 'NONE',  ( 18.07590614458695200, 1.637417875877629436, 51.62951866002712364 ) ) ;
#39611 = CARTESIAN_POINT ( 'NONE',  ( -14.97837282748989729, -8.193824179639600302, 60.73484884663594130 ) ) ;
#39612 = CARTESIAN_POINT ( 'NONE',  ( -11.17472172325445356, -18.86502640884145876, 64.92519864151283571 ) ) ;
#39613 = VERTEX_POINT ( 'NONE', #4720 ) ;
#39614 = CARTESIAN_POINT ( 'NONE',  ( -11.34829033918305718, -18.40080557649748272, 64.89140246238697785 ) ) ;
#39615 = ADVANCED_FACE ( 'NONE', ( #4466 ), #19742, .T. ) ;
#39616 = EDGE_CURVE ( 'NONE', #23182, #1656, #44434, .T. ) ;
#39617 = CARTESIAN_POINT ( 'NONE',  ( -13.65828898514496537, -20.76952646431350757, 65.00101022825411690 ) ) ;
#39618 = CARTESIAN_POINT ( 'NONE',  ( -22.53429319464570924, -9.952421322533329118, 73.48161091678163359 ) ) ;
#39619 = CARTESIAN_POINT ( 'NONE',  ( -18.52416312356643147, -7.896186446804856374, 73.84064402154488960 ) ) ;
#39620 = DIRECTION ( 'NONE',  ( -0.4780674886490096087, 0.8783231047267435754, 5.292596395488305015E-08 ) ) ;
#39621 = CARTESIAN_POINT ( 'NONE',  ( -14.84568658978198563, -7.819606672530345470, 56.95025746631047525 ) ) ;
#39622 = DIRECTION ( 'NONE',  ( -1.077913161506870186E-05, 7.121115479698836302E-06, 0.9999999999165498643 ) ) ;
#39623 = ORIENTED_EDGE ( 'NONE', *, *, #32489, .F. ) ;
#39624 = CARTESIAN_POINT ( 'NONE',  ( -15.49415903819706486, -8.028509590827587417, 74.22985659018391402 ) ) ;
#39625 = VERTEX_POINT ( 'NONE', #47478 ) ;
#39626 = CIRCLE ( 'NONE', #8292, 1.249999999999999556 ) ;
#39627 = CARTESIAN_POINT ( 'NONE',  ( -21.71080454141873517, -9.207639020309585476, 70.22312793020654453 ) ) ;
#39628 = CARTESIAN_POINT ( 'NONE',  ( -17.81164871297510643, -7.369293837194203611, 60.23060767647208280 ) ) ;
#39629 = ORIENTED_EDGE ( 'NONE', *, *, #26456, .F. ) ;
#39630 = CARTESIAN_POINT ( 'NONE',  ( -13.65769536888696223, -21.23707814910688541, 68.56350999071767660 ) ) ;
#39631 = EDGE_CURVE ( 'NONE', #21822, #12832, #34317, .T. ) ;
#39632 = CARTESIAN_POINT ( 'NONE',  ( -13.72409385650551528, -6.426201560718813433, 50.50509628382439331 ) ) ;
#39633 = EDGE_LOOP ( 'NONE', ( #18046, #10037, #11253, #46920, #16431 ) ) ;
#39634 = CARTESIAN_POINT ( 'NONE',  ( -15.12888584993918428, -21.89692032561032775, 68.83238837976321634 ) ) ;
#39635 =( BOUNDED_CURVE ( )  B_SPLINE_CURVE ( 3, ( #45355, #22451, #23188, #15035 ),
 .UNSPECIFIED., .F., .F. ) 
 B_SPLINE_CURVE_WITH_KNOTS ( ( 4, 4 ),
 ( 0.5000000000000000000, 0.9074455897393626236 ),
 .UNSPECIFIED. ) 
 CURVE ( )  GEOMETRIC_REPRESENTATION_ITEM ( )  RATIONAL_B_SPLINE_CURVE ( ( 1.000000000000005107, 0.4567392136813230308, 0.3561768502900233835, 0.6983129098261116052 ) ) 
 REPRESENTATION_ITEM ( '' )  );
#39636 = CARTESIAN_POINT ( 'NONE',  ( -17.65810221059773610, -7.762793303104816189, 63.56529088875731759 ) ) ;
#39637 = LINE ( 'NONE', #27586, #36848 ) ;
#39638 = VERTEX_POINT ( 'NONE', #32214 ) ;
#39639 = DIRECTION ( 'NONE',  ( 3.071710424422018668E-17, -6.404604876783312462E-16, -1.000000000000000000 ) ) ;
#39640 = CYLINDRICAL_SURFACE ( 'NONE', #3894, 2.000000000000000000 ) ;
#39641 = CARTESIAN_POINT ( 'NONE',  ( -23.91010245674826251, -17.57297063409389537, 62.75888927877479517 ) ) ;
#39642 = CARTESIAN_POINT ( 'NONE',  ( -12.99758137947571157, -9.386477775907486887, 71.14925353122600882 ) ) ;
#39643 = EDGE_LOOP ( 'NONE', ( #16511, #4565, #30176, #29319 ) ) ;
#39644 = EDGE_LOOP ( 'NONE', ( #11708, #25174, #30710, #41139, #30747 ) ) ;
#39645 = CARTESIAN_POINT ( 'NONE',  ( -42.04247620835423049, -14.80920654474410547, 66.05294117647058272 ) ) ;
#39646 = CARTESIAN_POINT ( 'NONE',  ( -24.30680323434813062, -16.08559572138876703, 62.87863259089944279 ) ) ;
#39647 = EDGE_LOOP ( 'NONE', ( #7967, #37721 ) ) ;
#39648 = CARTESIAN_POINT ( 'NONE',  ( -15.75283698213507755, -7.548994588147243334, 67.32502552484606895 ) ) ;
#39649 = CARTESIAN_POINT ( 'NONE',  ( -22.09287085128708839, -15.21639644245407119, 52.02966884056656482 ) ) ;
#39650 = CARTESIAN_POINT ( 'NONE',  ( -19.23659385759798823, -8.995762431863214559, 51.38120296130585274 ) ) ;
#39651 = DIRECTION ( 'NONE',  ( 0.1539336739619741601, 0.9880811829098680166, 6.607022902453645889E-08 ) ) ;
#39652 = FACE_OUTER_BOUND ( 'NONE', #28311, .T. ) ;
#39653 = CARTESIAN_POINT ( 'NONE',  ( -15.68875476689939852, -7.563362019294005201, 70.79645224690898431 ) ) ;
#39654 = B_SPLINE_CURVE_WITH_KNOTS ( 'NONE', 3,
 ( #34202, #33966, #30302, #495, #4419, #46281, #45565, #23150, #22915, #11820, #19196, #23382 ),
 .UNSPECIFIED., .F., .F.,
 ( 4, 2, 2, 2, 2, 4 ),
 ( 0.1735808155647264317, 0.3368604174146633268, 0.5001400192646002774, 0.6634196211145371169, 0.7450594220395003742, 0.8266992229644638535 ),
 .UNSPECIFIED. ) ;
#39655 =( BOUNDED_SURFACE ( )  B_SPLINE_SURFACE ( 3, 1, ( 
 ( #44211, #32613 ),
 ( #40256, #47875 ),
 ( #29403, #10460 ),
 ( #32838, #18059 ),
 ( #25467, #39758 ),
 ( #44680, #6520 ),
 ( #21771, #40720 ) ),
 .UNSPECIFIED., .T., .F., .F. ) 
 B_SPLINE_SURFACE_WITH_KNOTS ( ( 4, 3, 4 ),
 ( 2, 2 ),
 ( 0.000000000000000000, 0.5000000000000000000, 1.000000000000000000 ),
 ( 0.000000000000000000, 1.000000000000000000 ),
 .UNSPECIFIED. ) 
 GEOMETRIC_REPRESENTATION_ITEM ( )  RATIONAL_B_SPLINE_SURFACE ( (
 ( 1.000000000000000000, 1.000000000000000000),
 ( 0.3333333333333335369, 0.3333333333333330373),
 ( 0.3333333333333335369, 0.3333333333333330373),
 ( 1.000000000000000000, 1.000000000000000000),
 ( 0.3333333333333333703, 0.3333333333333333703),
 ( 0.3333333333333333703, 0.3333333333333333703),
 ( 1.000000000000000000, 1.000000000000000000) ) ) 
 REPRESENTATION_ITEM ( '' )  SURFACE ( )  );
#39656 = ORIENTED_EDGE ( 'NONE', *, *, #20054, .T. ) ;
#39657 = CARTESIAN_POINT ( 'NONE',  ( -22.83929682888979329, -10.29453308790037980, 66.55654356380499337 ) ) ;
#39658 = CARTESIAN_POINT ( 'NONE',  ( -19.24035349434955577, -7.583912967164861740, 63.68735177183580021 ) ) ;
#39659 = CARTESIAN_POINT ( 'NONE',  ( -12.52591726580351228, -9.195683270288645517, 74.50418291613799227 ) ) ;
#39660 = CARTESIAN_POINT ( 'NONE',  ( -11.16720114480400383, -11.56054632708127627, 67.61864607954859707 ) ) ;
#39661 = VERTEX_POINT ( 'NONE', #20885 ) ;
#39662 =( BOUNDED_CURVE ( )  B_SPLINE_CURVE ( 3, ( #28363, #32299, #2005, #12842 ),
 .UNSPECIFIED., .F., .F. ) 
 B_SPLINE_CURVE_WITH_KNOTS ( ( 4, 4 ),
 ( 1.570796326794896780, 1.780235837034217727 ),
 .UNSPECIFIED. ) 
 CURVE ( )  GEOMETRIC_REPRESENTATION_ITEM ( )  RATIONAL_B_SPLINE_CURVE ( ( 1.000000000000000000, 0.9963479302455154896, 0.9963479302455154896, 1.000000000000000000 ) ) 
 REPRESENTATION_ITEM ( '' )  );
#39663 = AXIS2_PLACEMENT_3D ( 'NONE', #32964, #48010, #21439 ) ;
#39664 = ORIENTED_EDGE ( 'NONE', *, *, #46911, .F. ) ;
#39665 = EDGE_CURVE ( 'NONE', #45314, #32695, #33220, .T. ) ;
#39666 = CARTESIAN_POINT ( 'NONE',  ( -10.88210962122359504, -12.31514282983516750, 57.55687129713847128 ) ) ;
#39667 = AXIS2_PLACEMENT_3D ( 'NONE', #41094, #42317, #8839 ) ;
#39668 = CARTESIAN_POINT ( 'NONE',  ( -20.92409385541305511, -25.10920654474410441, 81.99999999999998579 ) ) ;
#39669 = ORIENTED_EDGE ( 'NONE', *, *, #12709, .T. ) ;
#39670 = DIRECTION ( 'NONE',  ( 0.9687793358424819923, -0.2479245821708680464, 0.000000000000000000 ) ) ;
#39671 = EDGE_CURVE ( 'NONE', #13315, #10765, #9170, .T. ) ;
#39672 = FACE_OUTER_BOUND ( 'NONE', #27637, .T. ) ;
#39673 = ORIENTED_EDGE ( 'NONE', *, *, #48669, .T. ) ;
#39674 = ADVANCED_FACE ( 'NONE', ( #16254 ), #25551, .T. ) ;
#39675 = CARTESIAN_POINT ( 'NONE',  ( -10.96069698787312596, -18.51437578577013809, 57.92219301334858272 ) ) ;
#39676 = CARTESIAN_POINT ( 'NONE',  ( -17.76877443916874810, -21.80232427043311816, 62.06462945740774018 ) ) ;
#39677 = ADVANCED_FACE ( 'NONE', ( #21611 ), #9577, .T. ) ;
#39678 = VERTEX_POINT ( 'NONE', #17420 ) ;
#39679 = CARTESIAN_POINT ( 'NONE',  ( -45.96788223222966963, -14.20318880037429921, 71.05512804915051106 ) ) ;
#39680 = ORIENTED_EDGE ( 'NONE', *, *, #32517, .F. ) ;
#39681 = CARTESIAN_POINT ( 'NONE',  ( -13.51337628678458636, -21.15025853544303303, 65.08605242239845268 ) ) ;
#39682 = ORIENTED_EDGE ( 'NONE', *, *, #36604, .T. ) ;
#39683 = CARTESIAN_POINT ( 'NONE',  ( -11.94538260508191385, -19.85760771564406113, 58.12671156609361134 ) ) ;
#39684 = CARTESIAN_POINT ( 'NONE',  ( -17.97037870217379307, -19.46375863019785513, 52.02966884056656482 ) ) ;
#39685 = CARTESIAN_POINT ( 'NONE',  ( -19.37616744185158879, -21.99900390342548206, 58.71002665166666645 ) ) ;
#39686 = B_SPLINE_CURVE_WITH_KNOTS ( 'NONE', 1,
 ( #30356, #45366 ),
 .UNSPECIFIED., .F., .F.,
 ( 2, 2 ),
 ( 0.000000000000000000, 1.000000000000000000 ),
 .UNSPECIFIED. ) ;
#39687 = ORIENTED_EDGE ( 'NONE', *, *, #30238, .T. ) ;
#39688 = DIRECTION ( 'NONE',  ( -2.866981220435666553E-17, 1.000000000000000000, 1.190614954331866791E-16 ) ) ;
#39689 = DIRECTION ( 'NONE',  ( -1.000000000000000000, 0.000000000000000000, 0.000000000000000000 ) ) ;
#39690 = B_SPLINE_CURVE_WITH_KNOTS ( 'NONE', 1,
 ( #46799, #20462 ),
 .UNSPECIFIED., .F., .F.,
 ( 2, 2 ),
 ( 0.000000000000000000, 1.000000000000000000 ),
 .UNSPECIFIED. ) ;
#39691 = DIRECTION ( 'NONE',  ( -0.9687793358424822143, 0.2479245821708672415, 0.000000000000000000 ) ) ;
#39692 = CARTESIAN_POINT ( 'NONE',  ( -33.52409385541305653, -2.423472813913224222, 48.79999999999998295 ) ) ;
#39693 = DIRECTION ( 'NONE',  ( 2.866981220435666553E-17, -1.000000000000000000, -1.190614954331866791E-16 ) ) ;
#39694 = CARTESIAN_POINT ( 'NONE',  ( -19.14405459605125515, -8.023800501541026975, 60.15196141296932808 ) ) ;
#39695 = ORIENTED_EDGE ( 'NONE', *, *, #9350, .F. ) ;
#39696 = CARTESIAN_POINT ( 'NONE',  ( -17.80887632446114921, -10.12652590253629903, 49.52966884056655772 ) ) ;
#39697 = CARTESIAN_POINT ( 'NONE',  ( -17.23552066371262725, -19.49191114800217406, 49.52966884056656482 ) ) ;
#39698 = DIRECTION ( 'NONE',  ( -0.2466764125338440639, -0.9690979039805150963, 7.162324212089591066E-08 ) ) ;
#39699 = AXIS2_PLACEMENT_3D ( 'NONE', #17887, #39594, #32910 ) ;
#39700 = CARTESIAN_POINT ( 'NONE',  ( -13.24006525392636391, -20.97423447465198976, 61.70301720779925603 ) ) ;
#39701 = DIRECTION ( 'NONE',  ( 1.224646799147353207E-16, 1.000000000000000000, -1.912410701131276611E-32 ) ) ;
#39702 = DIRECTION ( 'NONE',  ( -0.9956360040033419567, 0.09332174201255245827, 0.000000000000000000 ) ) ;
#39703 = CIRCLE ( 'NONE', #36545, 1.249999999999999556 ) ;
#39704 = ORIENTED_EDGE ( 'NONE', *, *, #46856, .F. ) ;
#39705 = CARTESIAN_POINT ( 'NONE',  ( -21.30572535954460633, -21.16897061578360351, 65.69798576082847319 ) ) ;
#39706 = CARTESIAN_POINT ( 'NONE',  ( -24.40844971322602319, -15.79084262311724629, 73.41792560911460441 ) ) ;
#39707 = ORIENTED_EDGE ( 'NONE', *, *, #3689, .T. ) ;
#39708 = CARTESIAN_POINT ( 'NONE',  ( -9.974481508125691676, -14.72588544478808181, 71.37136786695171509 ) ) ;
#39709 = CARTESIAN_POINT ( 'NONE',  ( -15.64104502085146642, -10.46221995643221270, 49.52966884056655772 ) ) ;
#39710 = CARTESIAN_POINT ( 'NONE',  ( -14.49033176393974109, -8.453654632373657662, 63.89864959097710084 ) ) ;
#39711 = CARTESIAN_POINT ( 'NONE',  ( -13.65828898514496359, -20.76952646431350757, 65.00101022825411690 ) ) ;
#39712 = CARTESIAN_POINT ( 'NONE',  ( -10.40127108354264429, -12.32249413655887871, 57.51352655450988749 ) ) ;
#39713 = VERTEX_POINT ( 'NONE', #36596 ) ;
#39714 = B_SPLINE_CURVE_WITH_KNOTS ( 'NONE', 3,
 ( #41655, #22709, #15040, #7694, #4966, #7941, #15523, #26387, #23430, #19003 ),
 .UNSPECIFIED., .F., .F.,
 ( 4, 2, 2, 2, 4 ),
 ( 0.000000000000000000, 0.2500000000000000000, 0.5000000000000000000, 0.7500000000000000000, 1.000000000000000000 ),
 .UNSPECIFIED. ) ;
#39715 = B_SPLINE_CURVE_WITH_KNOTS ( 'NONE', 3,
 ( #41052, #7336, #26036, #21845, #3878, #15169, #7082, #33386, #22840, #22095 ),
 .UNSPECIFIED., .F., .F.,
 ( 4, 2, 2, 2, 4 ),
 ( 0.1272669073658152239, 0.2522669073463065237, 0.3772669073267979067, 0.5022669073072891788, 0.6272669072877805618 ),
 .UNSPECIFIED. ) ;
#39716 = CARTESIAN_POINT ( 'NONE',  ( -36.42409385541304800, -8.109206544743658540, 50.50000000000030553 ) ) ;
#39717 = CARTESIAN_POINT ( 'NONE',  ( -17.20949509180255887, -7.759470163990226155, 74.37506982372057962 ) ) ;
#39718 = LINE ( 'NONE', #47599, #42488 ) ;
#39719 = ORIENTED_EDGE ( 'NONE', *, *, #17244, .T. ) ;
#39720 = LINE ( 'NONE', #48075, #30610 ) ;
#39721 = CARTESIAN_POINT ( 'NONE',  ( -21.96159385541302811, -7.228003583438094459, 51.38655588711988287 ) ) ;
#39722 = DIRECTION ( 'NONE',  ( -0.7364384864160969935, 0.6765045127160409510, 1.031360481960658298E-08 ) ) ;
#39723 = CARTESIAN_POINT ( 'NONE',  ( -22.54890198535468571, -19.65079054415343052, 72.93840789290602800 ) ) ;
#39724 = EDGE_CURVE ( 'NONE', #13505, #34212, #29157, .T. ) ;
#39725 = CARTESIAN_POINT ( 'NONE',  ( -11.05034076241727625, -11.79557573020262318, 71.37388789199357575 ) ) ;
#39726 = CYLINDRICAL_SURFACE ( 'NONE', #1596, 0.1500000000000017153 ) ;
#39727 = VERTEX_POINT ( 'NONE', #13711 ) ;
#39728 = ORIENTED_EDGE ( 'NONE', *, *, #30189, .T. ) ;
#39729 = CARTESIAN_POINT ( 'NONE',  ( -19.43034385541304232, -6.857644439848013640, 49.98602051094139398 ) ) ;
#39730 = CARTESIAN_POINT ( 'NONE',  ( -14.91112529534803066, -8.221969756899694559, 57.13527940342243028 ) ) ;
#39731 = CARTESIAN_POINT ( 'NONE',  ( -15.35027142736847239, -7.653576728715946409, 74.26480947788739684 ) ) ;
#39732 = B_SPLINE_CURVE_WITH_KNOTS ( 'NONE', 1,
 ( #39919, #20731 ),
 .UNSPECIFIED., .F., .F.,
 ( 2, 2 ),
 ( 0.000000000000000000, 1.000000000000000000 ),
 .UNSPECIFIED. ) ;
#39733 = B_SPLINE_CURVE_WITH_KNOTS ( 'NONE', 3,
 ( #22588, #34380, #29733, #33394, #44768, #11019, #37843, #33906, #22340, #26281 ),
 .UNSPECIFIED., .F., .F.,
 ( 4, 2, 2, 2, 4 ),
 ( 0.000000000000000000, 0.2500000000000000000, 0.5000000000000000000, 0.7500000000000000000, 1.000000000000000000 ),
 .UNSPECIFIED. ) ;
#39734 = CARTESIAN_POINT ( 'NONE',  ( -14.15287076785618403, -8.620510619550140419, 70.95631002325610837 ) ) ;
#39735 = DIRECTION ( 'NONE',  ( -0.8037372918934696520, 0.5949843406508664723, 7.322964617522835370E-08 ) ) ;
#39736 = ORIENTED_EDGE ( 'NONE', *, *, #2044, .T. ) ;
#39737 = EDGE_CURVE ( 'NONE', #38388, #12632, #42874, .T. ) ;
#39738 = CARTESIAN_POINT ( 'NONE',  ( -19.29969712032438522, -22.01937259328346741, 58.64790515966043216 ) ) ;
#39739 = DIRECTION ( 'NONE',  ( -0.7800143876985551339, 0.6257615799833393666, -5.505484598862901566E-08 ) ) ;
#39740 = ADVANCED_FACE ( 'NONE', ( #37835 ), #4129, .T. ) ;
#39741 = ORIENTED_EDGE ( 'NONE', *, *, #16596, .T. ) ;
#39742 = CARTESIAN_POINT ( 'NONE',  ( -11.32469277870022850, -18.34471304272907588, 58.10714594244493725 ) ) ;
#39743 = CARTESIAN_POINT ( 'NONE',  ( -12.87691244601553819, -9.487112660658324259, 74.31923044616551977 ) ) ;
#39744 = ORIENTED_EDGE ( 'NONE', *, *, #17217, .T. ) ;
#39745 = EDGE_CURVE ( 'NONE', #15007, #2827, #39715, .T. ) ;
#39746 = LINE ( 'NONE', #36283, #10354 ) ;
#39747 = CARTESIAN_POINT ( 'NONE',  ( -12.17848440243300523, -19.44617680680578786, 57.99852596820085182 ) ) ;
#39748 = ORIENTED_EDGE ( 'NONE', *, *, #14520, .F. ) ;
#39749 = CARTESIAN_POINT ( 'NONE',  ( -23.91467064781584995, -17.58181910956628613, 69.55772506159280510 ) ) ;
#39750 = ADVANCED_FACE ( 'NONE', ( #22579 ), #47280, .T. ) ;
#39751 = CARTESIAN_POINT ( 'NONE',  ( -16.29155950929526497, -19.35680461458998280, 52.02966884056656482 ) ) ;
#39752 = CARTESIAN_POINT ( 'NONE',  ( -22.58346115289088729, -19.54005522229931202, 72.75286664271261827 ) ) ;
#39753 = ORIENTED_EDGE ( 'NONE', *, *, #44807, .F. ) ;
#39754 = CARTESIAN_POINT ( 'NONE',  ( -22.06352460594304787, -8.980016202103444201, 63.37649054182217867 ) ) ;
#39755 = ADVANCED_FACE ( 'NONE', ( #3371 ), #11012, .T. ) ;
#39756 = CARTESIAN_POINT ( 'NONE',  ( -11.91452160938943550, -19.82401263394628543, 58.18328287794685139 ) ) ;
#39757 = CARTESIAN_POINT ( 'NONE',  ( -23.77562434277295367, -17.86939608417919345, 59.01850491586762359 ) ) ;
#39758 = CARTESIAN_POINT ( 'NONE',  ( -11.51414000101334345, -10.27201461766008350, 74.62540520127058130 ) ) ;
#39759 = CARTESIAN_POINT ( 'NONE',  ( -16.23115966991289127, -7.455249367085269974, 60.31533194998537084 ) ) ;
#39760 = CYLINDRICAL_SURFACE ( 'NONE', #22822, 5.249999999999998224 ) ;
#39761 = ORIENTED_EDGE ( 'NONE', *, *, #47257, .F. ) ;
#39762 = CARTESIAN_POINT ( 'NONE',  ( -17.12409385541300111, -9.359200813967566646, 50.49621490985766314 ) ) ;
#39763 = LINE ( 'NONE', #21055, #22689 ) ;
#39764 = PLANE ( 'NONE',  #44001 ) ;
#39765 = EDGE_LOOP ( 'NONE', ( #8590, #16163, #24069, #44229 ) ) ;
#39766 = DIRECTION ( 'NONE',  ( -0.8960627639203775363, 0.4439273849576907960, 5.674307174482189006E-17 ) ) ;
#39767 = VECTOR ( 'NONE', #44396, 1000.000000000000114 ) ;
#39768 = ORIENTED_EDGE ( 'NONE', *, *, #45297, .T. ) ;
#39769 = EDGE_LOOP ( 'NONE', ( #27280, #12949, #42920, #39157, #43430 ) ) ;
#39770 = VERTEX_POINT ( 'NONE', #18619 ) ;
#39771 = APPLICATION_CONTEXT ( 'automotive_design' ) ;
#39772 = CARTESIAN_POINT ( 'NONE',  ( -18.78856086716502816, -7.485212962163699579, 70.47044390587494433 ) ) ;
#39773 = CARTESIAN_POINT ( 'NONE',  ( -23.15062744802226291, -18.83573658997407207, 65.84006125137906906 ) ) ;
#39774 = ADVANCED_FACE ( 'NONE', ( #36840 ), #33634, .T. ) ;
#39775 = CARTESIAN_POINT ( 'NONE',  ( -12.75531685953890459, -14.40201664703460871, 52.02966884056656482 ) ) ;
#39776 = CARTESIAN_POINT ( 'NONE',  ( 18.54465614458695555, 3.140996361033564721, 50.45002501377945947 ) ) ;
#39777 = CARTESIAN_POINT ( 'NONE',  ( -10.72958719098378744, -16.85608497040940534, 57.97144002984030209 ) ) ;
#39778 = EDGE_LOOP ( 'NONE', ( #18901, #7686, #27422, #41521, #21447 ) ) ;
#39779 = ORIENTED_EDGE ( 'NONE', *, *, #47253, .T. ) ;
#39780 = CARTESIAN_POINT ( 'NONE',  ( -19.85534385650552025, -7.417179338643134834, 52.18511593390279302 ) ) ;
#39781 = CARTESIAN_POINT ( 'NONE',  ( -20.78451513435706133, -21.00713107796517320, 62.12943504870421663 ) ) ;
#39782 = CARTESIAN_POINT ( 'NONE',  ( -23.37999588001404661, -18.58199455739222827, 69.57899840282863124 ) ) ;
#39783 =( BOUNDED_SURFACE ( )  B_SPLINE_SURFACE ( 3, 1, ( 
 ( #9122, #8884 ),
 ( #38905, #5185 ),
 ( #39144, #31524 ),
 ( #24388, #20924 ),
 ( #46560, #20449 ),
 ( #35448, #16724 ),
 ( #31766, #13033 ) ),
 .UNSPECIFIED., .T., .F., .F. ) 
 B_SPLINE_SURFACE_WITH_KNOTS ( ( 4, 3, 4 ),
 ( 2, 2 ),
 ( 0.000000000000000000, 0.5000000000000000000, 1.000000000000000000 ),
 ( 0.000000000000000000, 1.000000000000000000 ),
 .UNSPECIFIED. ) 
 GEOMETRIC_REPRESENTATION_ITEM ( )  RATIONAL_B_SPLINE_SURFACE ( (
 ( 1.000000000000000000, 1.000000000000000000),
 ( 0.3333333333333335369, 0.3333333333333330373),
 ( 0.3333333333333335369, 0.3333333333333330373),
 ( 1.000000000000000000, 1.000000000000000000),
 ( 0.3333333333333333703, 0.3333333333333333703),
 ( 0.3333333333333333703, 0.3333333333333333703),
 ( 1.000000000000000000, 1.000000000000000000) ) ) 
 REPRESENTATION_ITEM ( '' )  SURFACE ( )  );
#39784 = CARTESIAN_POINT ( 'NONE',  ( -19.34909385650551883, -8.104110260919579645, 48.81699501597546487 ) ) ;
#39785 = EDGE_CURVE ( 'NONE', #10750, #46952, #24000, .T. ) ;
#39786 = ORIENTED_EDGE ( 'NONE', *, *, #15351, .T. ) ;
#39787 = CARTESIAN_POINT ( 'NONE',  ( -24.37447228737878291, -15.64171875516282384, 69.60595450079478042 ) ) ;
#39788 = CARTESIAN_POINT ( 'NONE',  ( -22.12663539644009703, -20.06189125452669586, 62.52879380229166628 ) ) ;
#39789 = ORIENTED_EDGE ( 'NONE', *, *, #29500, .T. ) ;
#39790 = CARTESIAN_POINT ( 'NONE',  ( -23.08260857892799578, -18.93003297495478776, 62.35406880915004280 ) ) ;
#39791 = B_SPLINE_CURVE_WITH_KNOTS ( 'NONE', 3,
 ( #43896, #2516, #37186, #3471, #21707, #40187, #10867, #17520, #36946, #32548 ),
 .UNSPECIFIED., .F., .F.,
 ( 4, 2, 2, 2, 4 ),
 ( 0.6272669072878258589, 0.7522669073073262602, 0.8772669073268266615, 1.002266907346327063, 1.127266907365827464 ),
 .UNSPECIFIED. ) ;
#39792 =( BOUNDED_CURVE ( )  B_SPLINE_CURVE ( 3, ( #19033, #18785, #42175, #26671 ),
 .UNSPECIFIED., .F., .F. ) 
 B_SPLINE_CURVE_WITH_KNOTS ( ( 4, 4 ),
 ( 0.4074455897393750581, 0.5000000000000000000 ),
 .UNSPECIFIED. ) 
 CURVE ( )  GEOMETRIC_REPRESENTATION_ITEM ( )  RATIONAL_B_SPLINE_CURVE ( ( 0.6983129098261062762, 0.7760317562607026431, 0.8765941196519984047, 0.9999999999999887867 ) ) 
 REPRESENTATION_ITEM ( '' )  );
#39793 = VECTOR ( 'NONE', #31444, 1000.000000000000000 ) ;
#39794 = ORIENTED_EDGE ( 'NONE', *, *, #2032, .F. ) ;
#39795 = EDGE_CURVE ( 'NONE', #1251, #47122, #25663, .T. ) ;
#39796 = CARTESIAN_POINT ( 'NONE',  ( -19.71159385541296061, -8.990409506049296340, 49.61344411288065714 ) ) ;
#39797 = B_SPLINE_CURVE_WITH_KNOTS ( 'NONE', 3,
 ( #12672, #42726, #1103, #24255, #16100, #38771, #39262, #31141, #42235, #8991 ),
 .UNSPECIFIED., .F., .F.,
 ( 4, 2, 2, 2, 4 ),
 ( 0.6272669072877719021, 0.7522669073072933976, 0.8772669073268148932, 1.002266907346336389, 1.127266907365857884 ),
 .UNSPECIFIED. ) ;
#39798 = CARTESIAN_POINT ( 'NONE',  ( -10.27345454978659944, -12.71824136398891980, 64.45331520391344782 ) ) ;
#39799 = CARTESIAN_POINT ( 'NONE',  ( -24.47371109942907808, -14.90716652360855576, 59.25772288469824645 ) ) ;
#39800 = ADVANCED_FACE ( 'NONE', ( #44761 ), #35608, .T. ) ;
#39801 = ORIENTED_EDGE ( 'NONE', *, *, #7016, .T. ) ;
#39802 = DIRECTION ( 'NONE',  ( 1.000000000000000000, 1.669677910507523057E-21, 6.493791346278465266E-22 ) ) ;
#39803 = EDGE_CURVE ( 'NONE', #22946, #15624, #28022, .T. ) ;
#39804 = CARTESIAN_POINT ( 'NONE',  ( -24.47401588851211685, -14.84236380343934769, 59.24300237059242136 ) ) ;
#39805 = PLANE ( 'NONE',  #26853 ) ;
#39806 = VERTEX_POINT ( 'NONE', #38301 ) ;
#39807 = DIRECTION ( 'NONE',  ( -0.9687793358424822143, 0.2479245821708672415, 0.000000000000000000 ) ) ;
#39808 = ORIENTED_EDGE ( 'NONE', *, *, #33178, .T. ) ;
#39809 = CYLINDRICAL_SURFACE ( 'NONE', #22651, 0.1500000000000063782 ) ;
#39810 = LINE ( 'NONE', #31940, #2840 ) ;
#39811 = ORIENTED_EDGE ( 'NONE', *, *, #32918, .F. ) ;
#39812 = DIRECTION ( 'NONE',  ( 0.9687793358424821033, -0.2479245821708677133, 0.000000000000000000 ) ) ;
#39813 = CARTESIAN_POINT ( 'NONE',  ( -21.88020232903564732, -20.20778407762765738, 59.06442927265397458 ) ) ;
#39814 = CARTESIAN_POINT ( 'NONE',  ( -13.38575581802539993, -9.030060914960570173, 60.72478133471773987 ) ) ;
#39815 = FACE_OUTER_BOUND ( 'NONE', #17558, .T. ) ;
#39816 = VERTEX_POINT ( 'NONE', #12459 ) ;
#39817 = CARTESIAN_POINT ( 'NONE',  ( -10.46640841813360900, -14.03671436131648242, 61.20204760743435202 ) ) ;
#39818 = CARTESIAN_POINT ( 'NONE',  ( -14.82998572905333390, -8.253659511465704313, 60.32556042082950398 ) ) ;
#39820 = ADVANCED_FACE ( 'NONE', ( #27725 ), #8072, .F. ) ;
#39819 = CARTESIAN_POINT ( 'NONE',  ( -24.35389707626741185, -16.10709931453380861, 62.87856533165624029 ) ) ;
#39821 = ORIENTED_EDGE ( 'NONE', *, *, #1565, .T. ) ;
#39822 = DIRECTION ( 'NONE',  ( 0.9687793358424821033, -0.2479245821708680464, 0.000000000000000000 ) ) ;
#39823 = EDGE_CURVE ( 'NONE', #3385, #38805, #38559, .T. ) ;
#39824 = CARTESIAN_POINT ( 'NONE',  ( -19.57252240754909067, -21.52402959972952701, 65.47046003899923505 ) ) ;
#39825 = EDGE_CURVE ( 'NONE', #17695, #12464, #8600, .T. ) ;
#39826 = EDGE_CURVE ( 'NONE', #17630, #12655, #29297, .T. ) ;
#39827 = ORIENTED_EDGE ( 'NONE', *, *, #19200, .F. ) ;
#39828 = EDGE_LOOP ( 'NONE', ( #5837, #1453, #35338 ) ) ;
#39829 = CARTESIAN_POINT ( 'NONE',  ( -24.43827367352892210, -15.52193379869737200, 73.28831629023289906 ) ) ;
#39830 = DIRECTION ( 'NONE',  ( -4.115385489419834196E-17, -0.9999954153791273948, -0.003028072113822188795 ) ) ;
#39831 = CARTESIAN_POINT ( 'NONE',  ( -17.91159385650551528, -6.922745924619793101, 51.69366785382590024 ) ) ;
#39832 = CARTESIAN_POINT ( 'NONE',  ( -10.12358845859998624, -13.32384912816304556, 74.72171712345732431 ) ) ;
#39833 = CARTESIAN_POINT ( 'NONE',  ( -23.52949419687348964, -11.28347464189849703, 70.17738639980606763 ) ) ;
#39834 = CARTESIAN_POINT ( 'NONE',  ( -23.08260857892799578, -18.93003297495478776, 62.35406880915004280 ) ) ;
#39835 = CARTESIAN_POINT ( 'NONE',  ( -13.11718577119540718, -9.290850031293775402, 67.37942741453835538 ) ) ;
#39836 = CARTESIAN_POINT ( 'NONE',  ( -13.90059129645203662, -21.37345143546091819, 72.10324577624415099 ) ) ;
#39837 = CIRCLE ( 'NONE', #21002, 2.000000000000001332 ) ;
#39838 = AXIS2_PLACEMENT_3D ( 'NONE', #33704, #29802, #32976 ) ;
#39839 = ORIENTED_EDGE ( 'NONE', *, *, #21021, .F. ) ;
#39840 = EDGE_LOOP ( 'NONE', ( #34442, #37336, #39109, #12261, #4377, #27295, #39254, #32688 ) ) ;
#39841 = CARTESIAN_POINT ( 'NONE',  ( -10.44997270537017897, -15.86517854522099391, 61.24608883751315602 ) ) ;
#39842 = CARTESIAN_POINT ( 'NONE',  ( -23.61204096558246235, -11.53669824655086451, 66.72214514747398084 ) ) ;
#39843 = CARTESIAN_POINT ( 'NONE',  ( -15.96294676038700899, -7.962953527514619267, 67.15623976804144490 ) ) ;
#39844 = CARTESIAN_POINT ( 'NONE',  ( -21.31115985637654120, -8.927249709250720144, 73.88656608925673197 ) ) ;
#39845 = AXIS2_PLACEMENT_3D ( 'NONE', #46476, #19884, #42539 ) ;
#39846 = CARTESIAN_POINT ( 'NONE',  ( -17.92193097897700227, -21.84160713959417066, 62.17535923543130849 ) ) ;
#39847 = CARTESIAN_POINT ( 'NONE',  ( -20.10534385650551670, -8.801233750844183135, 48.81488406609782515 ) ) ;
#39848 = ORIENTED_EDGE ( 'NONE', *, *, #36939, .F. ) ;
#39849 = EDGE_CURVE ( 'NONE', #31686, #19851, #11991, .T. ) ;
#39850 = CARTESIAN_POINT ( 'NONE',  ( -10.66703313327717417, -12.79807994555918960, 64.56836111017611302 ) ) ;
#39851 = CARTESIAN_POINT ( 'NONE',  ( -21.68202464530013529, -12.85132308587069794, 49.52966884056655772 ) ) ;
#39852 = DIRECTION ( 'NONE',  ( -0.4251432040024066272, -0.9051260995521939190, -1.185120001106687566E-09 ) ) ;
#39853 = CARTESIAN_POINT ( 'NONE',  ( -35.42409385541304800, -9.159201730891741278, 50.49682052428079970 ) ) ;
#39854 = VERTEX_POINT ( 'NONE', #8297 ) ;
#39855 = ADVANCED_FACE ( 'NONE', ( #1367 ), #23312, .T. ) ;
#39856 = CARTESIAN_POINT ( 'NONE',  ( -10.56627859465609376, -16.21290490039525167, 71.44750383612122846 ) ) ;
#39857 = CARTESIAN_POINT ( 'NONE',  ( -17.58536440216138885, -7.758048768718602162, 59.96572088198239214 ) ) ;
#39858 = EDGE_CURVE ( 'NONE', #10228, #4125, #15660, .T. ) ;
#39859 = DIRECTION ( 'NONE',  ( 0.9687793358424819923, -0.2479245821708678243, 0.000000000000000000 ) ) ;
#39860 = DIRECTION ( 'NONE',  ( 2.081668171172170091E-15, 0.000000000000000000, -1.000000000000000000 ) ) ;
#39861 = ORIENTED_EDGE ( 'NONE', *, *, #16565, .T. ) ;
#39862 = FACE_OUTER_BOUND ( 'NONE', #27046, .T. ) ;
#39863 = CIRCLE ( 'NONE', #15485, 4.686499999999998778 ) ;
#39864 = AXIS2_PLACEMENT_3D ( 'NONE', #24476, #46635, #39479 ) ;
#39865 = ORIENTED_EDGE ( 'NONE', *, *, #46719, .T. ) ;
#39866 = CARTESIAN_POINT ( 'NONE',  ( -45.37196614242555626, -14.20920654474410760, 70.13000000000000966 ) ) ;
#39867 = CARTESIAN_POINT ( 'NONE',  ( -10.22954393756624114, -12.87502507475396918, 67.93843551393385383 ) ) ;
#39868 = EDGE_LOOP ( 'NONE', ( #22724, #6370, #17414, #25247, #29919 ) ) ;
#39869 = CARTESIAN_POINT ( 'NONE',  ( -13.72515530044423393, -21.27626469894021355, 68.59478590258110842 ) ) ;
#39870 = FACE_OUTER_BOUND ( 'NONE', #23130, .T. ) ;
#39871 = ORIENTED_EDGE ( 'NONE', *, *, #42471, .F. ) ;
#39872 = CARTESIAN_POINT ( 'NONE',  ( -24.47217469005613211, -14.64471752244937441, 62.71296487297676947 ) ) ;
#39873 = VECTOR ( 'NONE', #48328, 1000.000000000000000 ) ;
#39874 = CARTESIAN_POINT ( 'NONE',  ( -6.424093855413055110, -27.10920654474410796, 81.99999999999998579 ) ) ;
#39875 = CARTESIAN_POINT ( 'NONE',  ( -14.71758685070772366, -21.32224385381664788, 62.05089037315948275 ) ) ;
#39876 = ORIENTED_EDGE ( 'NONE', *, *, #5398, .T. ) ;
#39877 = CARTESIAN_POINT ( 'NONE',  ( -18.68070144837527735, -7.415226739706411330, 53.49999999999994316 ) ) ;
#39878 = EDGE_CURVE ( 'NONE', #37416, #31355, #8533, .T. ) ;
#39879 = CARTESIAN_POINT ( 'NONE',  ( -10.96069643151774109, -18.51437482595545347, 57.92219192461608657 ) ) ;
#39880 = DIRECTION ( 'NONE',  ( -1.000000000000000000, -1.669677910507523057E-21, -6.493791346278465266E-22 ) ) ;
#39881 = DIRECTION ( 'NONE',  ( 0.9687793358424819923, -0.2479245821708680464, 0.000000000000000000 ) ) ;
#39882 = EDGE_CURVE ( 'NONE', #27105, #36936, #5724, .T. ) ;
#39883 = EDGE_CURVE ( 'NONE', #17695, #31311, #16633, .T. ) ;
#39884 = VERTEX_POINT ( 'NONE', #46202 ) ;
#39885 = ORIENTED_EDGE ( 'NONE', *, *, #9691, .T. ) ;
#39886 = B_SPLINE_CURVE_WITH_KNOTS ( 'NONE', 3,
 ( #40646, #26621, #26368, #11353, #18986, #763, #4950, #41383, #4447, #22944 ),
 .UNSPECIFIED., .F., .F.,
 ( 4, 2, 2, 2, 4 ),
 ( 0.1272669073658213301, 0.2522669073463013611, 0.3772669073267813644, 0.5022669073072614232, 0.6272669072877414820 ),
 .UNSPECIFIED. ) ;
#39887 = FACE_OUTER_BOUND ( 'NONE', #9503, .T. ) ;
#39888 = CARTESIAN_POINT ( 'NONE',  ( -24.31965416599553720, -16.01388414632039314, 62.70214577705259273 ) ) ;
#39889 = ORIENTED_EDGE ( 'NONE', *, *, #44678, .F. ) ;
#39890 = CARTESIAN_POINT ( 'NONE',  ( -20.76545062400256825, -8.150403215067090201, 63.48934267039048507 ) ) ;
#39891 = CARTESIAN_POINT ( 'NONE',  ( -17.94284385759799605, -7.587656875400192291, 49.25157356644813689 ) ) ;
#39892 = CARTESIAN_POINT ( 'NONE',  ( -40.92409385541305511, -14.80920654474410725, 74.99999999999998579 ) ) ;
#39893 = CARTESIAN_POINT ( 'NONE',  ( -11.85162103594838001, -10.49015045520576983, 71.25420998615621215 ) ) ;
#39894 = CARTESIAN_POINT ( 'NONE',  ( -20.57971641534515328, -8.060397143422079580, 66.90387173718066549 ) ) ;
#39895 = VERTEX_POINT ( 'NONE', #42517 ) ;
#39896 = EDGE_CURVE ( 'NONE', #47432, #15891, #46451, .T. ) ;
#39897 = ADVANCED_FACE ( 'NONE', ( #23808 ), #31420, .T. ) ;
#39898 = CARTESIAN_POINT ( 'NONE',  ( -24.22092332596094977, -12.93687947476191269, 66.45246741375130739 ) ) ;
#39899 = CARTESIAN_POINT ( 'NONE',  ( -20.70232273485035890, -8.624288160964143302, 60.14125250309182036 ) ) ;
#39900 = CARTESIAN_POINT ( 'NONE',  ( -12.65882755920527458, -9.609488432089360543, 74.20434181795738482 ) ) ;
#39901 = CARTESIAN_POINT ( 'NONE',  ( -21.10164091802717223, -17.71419016815048764, 52.02966884056656482 ) ) ;
#39902 = VECTOR ( 'NONE', #23871, 1000.000000000000000 ) ;
#39903 = ORIENTED_EDGE ( 'NONE', *, *, #16268, .F. ) ;
#39904 = VECTOR ( 'NONE', #455, 1000.000000000000114 ) ;
#39905 = VERTEX_POINT ( 'NONE', #16865 ) ;
#39906 = ADVANCED_FACE ( 'NONE', ( #6290 ), #47577, .F. ) ;
#39907 = CARTESIAN_POINT ( 'NONE',  ( -24.87123163304818974, -14.59964195235338735, 62.89791815715346956 ) ) ;
#39908 = CARTESIAN_POINT ( 'NONE',  ( -23.70135507383723805, -11.71146680393053607, 62.95218278684509983 ) ) ;
#39909 = B_SPLINE_CURVE_WITH_KNOTS ( 'NONE', 3,
 ( #46387, #31845, #46634, #20761, #27419, #35761, #42452, #27905, #23749, #23983 ),
 .UNSPECIFIED., .F., .F.,
 ( 4, 2, 2, 2, 4 ),
 ( 0.6272669072878050978, 0.7522669073073239288, 0.8772669073268426487, 1.002266907346361480, 1.127266907365880311 ),
 .UNSPECIFIED. ) ;
#39910 = CARTESIAN_POINT ( 'NONE',  ( -11.42962470904260464, -10.38539412368214521, 74.62380407152070916 ) ) ;
#39911 = AXIS2_PLACEMENT_3D ( 'NONE', #30752, #1172, #38112 ) ;
#39912 = ORIENTED_EDGE ( 'NONE', *, *, #40980, .T. ) ;
#39913 = LINE ( 'NONE', #21685, #40774 ) ;
#39914 = CARTESIAN_POINT ( 'NONE',  ( -12.97018521796328017, -9.340428432532196013, 74.73411830381819243 ) ) ;
#39915 = ORIENTED_EDGE ( 'NONE', *, *, #17147, .T. ) ;
#39916 = CARTESIAN_POINT ( 'NONE',  ( -10.61357140615669792, -13.19155887971477448, 71.50828586566468914 ) ) ;
#39917 = CARTESIAN_POINT ( 'NONE',  ( -12.93804115531433396, -9.435551541445537538, 70.86427763179355566 ) ) ;
#39918 =( BOUNDED_CURVE ( )  B_SPLINE_CURVE ( 3, ( #41161, #38178, #11607, #15279 ),
 .UNSPECIFIED., .F., .F. ) 
 B_SPLINE_CURVE_WITH_KNOTS ( ( 4, 4 ),
 ( 0.9074455897393652881, 1.000000000000000000 ),
 .UNSPECIFIED. ) 
 CURVE ( )  GEOMETRIC_REPRESENTATION_ITEM ( )  RATIONAL_B_SPLINE_CURVE ( ( 0.6983129098261124934, 0.7760317562607149666, 0.8765941196520108392, 1.000000000000000000 ) ) 
 REPRESENTATION_ITEM ( '' )  );
#39919 = CARTESIAN_POINT ( 'NONE',  ( -12.05806040642128707, -10.23620046216302448, 67.51368956197082127 ) ) ;
#39920 = ORIENTED_EDGE ( 'NONE', *, *, #12145, .T. ) ;
#39921 = LINE ( 'NONE', #45584, #8667 ) ;
#39922 = VERTEX_POINT ( 'NONE', #13888 ) ;
#39923 = CARTESIAN_POINT ( 'NONE',  ( -14.20982686782564386, -8.534409222511607496, 71.02397852537180256 ) ) ;
#39924 = DIRECTION ( 'NONE',  ( -0.9466432954593471116, -0.3222832157619556770, -8.771047023603929338E-09 ) ) ;
#39925 = CARTESIAN_POINT ( 'NONE',  ( -18.16442973052015830, -21.82037594034854422, 65.63972370452951566 ) ) ;
#39926 = ORIENTED_EDGE ( 'NONE', *, *, #40432, .T. ) ;
#39927 = DIRECTION ( 'NONE',  ( -3.071710424422018668E-17, 6.404604876783312462E-16, 1.000000000000000000 ) ) ;
#39928 = CARTESIAN_POINT ( 'NONE',  ( -20.17342227129689292, -21.73347691371985846, 72.52666002253516808 ) ) ;
#39929 = FACE_OUTER_BOUND ( 'NONE', #46375, .T. ) ;
#39930 = VECTOR ( 'NONE', #23775, 1000.000000000000114 ) ;
#39931 = CARTESIAN_POINT ( 'NONE',  ( -13.62948724496060215, -8.926948417807865965, 57.26967755883410405 ) ) ;
#39932 = CARTESIAN_POINT ( 'NONE',  ( -10.47299162366406478, -15.63514707757639854, 61.33789045486464886 ) ) ;
#39933 = DIRECTION ( 'NONE',  ( -3.071710424422018668E-17, 6.404604876783312462E-16, 1.000000000000000000 ) ) ;
#39934 = EDGE_LOOP ( 'NONE', ( #9788, #1809, #37696, #38626 ) ) ;
#39936 = CARTESIAN_POINT ( 'NONE',  ( -36.42409385541304800, -9.359200813967566646, 50.49621490985803263 ) ) ;
#39935 =( BOUNDED_CURVE ( )  B_SPLINE_CURVE ( 3, ( #46945, #43270, #9288, #39799 ),
 .UNSPECIFIED., .F., .F. ) 
 B_SPLINE_CURVE_WITH_KNOTS ( ( 4, 4 ),
 ( 0.4074455897393629566, 0.5000000000000000000 ),
 .UNSPECIFIED. ) 
 CURVE ( )  GEOMETRIC_REPRESENTATION_ITEM ( )  RATIONAL_B_SPLINE_CURVE ( ( 0.6983129098260936196, 0.7760317562607117470, 0.8765941196520176115, 1.000000000000020650 ) ) 
 REPRESENTATION_ITEM ( '' )  );
#39937 = AXIS2_PLACEMENT_3D ( 'NONE', #11293, #18412, #14693 ) ;
#39938 = VECTOR ( 'NONE', #4099, 999.9999999999998863 ) ;
#39939 = CARTESIAN_POINT ( 'NONE',  ( -17.00889379717436611, -21.85058792022787699, 68.90380497144548144 ) ) ;
#39940 = CARTESIAN_POINT ( 'NONE',  ( -46.29409385541305255, -13.72754205882879042, 70.96013658682592506 ) ) ;
#39941 = CARTESIAN_POINT ( 'NONE',  ( -17.42409385541299471, -14.80920654474435771, 49.52966884056655772 ) ) ;
#39942 = CYLINDRICAL_SURFACE ( 'NONE', #17213, 0.1500000000000017708 ) ;
#39943 = CARTESIAN_POINT ( 'NONE',  ( -13.69284385650552061, -7.406986770994972602, 48.81910596585309747 ) ) ;
#39944 = EDGE_CURVE ( 'NONE', #25463, #744, #28730, .T. ) ;
#39945 = ORIENTED_EDGE ( 'NONE', *, *, #30903, .T. ) ;
#39946 = ORIENTED_EDGE ( 'NONE', *, *, #43703, .F. ) ;
#39947 = DIRECTION ( 'NONE',  ( -0.9974380310868017352, -0.07153582418399355436, 3.008056591778321396E-08 ) ) ;
#39948 = FACE_OUTER_BOUND ( 'NONE', #33777, .T. ) ;
#39949 = VERTEX_POINT ( 'NONE', #13651 ) ;
#39950 = CARTESIAN_POINT ( 'NONE',  ( -42.05571150247188683, -14.80920654474419074, 65.94705882352940307 ) ) ;
#39952 = CARTESIAN_POINT ( 'NONE',  ( -13.49909385650551563, -8.114302828567740988, 52.18300498402516041 ) ) ;
#39951 = CARTESIAN_POINT ( 'NONE',  ( -10.45004451964941872, -15.89438299218807771, 71.59183561948579211 ) ) ;
#39953 = CARTESIAN_POINT ( 'NONE',  ( -11.61616642816477807, -18.80577669094758164, 68.22249455738848667 ) ) ;
#39954 = CIRCLE ( 'NONE', #29721, 1.999999999999999556 ) ;
#39955 = CARTESIAN_POINT ( 'NONE',  ( -16.24320552860936928, -21.75975297682954945, 58.58025747933638172 ) ) ;
#39956 = VERTEX_POINT ( 'NONE', #31907 ) ;
#39957 = FACE_BOUND ( 'NONE', #16345, .T. ) ;
#39958 = AXIS2_PLACEMENT_3D ( 'NONE', #19537, #27656, #831 ) ;
#39959 = DIRECTION ( 'NONE',  ( -0.000000000000000000, -1.000000000000000000, -0.000000000000000000 ) ) ;
#39960 = CYLINDRICAL_SURFACE ( 'NONE', #9994, 0.1500000000000019651 ) ;
#39961 = EDGE_CURVE ( 'NONE', #29649, #43613, #46924, .T. ) ;
#39962 = EDGE_CURVE ( 'NONE', #39384, #21434, #7988, .T. ) ;
#39963 = CARTESIAN_POINT ( 'NONE',  ( -20.69509252757554307, -8.115601716887088202, 63.49616818922779515 ) ) ;
#39964 = ORIENTED_EDGE ( 'NONE', *, *, #17024, .T. ) ;
#39965 = CARTESIAN_POINT ( 'NONE',  ( -11.64902330566212463, -10.02396254413167576, 53.49999999999994316 ) ) ;
#39966 =( NAMED_UNIT ( * ) SI_UNIT ( $, .STERADIAN. ) SOLID_ANGLE_UNIT ( ) );
#39967 = EDGE_CURVE ( 'NONE', #27510, #20955, #28931, .T. ) ;
#39968 = EDGE_CURVE ( 'NONE', #7647, #12505, #20871, .T. ) ;
#39969 = CARTESIAN_POINT ( 'NONE',  ( -13.25446207031254886, -8.635133168339066856, 60.57916952436288227 ) ) ;
#39970 = CARTESIAN_POINT ( 'NONE',  ( -13.73970969606274473, -20.76112332560825990, 65.28628881671112083 ) ) ;
#39971 = CARTESIAN_POINT ( 'NONE',  ( -11.52367759983210149, -11.04269222737732470, 57.50903262756441592 ) ) ;
#39972 = ORIENTED_EDGE ( 'NONE', *, *, #18486, .T. ) ;
#39973 = VERTEX_POINT ( 'NONE', #36537 ) ;
#39974 = CARTESIAN_POINT ( 'NONE',  ( -17.96784385541304374, -9.357632978295830739, 49.97845033065684106 ) ) ;
#39975 = EDGE_CURVE ( 'NONE', #46413, #28927, #31668, .T. ) ;
#39976 = CARTESIAN_POINT ( 'NONE',  ( -10.85841931818429629, -17.37798394237198707, 64.91267318220633342 ) ) ;
#39977 = VECTOR ( 'NONE', #14106, 1000.000000000000000 ) ;
#39978 = CYLINDRICAL_SURFACE ( 'NONE', #23730, 0.1500000000000006051 ) ;
#39979 = VECTOR ( 'NONE', #24595, 1000.000000000000000 ) ;
#39980 = AXIS2_PLACEMENT_3D ( 'NONE', #29900, #10459, #29645 ) ;
#39981 = AXIS2_PLACEMENT_3D ( 'NONE', #3594, #26749, #11239 ) ;
#39982 = CARTESIAN_POINT ( 'NONE',  ( -15.43264099835366565, -7.630132484668774140, 74.24132189675523819 ) ) ;
#39983 = ORIENTED_EDGE ( 'NONE', *, *, #21291, .F. ) ;
#39984 = CARTESIAN_POINT ( 'NONE',  ( -10.98866448286933029, -11.05551018869101298, 60.81739231005553847 ) ) ;
#39985 = VECTOR ( 'NONE', #47395, 1000.000000000000227 ) ;
#39986 = CARTESIAN_POINT ( 'NONE',  ( -22.05805477923917124, -20.12249178580863784, 62.23998944766726282 ) ) ;
#39987 = ORIENTED_EDGE ( 'NONE', *, *, #45361, .F. ) ;
#39988 = CARTESIAN_POINT ( 'NONE',  ( -27.42409385541305156, -15.80920654474410725, 47.99999999999997868 ) ) ;
#39989 = B_SPLINE_CURVE_WITH_KNOTS ( 'NONE', 3,
 ( #32311, #47335, #13565, #28611, #39928, #6201, #7672, #7423, #26364, #22677 ),
 .UNSPECIFIED., .F., .F.,
 ( 4, 2, 2, 2, 4 ),
 ( 0.6272669072974624838, 0.7522669073145729079, 0.8772669073316834432, 1.002266907348793978, 1.127266907365904292 ),
 .UNSPECIFIED. ) ;
#39990 = CARTESIAN_POINT ( 'NONE',  ( -14.69606858684902306, -21.31402952851196986, 61.93600410282152779 ) ) ;
#39991 = ORIENTED_EDGE ( 'NONE', *, *, #18753, .F. ) ;
#39992 = CYLINDRICAL_SURFACE ( 'NONE', #48048, 0.5000000000000004441 ) ;
#39993 = CARTESIAN_POINT ( 'NONE',  ( -18.54257441268414297, -21.71939603377284911, 72.58510895925300588 ) ) ;
#39994 = ORIENTED_EDGE ( 'NONE', *, *, #38328, .F. ) ;
#39995 = CARTESIAN_POINT ( 'NONE',  ( -17.93190708896392493, -21.84390349538901077, 58.29064763788917958 ) ) ;
#39996 = CARTESIAN_POINT ( 'NONE',  ( -23.40706900507760224, -18.44293855997280929, 73.06368236814604700 ) ) ;
#39997 = EDGE_CURVE ( 'NONE', #47492, #24829, #10321, .T. ) ;
#39998 = CARTESIAN_POINT ( 'NONE',  ( -15.27707121964805381, -8.090297697211889627, 74.28805465071215508 ) ) ;
#39999 = CARTESIAN_POINT ( 'NONE',  ( -22.48114071483173149, -19.64927648862363796, 72.94400547034429394 ) ) ;
#40000 = ORIENTED_EDGE ( 'NONE', *, *, #45972, .T. ) ;
#40001 = CARTESIAN_POINT ( 'NONE',  ( -10.38243336603528277, -15.21964919048783393, 57.65972899058709800 ) ) ;
#40002 = CARTESIAN_POINT ( 'NONE',  ( -24.14679772577363437, -12.68507108172156883, 70.05770892828130059 ) ) ;
#40003 = CARTESIAN_POINT ( 'NONE',  ( -20.51116909090755769, -10.56274136881318348, 52.02966884056656482 ) ) ;
#40004 = ITEM_DEFINED_TRANSFORMATION ( 'NONE', 'NONE', #43184,  #29031 ) ;
#40005 = CARTESIAN_POINT ( 'NONE',  ( -20.06975372951847447, -8.274133229585533655, 73.73568642813194174 ) ) ;
#40006 = CARTESIAN_POINT ( 'NONE',  ( -22.13034385650551883, -9.794322478646142471, 51.19202720610083190 ) ) ;
#40007 = ADVANCED_FACE ( 'NONE', ( #5814 ), #2104, .T. ) ;
#40008 = AXIS2_PLACEMENT_3D ( 'NONE', #7990, #23003, #37747 ) ;
#40009 = CARTESIAN_POINT ( 'NONE',  ( -50.42609385541305755, -14.90920654474419038, 65.04705882352939739 ) ) ;
#40010 = DIRECTION ( 'NONE',  ( -3.892913453477729145E-06, -4.639959647628106577E-06, -0.9999999999816580054 ) ) ;
#40011 = ORIENTED_EDGE ( 'NONE', *, *, #14859, .T. ) ;
#40012 = CARTESIAN_POINT ( 'NONE',  ( -10.69339011031838105, -12.88606202777132914, 64.55370748154987837 ) ) ;
#40013 = AXIS2_PLACEMENT_3D ( 'NONE', #20474, #38931, #5211 ) ;
#40014 = CARTESIAN_POINT ( 'NONE',  ( -14.28136839270488423, -8.054466369743188636, 67.45313376895239799 ) ) ;
#40015 = CARTESIAN_POINT ( 'NONE',  ( -10.00048885941320087, -15.43727575513289629, 57.69075912652810700 ) ) ;
#40016 = ORIENTED_EDGE ( 'NONE', *, *, #20237, .F. ) ;
#40017 = DIRECTION ( 'NONE',  ( -3.071710424422018668E-17, 6.404604876783312462E-16, 1.000000000000000000 ) ) ;
#40018 = VECTOR ( 'NONE', #32779, 1000.000000000000000 ) ;
#40019 = CONICAL_SURFACE ( 'NONE', #14032, 0.5560000000000009379, 0.06981317007976595157 ) ;
#40020 = B_SPLINE_CURVE_WITH_KNOTS ( 'NONE', 3,
 ( #2648, #21130, #10761, #6828, #10530, #17886, #44510, #13476, #29479, #6102 ),
 .UNSPECIFIED., .F., .F.,
 ( 4, 2, 2, 2, 4 ),
 ( 0.000000000000000000, 0.2500000000000000000, 0.5000000000000000000, 0.7500000000000000000, 1.000000000000000000 ),
 .UNSPECIFIED. ) ;
#40021 = ORIENTED_EDGE ( 'NONE', *, *, #40454, .T. ) ;
#40022 = ORIENTED_EDGE ( 'NONE', *, *, #7906, .T. ) ;
#40023 = EDGE_LOOP ( 'NONE', ( #3069, #25010, #48172, #29415 ) ) ;
#40024 = EDGE_CURVE ( 'NONE', #21408, #8478, #48371, .T. ) ;
#40025 = CARTESIAN_POINT ( 'NONE',  ( -15.62222905942471840, -7.993050613273783966, 70.89517703929612935 ) ) ;
#40026 = AXIS2_PLACEMENT_3D ( 'NONE', #36108, #13694, #28739 ) ;
#40027 = EDGE_CURVE ( 'NONE', #8571, #25, #13602, .T. ) ;
#40028 = CARTESIAN_POINT ( 'NONE',  ( -12.90958250904497362, -8.882692446305687994, 67.50225915842231927 ) ) ;
#40029 = CARTESIAN_POINT ( 'NONE',  ( -22.79734351242366941, -10.24514170768878962, 66.69182257473532616 ) ) ;
#40030 = CARTESIAN_POINT ( 'NONE',  ( -13.12535629923256941, -9.217633289312832545, 71.26414145609075490 ) ) ;
#40031 = ORIENTED_EDGE ( 'NONE', *, *, #38220, .T. ) ;
#40032 = ORIENTED_EDGE ( 'NONE', *, *, #18820, .T. ) ;
#40033 = EDGE_CURVE ( 'NONE', #6071, #20751, #32628, .T. ) ;
#40034 = CARTESIAN_POINT ( 'NONE',  ( -18.33659385650551243, -6.915538690918075382, 49.31353937987644542 ) ) ;
#40035 = DIRECTION ( 'NONE',  ( 0.3047757271037812021, -0.9524197806957002133, -0.002884009000665106303 ) ) ;
#40036 = CARTESIAN_POINT ( 'NONE',  ( -40.92409385541305511, -25.10920654474410441, 74.99999999999998579 ) ) ;
#40037 = EDGE_CURVE ( 'NONE', #37693, #26590, #29181, .T. ) ;
#40038 = CARTESIAN_POINT ( 'NONE',  ( -19.57409385650551670, -9.792211528768504536, 50.49490371617623197 ) ) ;
#40039 = ORIENTED_EDGE ( 'NONE', *, *, #21275, .F. ) ;
#40040 = DIRECTION ( 'NONE',  ( 1.000000000000000000, -0.000000000000000000, -2.406186529621654511E-16 ) ) ;
#40041 = AXIS2_PLACEMENT_3D ( 'NONE', #44620, #17759, #40661 ) ;
#40042 = CARTESIAN_POINT ( 'NONE',  ( -24.78816760170556677, -15.94238017617776215, 69.71962869939886787 ) ) ;
#40043 = ORIENTED_EDGE ( 'NONE', *, *, #18878, .T. ) ;
#40044 = CARTESIAN_POINT ( 'NONE',  ( -11.28069604468732479, -11.45046212628238358, 67.80791698215925578 ) ) ;
#40045 = ORIENTED_EDGE ( 'NONE', *, *, #43989, .F. ) ;
#40046 = CARTESIAN_POINT ( 'NONE',  ( -45.92409385541306222, 12.69079345525585545, 70.50000000000000000 ) ) ;
#40047 = DIRECTION ( 'NONE',  ( 0.000000000000000000, 0.000000000000000000, 1.000000000000000000 ) ) ;
#40048 = CARTESIAN_POINT ( 'NONE',  ( -14.42215129996211154, -7.990733167546266280, 63.89640551974409988 ) ) ;
#40049 = ORIENTED_EDGE ( 'NONE', *, *, #14465, .T. ) ;
#40050 = VECTOR ( 'NONE', #23973, 1000.000000000000000 ) ;
#40051 = CARTESIAN_POINT ( 'NONE',  ( -19.51114651407244338, -7.656733154341000436, 60.14748342315007790 ) ) ;
#40052 = EDGE_CURVE ( 'NONE', #748, #21369, #12065, .T. ) ;
#40053 = CARTESIAN_POINT ( 'NONE',  ( -11.29134393598116937, -11.33126488396075260, 64.16354160640879911 ) ) ;
#40054 = CARTESIAN_POINT ( 'NONE',  ( -18.07488717577700754, -21.77899923650016589, 65.64532180046710153 ) ) ;
#40055 = ORIENTED_EDGE ( 'NONE', *, *, #30786, .F. ) ;
#40056 = CARTESIAN_POINT ( 'NONE',  ( -20.77611426707521858, -20.95444529357722629, 58.75361203847226932 ) ) ;
#40057 = DIRECTION ( 'NONE',  ( 0.8447509909909733938, -0.5351595679979650466, 0.000000000000000000 ) ) ;
#40058 = ORIENTED_EDGE ( 'NONE', *, *, #18703, .T. ) ;
#40059 = CARTESIAN_POINT ( 'NONE',  ( -14.60479643987598841, -7.913168514039711887, 60.50491717424539218 ) ) ;
#40060 = ORIENTED_EDGE ( 'NONE', *, *, #48349, .T. ) ;
#40061 = CARTESIAN_POINT ( 'NONE',  ( -26.42409385541305511, -25.10920654474410441, 47.99999999999997868 ) ) ;
#40062 = CARTESIAN_POINT ( 'NONE',  ( -11.02242957576233451, -11.85532881267382166, 74.57312195644870201 ) ) ;
#40063 = CARTESIAN_POINT ( 'NONE',  ( -22.71059208588729561, -10.14448404190931186, 70.02650598627910483 ) ) ;
#40064 = LINE ( 'NONE', #43284, #35304 ) ;
#40065 = ORIENTED_EDGE ( 'NONE', *, *, #10169, .T. ) ;
#40066 = CARTESIAN_POINT ( 'NONE',  ( -17.42409385541305511, -14.80920654474410725, 45.99899999999998101 ) ) ;
#40067 = UNCERTAINTY_MEASURE_WITH_UNIT (LENGTH_MEASURE( 1.000000000000000082E-05 ), #47112, 'distance_accuracy_value', 'NONE');
#40068 =( BOUNDED_CURVE ( )  B_SPLINE_CURVE ( 3, ( #27902, #4775, #20032, #34802 ),
 .UNSPECIFIED., .F., .F. ) 
 B_SPLINE_CURVE_WITH_KNOTS ( ( 4, 4 ),
 ( 0.000000000000000000, 0.4074455897393594039 ),
 .UNSPECIFIED. ) 
 CURVE ( )  GEOMETRIC_REPRESENTATION_ITEM ( )  RATIONAL_B_SPLINE_CURVE ( ( 1.000000000000000000, 0.4567392136813357428, 0.3561768502900316546, 0.6983129098260878465 ) ) 
 REPRESENTATION_ITEM ( '' )  );
#40069 = CARTESIAN_POINT ( 'NONE',  ( -16.65185932245351452, -21.81708442718849383, 65.51092266128213737 ) ) ;
#40070 = CARTESIAN_POINT ( 'NONE',  ( -16.52316554273587101, -21.80170452179945073, 65.24036514508233608 ) ) ;
#40071 = ORIENTED_EDGE ( 'NONE', *, *, #4262, .T. ) ;
#40072 = CARTESIAN_POINT ( 'NONE',  ( -17.42409385541299471, -14.80920654474435594, 52.02966884056656482 ) ) ;
#40073 = CARTESIAN_POINT ( 'NONE',  ( -24.77957839681537777, -15.99319750247286542, 66.20178371291459030 ) ) ;
#40074 = VERTEX_POINT ( 'NONE', #33831 ) ;
#40075 = ORIENTED_EDGE ( 'NONE', *, *, #33653, .F. ) ;
#40076 = CARTESIAN_POINT ( 'NONE',  ( -24.06787342886325121, -18.28917680027896608, 54.27966884056654351 ) ) ;
#40077 = EDGE_CURVE ( 'NONE', #43447, #14295, #44225, .T. ) ;
#40079 = CARTESIAN_POINT ( 'NONE',  ( -11.42587710518540334, -11.10406226247761019, 57.49431069621225276 ) ) ;
#40078 = AXIS2_PLACEMENT_3D ( 'NONE', #25215, #40237, #40953 ) ;
#40080 = CARTESIAN_POINT ( 'NONE',  ( -21.89269609535176997, -8.848005330197558749, 66.78337213843711595 ) ) ;
#40081 = DIRECTION ( 'NONE',  ( -0.3478314405900341799, -0.9375570856950852239, 0.000000000000000000 ) ) ;
#40082 =( BOUNDED_CURVE ( )  B_SPLINE_CURVE ( 3, ( #44844, #3707, #18971, #33468 ),
 .UNSPECIFIED., .F., .F. ) 
 B_SPLINE_CURVE_WITH_KNOTS ( ( 4, 4 ),
 ( 0.9074455897393706172, 1.000000000000000000 ),
 .UNSPECIFIED. ) 
 CURVE ( )  GEOMETRIC_REPRESENTATION_ITEM ( )  RATIONAL_B_SPLINE_CURVE ( ( 0.6983129098261035006, 0.7760317562607071951, 0.8765941196520060652, 1.000000000000000000 ) ) 
 REPRESENTATION_ITEM ( '' )  );
#40083 = CARTESIAN_POINT ( 'NONE',  ( -45.50908060261262023, -14.20920654474410760, 70.87000000000000455 ) ) ;
#40084 = CARTESIAN_POINT ( 'NONE',  ( -11.22844613476422282, -11.44458948612160221, 64.43409918096024569 ) ) ;
#40085 =( BOUNDED_CURVE ( )  B_SPLINE_CURVE ( 3, ( #39976, #13120, #47376, #47611 ),
 .UNSPECIFIED., .F., .F. ) 
 B_SPLINE_CURVE_WITH_KNOTS ( ( 4, 4 ),
 ( 0.000000000000000000, 0.4074455897393624570 ),
 .UNSPECIFIED. ) 
 CURVE ( )  GEOMETRIC_REPRESENTATION_ITEM ( )  RATIONAL_B_SPLINE_CURVE ( ( 1.000000000000000000, 0.4567392136813325787, 0.3561768502900305444, 0.6983129098260937306 ) ) 
 REPRESENTATION_ITEM ( '' )  );
#40086 = CARTESIAN_POINT ( 'NONE',  ( -20.50928888383101167, -8.027964920953767347, 66.82458168832727097 ) ) ;
#40087 = TOROIDAL_SURFACE ( 'NONE', #23576, 1.899999999999999911, 0.1000000000000000056 ) ;
#40088 = ORIENTED_EDGE ( 'NONE', *, *, #17901, .T. ) ;
#40089 = ORIENTED_EDGE ( 'NONE', *, *, #30963, .F. ) ;
#40090 = B_SPLINE_CURVE_WITH_KNOTS ( 'NONE', 3,
 ( #34519, #22735, #7476, #12123, #33784, #7714, #16039, #15548, #41424, #30124 ),
 .UNSPECIFIED., .F., .F.,
 ( 4, 2, 2, 2, 4 ),
 ( 0.000000000000000000, 0.2500000000000000000, 0.5000000000000000000, 0.7500000000000000000, 1.000000000000000000 ),
 .UNSPECIFIED. ) ;
#40091 = EDGE_CURVE ( 'NONE', #34163, #48033, #2635, .T. ) ;
#40092 = CARTESIAN_POINT ( 'NONE',  ( -22.88264614489240856, -10.34704276773305764, 63.35713876973677827 ) ) ;
#40093 = CARTESIAN_POINT ( 'NONE',  ( -19.99112977906324318, -8.296885409642934306, 74.02096600045412345 ) ) ;
#40094 = CARTESIAN_POINT ( 'NONE',  ( -14.92764478915313653, -21.34891159457319532, 61.63600440564275829 ) ) ;
#40095 = CIRCLE ( 'NONE', #799, 0.4000000000000006883 ) ;
#40096 = CARTESIAN_POINT ( 'NONE',  ( -11.01524394860871858, -17.62490983191025862, 71.86718188073483304 ) ) ;
#40097 = ADVANCED_FACE ( 'NONE', ( #21783 ), #18636, .T. ) ;
#40098 = CARTESIAN_POINT ( 'NONE',  ( -14.07063681424402724, -8.156626161945256470, 70.87957628055752934 ) ) ;
#40099 = CARTESIAN_POINT ( 'NONE',  ( -21.00534385650551883, -8.801233750844183135, 48.81488406609782515 ) ) ;
#40100 =( BOUNDED_CURVE ( )  B_SPLINE_CURVE ( 3, ( #44859, #25403, #21946, #21703 ),
 .UNSPECIFIED., .F., .F. ) 
 B_SPLINE_CURVE_WITH_KNOTS ( ( 4, 4 ),
 ( 0.5000000000000000000, 0.9074455897393651771 ),
 .UNSPECIFIED. ) 
 CURVE ( )  GEOMETRIC_REPRESENTATION_ITEM ( )  RATIONAL_B_SPLINE_CURVE ( ( 1.000000000000009548, 0.4567392136813376302, 0.3561768502900256594, 0.6983129098260838497 ) ) 
 REPRESENTATION_ITEM ( '' )  );
#40101 = ORIENTED_EDGE ( 'NONE', *, *, #24490, .T. ) ;
#40102 = CARTESIAN_POINT ( 'NONE',  ( -21.94683289283972982, -20.15404817794292214, 62.34512228983284388 ) ) ;
#40103 = CARTESIAN_POINT ( 'NONE',  ( -13.12613380977788147, -20.89454282643029259, 58.16154686733092660 ) ) ;
#40104 = CARTESIAN_POINT ( 'NONE',  ( -21.50966673221228120, -17.12947588552333045, 49.52966884056655772 ) ) ;
#40105 = CARTESIAN_POINT ( 'NONE',  ( -17.26958401828953171, -19.65204229739824626, 49.52966884056656482 ) ) ;
#40106 = EDGE_CURVE ( 'NONE', #34964, #16737, #3556, .T. ) ;
#40107 = ORIENTED_EDGE ( 'NONE', *, *, #35239, .T. ) ;
#40108 = EDGE_CURVE ( 'NONE', #43339, #17712, #47904, .T. ) ;
#40109 = CARTESIAN_POINT ( 'NONE',  ( -13.88833677318074500, -20.91193151007171736, 64.87139997340349851 ) ) ;
#40110 = EDGE_CURVE ( 'NONE', #42299, #6219, #25973, .T. ) ;
#40111 = CARTESIAN_POINT ( 'NONE',  ( -42.55865267894247239, -14.80920654474414810, 61.92352941176469727 ) ) ;
#40112 = AXIS2_PLACEMENT_3D ( 'NONE', #32936, #17198, #47982 ) ;
#40113 = PLANE ( 'NONE',  #5330 ) ;
#40114 = AXIS2_PLACEMENT_3D ( 'NONE', #30379, #3520, #44917 ) ;
#40115 = CARTESIAN_POINT ( 'NONE',  ( -10.88286923018596575, -17.43962093083235843, 68.11193994895104709 ) ) ;
#40116 = ORIENTED_EDGE ( 'NONE', *, *, #42284, .T. ) ;
#40117 = FACE_OUTER_BOUND ( 'NONE', #25025, .T. ) ;
#40118 = AXIS2_PLACEMENT_3D ( 'NONE', #30414, #40993, #3317 ) ;
#40119 = EDGE_LOOP ( 'NONE', ( #15034, #48221 ) ) ;
#40120 = DIRECTION ( 'NONE',  ( 0.000000000000000000, 0.000000000000000000, -1.000000000000000000 ) ) ;
#40121 = CARTESIAN_POINT ( 'NONE',  ( -19.21722672681719146, -7.578212081832392144, 63.63100440621975906 ) ) ;
#40122 = ORIENTED_EDGE ( 'NONE', *, *, #21678, .T. ) ;
#40123 = CARTESIAN_POINT ( 'NONE',  ( 18.57590614458695200, 2.136931092028981460, 51.79103196254469310 ) ) ;
#40124 = CARTESIAN_POINT ( 'NONE',  ( -13.55534385650551243, -7.417179338643134834, 52.18511593390279302 ) ) ;
#40125 = VERTEX_POINT ( 'NONE', #18562 ) ;
#40126 = DIRECTION ( 'NONE',  ( 1.078708504465006897E-05, 7.367657514171588156E-06, 0.9999999999146782503 ) ) ;
#40127 = AXIS2_PLACEMENT_3D ( 'NONE', #6243, #36261, #36975 ) ;
#40128 = LINE ( 'NONE', #47517, #10233 ) ;
#40129 = CARTESIAN_POINT ( 'NONE',  ( -23.92719381113450083, -11.17417296164256157, 70.00715453762190066 ) ) ;
#40130 = ORIENTED_EDGE ( 'NONE', *, *, #32043, .F. ) ;
#40131 = LINE ( 'NONE', #6393, #21573 ) ;
#40132 = CARTESIAN_POINT ( 'NONE',  ( -16.86460949297358525, -7.773444642497263857, 70.64603134899243742 ) ) ;
#40133 = CARTESIAN_POINT ( 'NONE',  ( -24.09973193186370111, -12.53120327594186634, 69.98062835556456207 ) ) ;
#40134 = CARTESIAN_POINT ( 'NONE',  ( -23.16791676868475491, -10.71612278230448823, 60.01692287334890352 ) ) ;
#40136 = ORIENTED_EDGE ( 'NONE', *, *, #33890, .T. ) ;
#40135 = CLOSED_SHELL ( 'NONE', ( #16477, #30672, #18461, #4989, #7526, #42078, #30367, #24158, #22971, #11962, #15126, #19568, #14978, #20783, #40160, #31719, #1422, #12605, #11998, #38255, #5660, #35590, #36009, #34264, #11423, #13258, #46839, #41901, #37768, #47130, #30430, #17478, #17142, #43866, #6424, #7154, #39495, #14410, #34709, #25016, #15567, #33800, #41912, #35227, #27066, #24761, #2539, #44754, #34935, #5573, #13923, #32200, #25678, #19375, #11111, #30880, #22232, #13266, #43589, #39055, #14627, #14678, #16904, #48680 ) ) ;
#40137 = VERTEX_POINT ( 'NONE', #14852 ) ;
#40138 = CARTESIAN_POINT ( 'NONE',  ( -43.17409385541305511, -15.80920654474410725, 56.99999999999998579 ) ) ;
#40139 = CARTESIAN_POINT ( 'NONE',  ( -21.42336286209559759, -21.09487474236010485, 69.23945462178221533 ) ) ;
#40140 = EDGE_LOOP ( 'NONE', ( #42775, #32203, #43745, #1087, #47609 ) ) ;
#40141 = CARTESIAN_POINT ( 'NONE',  ( -10.43972881942000086, -15.77115500203794873, 64.52243715390834211 ) ) ;
#40142 = CARTESIAN_POINT ( 'NONE',  ( -20.58659385759798965, -7.222650657624104298, 49.61879703869476543 ) ) ;
#40143 = CARTESIAN_POINT ( 'NONE',  ( -11.07857809310684338, -11.73724795245126273, 71.38860870961248395 ) ) ;
#40144 = CARTESIAN_POINT ( 'NONE',  ( -16.93852767260800007, -21.79234520888179460, 68.88663808031736835 ) ) ;
#40145 = CARTESIAN_POINT ( 'NONE',  ( -12.31380134045779506, -10.02538898168817916, 60.55918086676557976 ) ) ;
#40146 = EDGE_LOOP ( 'NONE', ( #38469, #17259, #18566, #39298, #28609 ) ) ;
#40147 = EDGE_CURVE ( 'NONE', #12505, #7647, #17371, .T. ) ;
#40148 = CARTESIAN_POINT ( 'NONE',  ( -10.55579457777002439, -13.45742151464481751, 74.96352273250263920 ) ) ;
#40149 = CARTESIAN_POINT ( 'NONE',  ( -14.55015457993596328, -8.362855509585410019, 70.87390454733632339 ) ) ;
#40150 = CIRCLE ( 'NONE', #41733, 1.999999999999999556 ) ;
#40151 = CARTESIAN_POINT ( 'NONE',  ( -19.70639647806698136, -21.90109437720271757, 65.57990800639531415 ) ) ;
#40152 = CARTESIAN_POINT ( 'NONE',  ( -14.94170459844064780, -18.78425696289860269, 49.52966884056656482 ) ) ;
#40153 = VECTOR ( 'NONE', #47836, 1000.000000000000000 ) ;
#40154 = ORIENTED_EDGE ( 'NONE', *, *, #2796, .T. ) ;
#40155 = ORIENTED_EDGE ( 'NONE', *, *, #40024, .T. ) ;
#40156 = CARTESIAN_POINT ( 'NONE',  ( -24.87126894608573124, -14.60124070896847392, 62.75650584303257062 ) ) ;
#40157 = CARTESIAN_POINT ( 'NONE',  ( -23.34288396506439867, -19.33377296368179543, 59.06906041190286771 ) ) ;
#40158 = VECTOR ( 'NONE', #17548, 1000.000000000000000 ) ;
#40159 = ORIENTED_EDGE ( 'NONE', *, *, #37454, .F. ) ;
#40160 = ADVANCED_FACE ( 'NONE', ( #8473 ), #41723, .T. ) ;
#40161 = CARTESIAN_POINT ( 'NONE',  ( -24.47010849973345614, -14.47977947063238879, 69.95275342396321605 ) ) ;
#40162 = DIRECTION ( 'NONE',  ( 0.000000000000000000, 0.000000000000000000, -1.000000000000000000 ) ) ;
#40163 = EDGE_CURVE ( 'NONE', #20660, #9213, #4785, .T. ) ;
#40164 = ADVANCED_FACE ( 'NONE', ( #19811 ), #35048, .T. ) ;
#40165 = EDGE_CURVE ( 'NONE', #28641, #11779, #8320, .T. ) ;
#40166 = AXIS2_PLACEMENT_3D ( 'NONE', #41016, #10978, #45213 ) ;
#40167 = ORIENTED_EDGE ( 'NONE', *, *, #47728, .F. ) ;
#40168 = CARTESIAN_POINT ( 'NONE',  ( -10.61465111059293598, -17.83148713366484017, 71.66743938577346285 ) ) ;
#40169 =( BOUNDED_CURVE ( )  B_SPLINE_CURVE ( 1, ( #24755, #47157 ),
 .UNSPECIFIED., .F., .F. ) 
 B_SPLINE_CURVE_WITH_KNOTS ( ( 2, 2 ),
 ( 0.000000000000000000, 1.000000000000000000 ),
 .UNSPECIFIED. ) 
 CURVE ( )  GEOMETRIC_REPRESENTATION_ITEM ( )  RATIONAL_B_SPLINE_CURVE ( ( 0.9847253504145836445, 0.9847253504145836445 ) ) 
 REPRESENTATION_ITEM ( '' )  );
#40170 = CARTESIAN_POINT ( 'NONE',  ( -24.47066272824306665, -14.57993217219608795, 62.99824437345093031 ) ) ;
#40171 = CARTESIAN_POINT ( 'NONE',  ( -23.33631914962121456, -10.27599873017480903, 59.77920290994538988 ) ) ;
#40172 = ORIENTED_EDGE ( 'NONE', *, *, #25442, .F. ) ;
#40173 = ORIENTED_EDGE ( 'NONE', *, *, #7715, .F. ) ;
#40174 = CARTESIAN_POINT ( 'NONE',  ( -10.11824970337647223, -16.26811690260224452, 71.56254994910038647 ) ) ;
#40176 = LINE ( 'NONE', #25394, #11635 ) ;
#40175 = AXIS2_PLACEMENT_3D ( 'NONE', #17667, #24109, #20422 ) ;
#40177 = VERTEX_POINT ( 'NONE', #46394 ) ;
#40178 = CARTESIAN_POINT ( 'NONE',  ( -21.42981983006149349, -21.09080987443381261, 69.23167044377096602 ) ) ;
#40179 = DIRECTION ( 'NONE',  ( -0.5263399769092093061, 0.8502742079512979334, 7.678741024442198749E-08 ) ) ;
#40180 = CARTESIAN_POINT ( 'NONE',  ( -23.11784385650551954, -9.790100578890868377, 49.79778022625162492 ) ) ;
#40181 = DIRECTION ( 'NONE',  ( -3.071710424422018668E-17, 6.404604876783312462E-16, 1.000000000000000000 ) ) ;
#40182 = CARTESIAN_POINT ( 'NONE',  ( 18.82590614458706924, 1.890747609047893185, 50.53028072113869484 ) ) ;
#40183 = CARTESIAN_POINT ( 'NONE',  ( -16.65185932245351452, -21.81708442718849383, 65.51092266128213737 ) ) ;
#40184 = EDGE_LOOP ( 'NONE', ( #14453, #7098, #2856, #22566, #46379 ) ) ;
#40185 = CARTESIAN_POINT ( 'NONE',  ( -11.95967870817407430, -14.07562448187690940, 53.88362224778186516 ) ) ;
#40186 = CARTESIAN_POINT ( 'NONE',  ( -11.82257370584654943, -19.00738327630861946, 71.68685835237670290 ) ) ;
#40187 = CARTESIAN_POINT ( 'NONE',  ( -22.94659349086428435, -9.808683002949324603, 70.11840218492315557 ) ) ;
#40188 = FACE_OUTER_BOUND ( 'NONE', #12130, .T. ) ;
#40189 = CARTESIAN_POINT ( 'NONE',  ( -16.09337608010665477, -22.13948405174236811, 58.40090292489767876 ) ) ;
#40190 = CARTESIAN_POINT ( 'NONE',  ( -11.86342561440307186, -10.47520584478210814, 71.26333307341455736 ) ) ;
#40191 = EDGE_CURVE ( 'NONE', #29761, #11480, #31900, .T. ) ;
#40192 = ORIENTED_EDGE ( 'NONE', *, *, #44259, .F. ) ;
#40193 = EDGE_LOOP ( 'NONE', ( #30543, #32870 ) ) ;
#40194 = DIRECTION ( 'NONE',  ( 3.549360974554993999E-17, -6.371834667797928663E-18, -1.000000000000000000 ) ) ;
#40195 = ORIENTED_EDGE ( 'NONE', *, *, #42083, .T. ) ;
#40196 = CARTESIAN_POINT ( 'NONE',  ( -23.46260529264823447, -11.17067950781535579, 73.36193301757424479 ) ) ;
#40198 = PLANE ( 'NONE',  #38337 ) ;
#40197 = CYLINDRICAL_SURFACE ( 'NONE', #19584, 1.999999999999999556 ) ;
#40199 = CIRCLE ( 'NONE', #11871, 0.5560000000000009379 ) ;
#40200 = DIRECTION ( 'NONE',  ( -0.3478314405900341799, -0.9375570856950852239, 0.000000000000000000 ) ) ;
#40201 = CARTESIAN_POINT ( 'NONE',  ( -19.24025795797341942, -7.996846695050864540, 60.24620885950562865 ) ) ;
#40202 = CARTESIAN_POINT ( 'NONE',  ( -50.42609385541305755, -14.80920654474418008, 64.94117647058821774 ) ) ;
#40203 = B_SPLINE_CURVE_WITH_KNOTS ( 'NONE', 1,
 ( #4819, #19842 ),
 .UNSPECIFIED., .F., .F.,
 ( 2, 2 ),
 ( 0.000000000000000000, 1.000000000000000000 ),
 .UNSPECIFIED. ) ;
#40204 = ORIENTED_EDGE ( 'NONE', *, *, #10108, .T. ) ;
#40205 = CARTESIAN_POINT ( 'NONE',  ( -24.72694788909437236, -16.28301151488813403, 62.70833397083087846 ) ) ;
#40206 = PLANE ( 'NONE',  #6622 ) ;
#40207 = FACE_OUTER_BOUND ( 'NONE', #3795, .T. ) ;
#40208 = CARTESIAN_POINT ( 'NONE',  ( -20.60788153932096023, -8.518722016582884748, 63.32593600985608617 ) ) ;
#40209 = ADVANCED_FACE ( 'NONE', ( #20041 ), #47846, .T. ) ;
#40210 = ORIENTED_EDGE ( 'NONE', *, *, #47895, .T. ) ;
#40211 = AXIS2_PLACEMENT_3D ( 'NONE', #36563, #43516, #39564 ) ;
#40212 = DIRECTION ( 'NONE',  ( 0.000000000000000000, 0.000000000000000000, -1.000000000000000000 ) ) ;
#40213 = CARTESIAN_POINT ( 'NONE',  ( -50.42609385541305755, -14.90920654474412643, 59.01176470588234224 ) ) ;
#40214 = ADVANCED_FACE ( 'NONE', ( #34810 ), #15597, .F. ) ;
#40215 = DIRECTION ( 'NONE',  ( 0.07061531369766044230, 0.9975036227860933913, 1.268851335910971019E-08 ) ) ;
#40216 = FACE_OUTER_BOUND ( 'NONE', #38873, .T. ) ;
#40217 = CARTESIAN_POINT ( 'NONE',  ( -10.67250920137991521, -11.65805311173287961, 71.20205571017048385 ) ) ;
#40218 = CARTESIAN_POINT ( 'NONE',  ( -40.92409385541305511, -14.80920654474410725, 74.99999999999998579 ) ) ;
#40219 = ORIENTED_EDGE ( 'NONE', *, *, #5176, .F. ) ;
#40220 = ORIENTED_EDGE ( 'NONE', *, *, #9086, .F. ) ;
#40221 = CARTESIAN_POINT ( 'NONE',  ( -19.65534385541304019, -8.623186033802570094, 49.24843789510466507 ) ) ;
#40222 = AXIS2_PLACEMENT_3D ( 'NONE', #22790, #39178, #37522 ) ;
#40223 = LINE ( 'NONE', #39492, #36614 ) ;
#40224 = CARTESIAN_POINT ( 'NONE',  ( -12.23165125622869631, -10.02867215863997608, 67.64329750964374455 ) ) ;
#40225 =( BOUNDED_CURVE ( )  B_SPLINE_CURVE ( 3, ( #8734, #35294, #47118, #35542 ),
 .UNSPECIFIED., .F., .F. ) 
 B_SPLINE_CURVE_WITH_KNOTS ( ( 4, 4 ),
 ( 0.4074455897393624015, 0.5000000000000000000 ),
 .UNSPECIFIED. ) 
 CURVE ( )  GEOMETRIC_REPRESENTATION_ITEM ( )  RATIONAL_B_SPLINE_CURVE ( ( 0.6983129098260898449, 0.7760317562606841024, 0.8765941196519841938, 0.9999999999999820144 ) ) 
 REPRESENTATION_ITEM ( '' )  );
#40226 = CARTESIAN_POINT ( 'NONE',  ( -20.24909385759799108, -8.112991634885936776, 51.74999426922421719 ) ) ;
#40227 = EDGE_CURVE ( 'NONE', #27599, #16869, #45428, .T. ) ;
#40228 = EDGE_CURVE ( 'NONE', #5464, #11732, #48405, .T. ) ;
#40229 = CARTESIAN_POINT ( 'NONE',  ( -10.45256735519816615, -15.43993469624229853, 57.56792809193251514 ) ) ;
#40230 = ORIENTED_EDGE ( 'NONE', *, *, #28705, .F. ) ;
#40231 = CARTESIAN_POINT ( 'NONE',  ( -10.39215594834096024, -14.30487625923878880, 64.53803863383089379 ) ) ;
#40232 = AXIS2_PLACEMENT_3D ( 'NONE', #25380, #10598, #28823 ) ;
#40233 = CARTESIAN_POINT ( 'NONE',  ( -20.54786284059405688, -21.13826946137156781, 62.25904375309657723 ) ) ;
#40234 = VERTEX_POINT ( 'NONE', #45677 ) ;
#40235 = DIRECTION ( 'NONE',  ( -2.866981220435666553E-17, 1.000000000000000000, 1.190614954331866791E-16 ) ) ;
#40236 =( BOUNDED_CURVE ( )  B_SPLINE_CURVE ( 3, ( #43743, #28947, #32413, #1642 ),
 .UNSPECIFIED., .F., .F. ) 
 B_SPLINE_CURVE_WITH_KNOTS ( ( 4, 4 ),
 ( 0.5000000000000000000, 0.9074455897393596260 ),
 .UNSPECIFIED. ) 
 CURVE ( )  GEOMETRIC_REPRESENTATION_ITEM ( )  RATIONAL_B_SPLINE_CURVE ( ( 1.000000000000023981, 0.4567392136813375192, 0.3561768502900155564, 0.6983129098260840717 ) ) 
 REPRESENTATION_ITEM ( '' )  );
#40237 = DIRECTION ( 'NONE',  ( -0.2771212459065067191, 0.9608349572466770017, 4.100231986695772107E-08 ) ) ;
#40238 = EDGE_LOOP ( 'NONE', ( #33330, #17585 ) ) ;
#40239 = EDGE_CURVE ( 'NONE', #22574, #36634, #30659, .T. ) ;
#40240 = EDGE_CURVE ( 'NONE', #11393, #48283, #24839, .T. ) ;
#40241 = CARTESIAN_POINT ( 'NONE',  ( -17.78451647839747807, -7.367880489560593382, 60.18722466726725884 ) ) ;
#40242 = CARTESIAN_POINT ( 'NONE',  ( -41.42703503188364778, -14.90920654474424367, 70.97647058823527288 ) ) ;
#40243 = CARTESIAN_POINT ( 'NONE',  ( -9.980621257831284510, -14.49716697860085546, 67.95776503052229600 ) ) ;
#40244 = ORIENTED_EDGE ( 'NONE', *, *, #35920, .F. ) ;
#40245 = CARTESIAN_POINT ( 'NONE',  ( -11.92829163603010301, -19.83900259450906489, 58.02708122498009402 ) ) ;
#40246 = AXIS2_PLACEMENT_3D ( 'NONE', #40182, #18234, #36685 ) ;
#40247 = EDGE_CURVE ( 'NONE', #14322, #31196, #29675, .T. ) ;
#40248 = CARTESIAN_POINT ( 'NONE',  ( -24.72409385541305582, -14.80920654474422271, 68.96470588235293064 ) ) ;
#40249 = CARTESIAN_POINT ( 'NONE',  ( -16.72801347667246574, -21.77457299860571283, 65.45237662829435976 ) ) ;
#40250 = CARTESIAN_POINT ( 'NONE',  ( -17.19811928533322387, -9.313850733363548073, 54.07175714974879099 ) ) ;
#40251 = EDGE_LOOP ( 'NONE', ( #17117, #33013, #38230, #24384, #9518 ) ) ;
#40252 = CARTESIAN_POINT ( 'NONE',  ( -15.40811923343077083, -21.56513327689926030, 72.06047564147742435 ) ) ;
#40253 = CARTESIAN_POINT ( 'NONE',  ( -10.76011810543446323, -12.66604461453143493, 60.79853557587211554 ) ) ;
#40254 = CARTESIAN_POINT ( 'NONE',  ( -24.92071865458970947, -14.23843710221147774, 54.02312124697527906 ) ) ;
#40255 = AXIS2_PLACEMENT_3D ( 'NONE', #17181, #13494, #28293 ) ;
#40256 = CARTESIAN_POINT ( 'NONE',  ( -11.57126885336172073, -10.86466612894600381, 74.59451641100736197 ) ) ;
#40257 = EDGE_CURVE ( 'NONE', #45412, #8644, #11444, .T. ) ;
#40258 = CARTESIAN_POINT ( 'NONE',  ( -16.78181722113097152, -22.23154757984593388, 68.73914717078854153 ) ) ;
#40259 = PLANE ( 'NONE',  #22990 ) ;
#40260 = ORIENTED_EDGE ( 'NONE', *, *, #33405, .F. ) ;
#40261 = CARTESIAN_POINT ( 'NONE',  ( -18.52416312356643147, -7.896186446804856374, 73.84064402154488960 ) ) ;
#40262 = CARTESIAN_POINT ( 'NONE',  ( -21.52725980274252393, -9.076272844571150245, 70.43132538913752683 ) ) ;
#40263 = CARTESIAN_POINT ( 'NONE',  ( -18.55957040452605611, -7.446158924837727788, 74.02559677774105751 ) ) ;
#40264 = ORIENTED_EDGE ( 'NONE', *, *, #47916, .T. ) ;
#40265 = CARTESIAN_POINT ( 'NONE',  ( -20.63647318826268773, -18.96169002115701119, 52.02966884056656482 ) ) ;
#40266 = ORIENTED_EDGE ( 'NONE', *, *, #30081, .T. ) ;
#40267 = VERTEX_POINT ( 'NONE', #35539 ) ;
#40268 = ORIENTED_EDGE ( 'NONE', *, *, #4498, .T. ) ;
#40269 = DIRECTION ( 'NONE',  ( -3.071710424422018668E-17, 6.404604876783312462E-16, 1.000000000000000000 ) ) ;
#40270 = CARTESIAN_POINT ( 'NONE',  ( -12.84690951644825851, -8.931012861620404308, 67.56438176077992352 ) ) ;
#40271 = CYLINDRICAL_SURFACE ( 'NONE', #25188, 0.1499999999999991063 ) ;
#40272 = DIRECTION ( 'NONE',  ( 3.071710424422018668E-17, -6.404604876783312462E-16, -1.000000000000000000 ) ) ;
#40273 = ORIENTED_EDGE ( 'NONE', *, *, #39573, .F. ) ;
#40274 = ORIENTED_EDGE ( 'NONE', *, *, #4581, .T. ) ;
#40275 = CARTESIAN_POINT ( 'NONE',  ( -19.06784385650551528, -6.428312510596451368, 51.20221977374900035 ) ) ;
#40276 = DIRECTION ( 'NONE',  ( 0.9687793358424821033, -0.2479245821708677133, 0.000000000000000000 ) ) ;
#40277 = CARTESIAN_POINT ( 'NONE',  ( -10.82849021881276386, -17.15435654512475594, 61.15743105340639119 ) ) ;
#40278 = EDGE_CURVE ( 'NONE', #43505, #10981, #35771, .T. ) ;
#40279 = CARTESIAN_POINT ( 'NONE',  ( -18.39284385650552167, -7.406986770994973490, 48.81910596585309747 ) ) ;
#40280 = VERTEX_POINT ( 'NONE', #28878 ) ;
#40281 = EDGE_CURVE ( 'NONE', #33252, #20890, #5008, .T. ) ;
#40282 = CARTESIAN_POINT ( 'NONE',  ( -15.32518410995109193, -21.95751795911967008, 72.16080160551160816 ) ) ;
#40283 = CARTESIAN_POINT ( 'NONE',  ( -20.00946539473887142, -8.250368680643830999, 73.87096600125035195 ) ) ;
#40284 = ORIENTED_EDGE ( 'NONE', *, *, #15183, .F. ) ;
#40285 = LINE ( 'NONE', #24790, #28062 ) ;
#40286 = VERTEX_POINT ( 'NONE', #20286 ) ;
#40287 = ADVANCED_FACE ( 'NONE', ( #31852 ), #28645, .T. ) ;
#40288 = CYLINDRICAL_SURFACE ( 'NONE', #43367, 1.999999999999999556 ) ;
#40289 = CARTESIAN_POINT ( 'NONE',  ( -16.34036753895378524, -21.72486956401631630, 58.51258804093296106 ) ) ;
#40290 = CARTESIAN_POINT ( 'NONE',  ( -11.35825037048775066, -11.21643016533577075, 60.67885780704620657 ) ) ;
#40291 = EDGE_CURVE ( 'NONE', #35967, #11672, #14998, .T. ) ;
#40292 = ORIENTED_EDGE ( 'NONE', *, *, #32943, .T. ) ;
#40293 = CARTESIAN_POINT ( 'NONE',  ( -19.50103315386265024, -8.068942516160735323, 60.37581784757137626 ) ) ;
#40294 = EDGE_CURVE ( 'NONE', #700, #44129, #43815, .T. ) ;
#40295 = CARTESIAN_POINT ( 'NONE',  ( -22.83929682888979329, -10.29453308790038157, 66.55654356380499337 ) ) ;
#40296 = CARTESIAN_POINT ( 'NONE',  ( -21.68499490698325971, -9.192515188766618550, 66.81149992326716358 ) ) ;
#40297 = VERTEX_POINT ( 'NONE', #35290 ) ;
#40298 = CARTESIAN_POINT ( 'NONE',  ( -10.42302287260171312, -13.97751933429587012, 57.73352905910142852 ) ) ;
#40299 = CARTESIAN_POINT ( 'NONE',  ( -10.42431094601142050, -14.74024948089186537, 71.32782695460157640 ) ) ;
#40300 = DIRECTION ( 'NONE',  ( -0.3478314405900309603, -0.9375570856950864451, 0.000000000000000000 ) ) ;
#40301 = ORIENTED_EDGE ( 'NONE', *, *, #26662, .T. ) ;
#40302 = CYLINDRICAL_SURFACE ( 'NONE', #43894, 1.999999999999999556 ) ;
#40303 = ORIENTED_EDGE ( 'NONE', *, *, #31433, .T. ) ;
#40304 = FACE_OUTER_BOUND ( 'NONE', #28093, .T. ) ;
#40305 = CARTESIAN_POINT ( 'NONE',  ( -13.70502021987594077, -20.80197949353049580, 68.87113990053892110 ) ) ;
#40306 = CARTESIAN_POINT ( 'NONE',  ( -11.36794959886231915, -18.31963617796164812, 57.80714594517343841 ) ) ;
#40307 = CARTESIAN_POINT ( 'NONE',  ( -45.92409385541306222, 12.69079345525585545, 71.75000000000001421 ) ) ;
#40308 = ORIENTED_EDGE ( 'NONE', *, *, #22655, .T. ) ;
#40309 = CYLINDRICAL_SURFACE ( 'NONE', #6366, 0.1500000000000080158 ) ;
#40310 = EDGE_CURVE ( 'NONE', #14550, #1220, #45987, .T. ) ;
#40311 = CARTESIAN_POINT ( 'NONE',  ( -19.04787736696107103, -7.538188104413229063, 67.02354920417977269 ) ) ;
#40312 = CARTESIAN_POINT ( 'NONE',  ( -15.69205246790211561, -7.972184624072811587, 74.49474465824219749 ) ) ;
#40313 = ORIENTED_EDGE ( 'NONE', *, *, #46255, .T. ) ;
#40314 = CARTESIAN_POINT ( 'NONE',  ( -11.22166882806820176, -18.93646342201198607, 64.86894282563231684 ) ) ;
#40315 = CARTESIAN_POINT ( 'NONE',  ( -24.28579947082789303, -13.18942387424446494, 62.84736316175410309 ) ) ;
#40316 = ORIENTED_EDGE ( 'NONE', *, *, #12933, .F. ) ;
#40317 = EDGE_LOOP ( 'NONE', ( #35140, #47245, #32923, #40511, #6815 ) ) ;
#40318 = CARTESIAN_POINT ( 'NONE',  ( -13.14551704304688684, -16.75068433397603940, 52.02966884056656482 ) ) ;
#40319 = CARTESIAN_POINT ( 'NONE',  ( -8.424093855413071097, -6.359206544744109735, 52.99999999999997868 ) ) ;
#40320 = DIRECTION ( 'NONE',  ( -0.000000000000000000, -0.000000000000000000, 1.000000000000000000 ) ) ;
#40321 = CARTESIAN_POINT ( 'NONE',  ( -23.39635208968330105, -11.04794396834914494, 70.04777744521437910 ) ) ;
#40322 = CARTESIAN_POINT ( 'NONE',  ( -14.87886258693389507, -8.287862487286286495, 60.33612870302592057 ) ) ;
#40323 = CARTESIAN_POINT ( 'NONE',  ( -12.35395094432871410, -20.26789845123980527, 68.59303345011528563 ) ) ;
#40324 = CARTESIAN_POINT ( 'NONE',  ( -22.22370946352282672, -9.111183370010303761, 59.90666632495347699 ) ) ;
#40325 = ORIENTED_EDGE ( 'NONE', *, *, #23442, .T. ) ;
#40326 = ORIENTED_EDGE ( 'NONE', *, *, #16423, .F. ) ;
#40327 = CARTESIAN_POINT ( 'NONE',  ( -19.05047292022263505, -10.41396213884962663, 52.02966884056656482 ) ) ;
#40328 = CARTESIAN_POINT ( 'NONE',  ( -21.80947398209100285, -9.353160252369512762, 63.49153755919518005 ) ) ;
#40329 = CARTESIAN_POINT ( 'NONE',  ( -11.01524411412108151, -17.62491020911333450, 71.56718188073510589 ) ) ;
#40330 = CARTESIAN_POINT ( 'NONE',  ( -18.54539007733004397, -7.443902428285554151, 74.00097724639977059 ) ) ;
#40331 = VERTEX_POINT ( 'NONE', #2545 ) ;
#40332 = EDGE_CURVE ( 'NONE', #13421, #27240, #21014, .T. ) ;
#40333 = CARTESIAN_POINT ( 'NONE',  ( -18.19284385650551883, -7.406986770994973490, 48.81910596585309747 ) ) ;
#40334 = ORIENTED_EDGE ( 'NONE', *, *, #45438, .F. ) ;
#40335 = CARTESIAN_POINT ( 'NONE',  ( -14.59650283654637271, -21.27602155829186259, 61.78033139454115030 ) ) ;
#40336 = CARTESIAN_POINT ( 'NONE',  ( -23.98955618046187865, -11.28797293959267023, 66.59931407123043812 ) ) ;
#40337 = AXIS2_PLACEMENT_3D ( 'NONE', #13125, #24496, #20781 ) ;
#40338 = LINE ( 'NONE', #6609, #10360 ) ;
#40339 = FACE_OUTER_BOUND ( 'NONE', #8431, .T. ) ;
#40340 = VERTEX_POINT ( 'NONE', #25660 ) ;
#40341 = B_SPLINE_CURVE_WITH_KNOTS ( 'NONE', 3,
 ( #23199, #537, #4468, #30837, #30352, #7700, #45853, #4000, #37450, #34752 ),
 .UNSPECIFIED., .F., .F.,
 ( 4, 2, 2, 2, 4 ),
 ( 0.000000000000000000, 0.2500000000000000000, 0.5000000000000000000, 0.7500000000000000000, 1.000000000000000000 ),
 .UNSPECIFIED. ) ;
#40342 = LINE ( 'NONE', #1945, #24371 ) ;
#40343 = CARTESIAN_POINT ( 'NONE',  ( -12.78931795874336430, -9.563283354468385511, 74.60457613011958244 ) ) ;
#40344 = ADVANCED_FACE ( 'NONE', ( #36971 ), #14790, .T. ) ;
#40345 = DIRECTION ( 'NONE',  ( 0.9372362738803845517, 0.3486949482324239735, -5.386914174890155429E-09 ) ) ;
#40346 = EDGE_CURVE ( 'NONE', #37913, #11700, #14556, .T. ) ;
#40347 =( BOUNDED_CURVE ( )  B_SPLINE_CURVE ( 3, ( #3926, #4174, #34419, #11307 ),
 .UNSPECIFIED., .F., .F. ) 
 B_SPLINE_CURVE_WITH_KNOTS ( ( 4, 4 ),
 ( 0.4074455897393696180, 0.5000000000000000000 ),
 .UNSPECIFIED. ) 
 CURVE ( )  GEOMETRIC_REPRESENTATION_ITEM ( )  RATIONAL_B_SPLINE_CURVE ( ( 0.6983129098261106060, 0.7760317562606908748, 0.8765941196519806411, 0.9999999999999641398 ) ) 
 REPRESENTATION_ITEM ( '' )  );
#40348 = CARTESIAN_POINT ( 'NONE',  ( -12.48216758013337113, -16.58117287899024461, 50.77966884056655772 ) ) ;
#40349 = EDGE_LOOP ( 'NONE', ( #39090, #7556, #6540, #10549, #47497 ) ) ;
#40350 = CARTESIAN_POINT ( 'NONE',  ( -20.95199379672471096, -20.85531803099279458, 65.88453983062113650 ) ) ;
#40351 = ORIENTED_EDGE ( 'NONE', *, *, #14353, .T. ) ;
#40352 = CARTESIAN_POINT ( 'NONE',  ( -4.424093855413056886, -27.10920654474410796, 79.99999999999998579 ) ) ;
#40353 = EDGE_CURVE ( 'NONE', #29232, #43757, #36488, .T. ) ;
#40354 = VERTEX_POINT ( 'NONE', #6958 ) ;
#40355 = LINE ( 'NONE', #40123, #45478 ) ;
#40356 = CARTESIAN_POINT ( 'NONE',  ( -13.89284385650552167, -7.406986770994972602, 48.81910596585309747 ) ) ;
#40357 = ORIENTED_EDGE ( 'NONE', *, *, #3019, .T. ) ;
#40358 = CARTESIAN_POINT ( 'NONE',  ( -18.71757194967216975, -7.929750632967406787, 70.37068030597254165 ) ) ;
#40359 = EDGE_CURVE ( 'NONE', #39039, #30917, #2251, .T. ) ;
#40360 = LINE ( 'NONE', #21423, #44826 ) ;
#40361 =( BOUNDED_CURVE ( )  B_SPLINE_CURVE ( 3, ( #20844, #24309, #35607, #35370 ),
 .UNSPECIFIED., .F., .F. ) 
 B_SPLINE_CURVE_WITH_KNOTS ( ( 4, 4 ),
 ( 0.4074455897393707837, 0.5000000000000000000 ),
 .UNSPECIFIED. ) 
 CURVE ( )  GEOMETRIC_REPRESENTATION_ITEM ( )  RATIONAL_B_SPLINE_CURVE ( ( 0.6983129098261093848, 0.7760317562607007558, 0.8765941196519941858, 0.9999999999999816813 ) ) 
 REPRESENTATION_ITEM ( '' )  );
#40362 = CARTESIAN_POINT ( 'NONE',  ( -20.12289019246589206, -7.865124395032225380, 73.90592041591946781 ) ) ;
#40363 = ORIENTED_EDGE ( 'NONE', *, *, #12287, .T. ) ;
#40365 = CARTESIAN_POINT ( 'NONE',  ( -19.97164353606484255, -21.81018995992316079, 69.11977899231902711 ) ) ;
#40364 =( BOUNDED_CURVE ( )  B_SPLINE_CURVE ( 3, ( #4492, #15553, #45153, #41685 ),
 .UNSPECIFIED., .F., .F. ) 
 B_SPLINE_CURVE_WITH_KNOTS ( ( 4, 4 ),
 ( 0.4074455897393695625, 0.5000000000000000000 ),
 .UNSPECIFIED. ) 
 CURVE ( )  GEOMETRIC_REPRESENTATION_ITEM ( )  RATIONAL_B_SPLINE_CURVE ( ( 0.6983129098261096068, 0.7760317562606910968, 0.8765941196519815293, 0.9999999999999659162 ) ) 
 REPRESENTATION_ITEM ( '' )  );
#40366 = EDGE_CURVE ( 'NONE', #46408, #39071, #11436, .T. ) ;
#40367 = CARTESIAN_POINT ( 'NONE',  ( -11.95960950777170062, -10.43434529725880466, 67.69000071772322258 ) ) ;
#40368 = CARTESIAN_POINT ( 'NONE',  ( -17.42409385541305511, -14.80920654474411080, 47.99999999999997868 ) ) ;
#40369 = VECTOR ( 'NONE', #32658, 1000.000000000000114 ) ;
#40370 = ORIENTED_EDGE ( 'NONE', *, *, #26750, .T. ) ;
#40371 = ORIENTED_EDGE ( 'NONE', *, *, #20068, .F. ) ;
#40372 = CARTESIAN_POINT ( 'NONE',  ( -23.34092575347512266, -10.28207967581048088, 59.78698817202694471 ) ) ;
#40373 = CARTESIAN_POINT ( 'NONE',  ( -11.88348671940001999, -10.53106331603155077, 70.98395522823196302 ) ) ;
#40374 = EDGE_LOOP ( 'NONE', ( #45288, #45900, #10094, #18189, #40326 ) ) ;
#40375 = CARTESIAN_POINT ( 'NONE',  ( -11.42587710518540334, -11.10406226247761019, 57.49431069621225276 ) ) ;
#40376 = CARTESIAN_POINT ( 'NONE',  ( -16.36784385759798965, -9.357632978295830739, 49.97845033065684106 ) ) ;
#40377 = DIRECTION ( 'NONE',  ( -5.731567514496413899E-31, -1.020425574103664789E-16, -1.000000000000000000 ) ) ;
#40378 = DIRECTION ( 'NONE',  ( 1.000000000000000000, -4.164305804376849172E-17, 1.614929280266638808E-16 ) ) ;
#40379 =( BOUNDED_SURFACE ( )  B_SPLINE_SURFACE ( 3, 1, ( 
 ( #6915, #18714 ),
 ( #17978, #33728 ),
 ( #15010, #30073 ),
 ( #18975, #18225 ),
 ( #48273, #7176 ),
 ( #11345, #14749 ),
 ( #29821, #44850 ) ),
 .UNSPECIFIED., .T., .F., .F. ) 
 B_SPLINE_SURFACE_WITH_KNOTS ( ( 4, 3, 4 ),
 ( 2, 2 ),
 ( 0.000000000000000000, 0.5000000000000000000, 1.000000000000000000 ),
 ( 0.000000000000000000, 1.000000000000000000 ),
 .UNSPECIFIED. ) 
 GEOMETRIC_REPRESENTATION_ITEM ( )  RATIONAL_B_SPLINE_SURFACE ( (
 ( 1.000000000000000000, 1.000000000000000000),
 ( 0.3333333333333335369, 0.3333333333333330373),
 ( 0.3333333333333335369, 0.3333333333333330373),
 ( 1.000000000000000000, 1.000000000000000000),
 ( 0.3333333333333333703, 0.3333333333333333703),
 ( 0.3333333333333333703, 0.3333333333333333703),
 ( 1.000000000000000000, 1.000000000000000000) ) ) 
 REPRESENTATION_ITEM ( '' )  SURFACE ( )  );
#40380 = VERTEX_POINT ( 'NONE', #6715 ) ;
#40381 = CARTESIAN_POINT ( 'NONE',  ( -20.78299823145727387, -8.610459808214880439, 59.85597358678664648 ) ) ;
#40382 = CARTESIAN_POINT ( 'NONE',  ( -17.19980194945414809, -7.762775306501539241, 70.64035839668011363 ) ) ;
#40383 = CARTESIAN_POINT ( 'NONE',  ( -16.56702387822477363, -22.20979222136662656, 65.33226067334068432 ) ) ;
#40384 = EDGE_CURVE ( 'NONE', #44513, #28707, #4149, .T. ) ;
#40385 = ORIENTED_EDGE ( 'NONE', *, *, #35204, .T. ) ;
#40386 = ORIENTED_EDGE ( 'NONE', *, *, #11206, .T. ) ;
#40387 = CARTESIAN_POINT ( 'NONE',  ( -17.68062394802985793, -21.85468638579756373, 58.41113140978044527 ) ) ;
#40388 = LINE ( 'NONE', #47775, #37054 ) ;
#40389 = CARTESIAN_POINT ( 'NONE',  ( -23.89200480383413350, -11.11192299349349533, 70.07706151945906470 ) ) ;
#40390 = CARTESIAN_POINT ( 'NONE',  ( -11.37338168604670408, -19.15691247995520996, 71.87341272242258583 ) ) ;
#40391 = ORIENTED_EDGE ( 'NONE', *, *, #45324, .T. ) ;
#40392 = EDGE_CURVE ( 'NONE', #42072, #36064, #14314, .T. ) ;
#40393 = CARTESIAN_POINT ( 'NONE',  ( -24.45201636468675943, -14.25170757634699825, 69.95275273439749242 ) ) ;
#40394 = CARTESIAN_POINT ( 'NONE',  ( -12.47302444406249933, -9.241390648102244754, 74.43267637782378188 ) ) ;
#40395 = VECTOR ( 'NONE', #20511, 1000.000000000000000 ) ;
#40396 = VERTEX_POINT ( 'NONE', #22223 ) ;
#40397 = CARTESIAN_POINT ( 'NONE',  ( -13.64450405064090788, -21.22941549479649126, 68.57908268650601258 ) ) ;
#40398 = CARTESIAN_POINT ( 'NONE',  ( -12.99758330771203951, -9.386476247090117297, 70.84925353123610137 ) ) ;
#40399 = CYLINDRICAL_SURFACE ( 'NONE', #28877, 0.1500000000000063227 ) ;
#40400 = EDGE_LOOP ( 'NONE', ( #29792, #31493, #38244, #2820, #26233 ) ) ;
#40401 = CARTESIAN_POINT ( 'NONE',  ( -14.65765131015531253, -21.78034674156931061, 53.49999999999994316 ) ) ;
#40402 = VERTEX_POINT ( 'NONE', #10423 ) ;
#40403 = FACE_OUTER_BOUND ( 'NONE', #18243, .T. ) ;
#40404 = CARTESIAN_POINT ( 'NONE',  ( 8.575906144586953772, 1.671029476340948561, 40.52956954931881484 ) ) ;
#40405 = EDGE_CURVE ( 'NONE', #8735, #26020, #32639, .T. ) ;
#40406 = PLANE ( 'NONE',  #5354 ) ;
#40407 = ORIENTED_EDGE ( 'NONE', *, *, #41868, .F. ) ;
#40408 = CARTESIAN_POINT ( 'NONE',  ( -14.41069671968389265, -11.21995593321280360, 49.52966884056655772 ) ) ;
#40409 = CARTESIAN_POINT ( 'NONE',  ( -24.02655296236175175, -11.35792967378293916, 66.53719098615387395 ) ) ;
#40410 = DIRECTION ( 'NONE',  ( 0.4007314504464623006, -0.1985303619678229492, 0.8944271909999157444 ) ) ;
#40411 = EDGE_CURVE ( 'NONE', #3011, #38799, #27430, .T. ) ;
#40412 = CARTESIAN_POINT ( 'NONE',  ( -10.05141141991806641, -15.87983426743701543, 64.60797347950868641 ) ) ;
#40413 = DIRECTION ( 'NONE',  ( -2.866981220435666553E-17, 1.000000000000000000, 1.190614954331866791E-16 ) ) ;
#40414 = DIRECTION ( 'NONE',  ( 0.6408936281290997794, 0.7676297007174212039, 4.260501105223829885E-08 ) ) ;
#40415 = ORIENTED_EDGE ( 'NONE', *, *, #43427, .F. ) ;
#40416 = CARTESIAN_POINT ( 'NONE',  ( -12.12786991918758339, -13.32596279628197600, 53.49999999999995026 ) ) ;
#40417 = CARTESIAN_POINT ( 'NONE',  ( -16.09337498760136853, -22.13948385882417824, 58.40090183616962349 ) ) ;
#40418 = CARTESIAN_POINT ( 'NONE',  ( -23.98474799315784978, -17.25007060033011896, 69.41339792561625188 ) ) ;
#40419 = CARTESIAN_POINT ( 'NONE',  ( -13.17770392829461912, -20.93059606819637608, 58.15311748147730952 ) ) ;
#40420 = DIRECTION ( 'NONE',  ( 0.9163203205182083311, 0.4004460890125009498, -2.380681616944615543E-09 ) ) ;
#40421 = CARTESIAN_POINT ( 'NONE',  ( -22.60922486080212934, -15.63195587288279320, 52.02966884056656482 ) ) ;
#40422 = ORIENTED_EDGE ( 'NONE', *, *, #32814, .F. ) ;
#40423 = ORIENTED_EDGE ( 'NONE', *, *, #31325, .T. ) ;
#40424 = CARTESIAN_POINT ( 'NONE',  ( -23.68653687815194786, -11.57061008776567945, 66.43686604568146947 ) ) ;
#40425 = CARTESIAN_POINT ( 'NONE',  ( -21.73662441638723308, -9.231682010981758779, 66.67622112302015580 ) ) ;
#40426 = ORIENTED_EDGE ( 'NONE', *, *, #7715, .T. ) ;
#40428 = CARTESIAN_POINT ( 'NONE',  ( -11.71830028707309523, -18.86652491371886242, 71.91515846292473668 ) ) ;
#40427 = FACE_OUTER_BOUND ( 'NONE', #35188, .T. ) ;
#40429 = CARTESIAN_POINT ( 'NONE',  ( -15.34465393633500518, -21.54586957516256263, 68.86120835375241711 ) ) ;
#40430 = CARTESIAN_POINT ( 'NONE',  ( -10.40888613812686359, -14.10966362093629378, 61.06821293886368807 ) ) ;
#40431 = DIRECTION ( 'NONE',  ( -5.731567514496413899E-31, -1.020425574103664789E-16, -1.000000000000000000 ) ) ;
#40432 = EDGE_CURVE ( 'NONE', #16630, #43698, #43724, .T. ) ;
#40433 = CARTESIAN_POINT ( 'NONE',  ( -24.35389707626741185, -16.10709931453381216, 62.87856533165624029 ) ) ;
#40434 = ADVANCED_FACE ( 'NONE', ( #48558 ), #7463, .T. ) ;
#40435 = CARTESIAN_POINT ( 'NONE',  ( -50.42609385541305755, -14.90920654474412643, 59.01176470588234224 ) ) ;
#40436 = AXIS2_PLACEMENT_3D ( 'NONE', #3550, #17590, #18556 ) ;
#40437 = CARTESIAN_POINT ( 'NONE',  ( -23.75797251732913296, -17.78947179557082592, 59.00378417803962350 ) ) ;
#40438 = EDGE_CURVE ( 'NONE', #8094, #28537, #10664, .T. ) ;
#40439 = ADVANCED_FACE ( 'NONE', ( #1028 ), #541, .T. ) ;
#40440 = EDGE_LOOP ( 'NONE', ( #14786, #20534, #44545, #45264 ) ) ;
#40441 = CARTESIAN_POINT ( 'NONE',  ( -10.39679176622870038, -14.24023819782134481, 64.40275955115841100 ) ) ;
#40442 = DIRECTION ( 'NONE',  ( 0.000000000000000000, 1.000000000000000000, -0.000000000000000000 ) ) ;
#40443 = CARTESIAN_POINT ( 'NONE',  ( -21.02642643314752036, -20.81301377900324212, 69.24377353718439565 ) ) ;
#40444 = CARTESIAN_POINT ( 'NONE',  ( -13.77494768682002935, -20.78293651617081750, 65.28628829308328818 ) ) ;
#40445 = CARTESIAN_POINT ( 'NONE',  ( -11.58273428586415221, -10.94902261066962978, 57.31976413542670201 ) ) ;
#40446 = ORIENTED_EDGE ( 'NONE', *, *, #33947, .F. ) ;
#40447 = ORIENTED_EDGE ( 'NONE', *, *, #3603, .F. ) ;
#40448 = CARTESIAN_POINT ( 'NONE',  ( -18.86784385541304943, -9.357632978295830739, 49.97845033065684106 ) ) ;
#40449 = ORIENTED_EDGE ( 'NONE', *, *, #32593, .T. ) ;
#40450 = CARTESIAN_POINT ( 'NONE',  ( -46.92409385541305511, -17.80920654474410370, 61.49999999999999289 ) ) ;
#40451 = CARTESIAN_POINT ( 'NONE',  ( -19.03885666732217885, -7.536228653801991584, 67.15717731432056326 ) ) ;
#40452 =( BOUNDED_CURVE ( )  B_SPLINE_CURVE ( 3, ( #26991, #19856, #24037, #414 ),
 .UNSPECIFIED., .F., .F. ) 
 B_SPLINE_CURVE_WITH_KNOTS ( ( 4, 4 ),
 ( 0.5000000000000000000, 0.9074455897393708392 ),
 .UNSPECIFIED. ) 
 CURVE ( )  GEOMETRIC_REPRESENTATION_ITEM ( )  RATIONAL_B_SPLINE_CURVE ( ( 1.000000000000017986, 0.4567392136813231973, 0.3561768502900144462, 0.6983129098261110501 ) ) 
 REPRESENTATION_ITEM ( '' )  );
#40453 = CARTESIAN_POINT ( 'NONE',  ( -45.92409385541306222, -14.20920654474410760, 71.05600000000001160 ) ) ;
#40454 = EDGE_CURVE ( 'NONE', #3383, #28963, #18519, .T. ) ;
#40455 = CARTESIAN_POINT ( 'NONE',  ( -15.55171133418867235, -7.598245370416885969, 70.79485226425863686 ) ) ;
#40456 = ORIENTED_EDGE ( 'NONE', *, *, #4368, .F. ) ;
#40457 = CARTESIAN_POINT ( 'NONE',  ( -13.47381639519378105, -21.12577003491056260, 65.24274829841968426 ) ) ;
#40458 = CARTESIAN_POINT ( 'NONE',  ( -23.23520415037899411, -10.14728669485665691, 63.22185993134614534 ) ) ;
#40459 = ORIENTED_EDGE ( 'NONE', *, *, #5890, .T. ) ;
#40460 = CARTESIAN_POINT ( 'NONE',  ( -15.28291115335697192, -21.52618774670101232, 68.72592918174676413 ) ) ;
#40461 = CIRCLE ( 'NONE', #14487, 0.4000000000000011879 ) ;
#40462 = EDGE_LOOP ( 'NONE', ( #41047, #11170, #14651, #4515, #27837 ) ) ;
#40463 = B_SPLINE_CURVE_WITH_KNOTS ( 'NONE', 3,
 ( #22992, #328, #15312, #30376, #22484, #45876, #26185, #27150, #7483, #37977 ),
 .UNSPECIFIED., .F., .F.,
 ( 4, 2, 2, 2, 4 ),
 ( 0.000000000000000000, 0.2500000000000000000, 0.5000000000000000000, 0.7500000000000000000, 1.000000000000000000 ),
 .UNSPECIFIED. ) ;
#40464 = FACE_OUTER_BOUND ( 'NONE', #22021, .T. ) ;
#40465 = CARTESIAN_POINT ( 'NONE',  ( -10.33531692083374587, -17.10115316349580894, 57.87255846826901262 ) ) ;
#40466 = DIRECTION ( 'NONE',  ( -3.071710424422018668E-17, 6.404604876783312462E-16, 1.000000000000000000 ) ) ;
#40467 = VERTEX_POINT ( 'NONE', #4975 ) ;
#40468 = DIRECTION ( 'NONE',  ( -5.731567514496413899E-31, -1.020425574103664789E-16, -1.000000000000000000 ) ) ;
#40469 = AXIS2_PLACEMENT_3D ( 'NONE', #39281, #47158, #24269 ) ;
#40470 = CARTESIAN_POINT ( 'NONE',  ( -24.05420634179087358, -17.20676946999824608, 69.69867738674849988 ) ) ;
#40471 = CARTESIAN_POINT ( 'NONE',  ( -15.11195830621016256, -21.41632612911037370, 65.40596681519618016 ) ) ;
#40472 = CARTESIAN_POINT ( 'NONE',  ( -23.92992157843938728, -17.39298733450930001, 66.24357246489365991 ) ) ;
#40473 = EDGE_LOOP ( 'NONE', ( #39045, #25165, #17661, #34379, #31814 ) ) ;
#40474 = FACE_OUTER_BOUND ( 'NONE', #17196, .T. ) ;
#40475 = CARTESIAN_POINT ( 'NONE',  ( -10.72789316105772528, -12.76937900761250155, 60.90739623444811457 ) ) ;
#40476 = CARTESIAN_POINT ( 'NONE',  ( -23.30963478160716562, -18.69084381296369912, 69.30844128244088154 ) ) ;
#40477 = LINE ( 'NONE', #2333, #3447 ) ;
#40478 = CARTESIAN_POINT ( 'NONE',  ( -10.12326195556307695, -13.32541703369907893, 74.86313051124790263 ) ) ;
#40479 = PLANE ( 'NONE',  #28913 ) ;
#40480 = VERTEX_POINT ( 'NONE', #23440 ) ;
#40481 = CARTESIAN_POINT ( 'NONE',  ( -24.33626633208317713, -17.58850949613905001, 66.04333621789641029 ) ) ;
#40482 = CARTESIAN_POINT ( 'NONE',  ( -50.42509385541305988, -8.109206544744111511, 49.44999999999998863 ) ) ;
#40483 = CARTESIAN_POINT ( 'NONE',  ( 10.57590614458695377, 1.890747609047612521, 50.53028072113853142 ) ) ;
#40484 = EDGE_LOOP ( 'NONE', ( #29544, #4187 ) ) ;
#40485 = DIRECTION ( 'NONE',  ( 0.000000000000000000, 0.007114381193220334181, -0.9999746924698833528 ) ) ;
#40486 = ORIENTED_EDGE ( 'NONE', *, *, #9959, .T. ) ;
#40487 = EDGE_CURVE ( 'NONE', #43456, #15655, #16730, .T. ) ;
#40488 = ADVANCED_FACE ( 'NONE', ( #310 ), #42153, .T. ) ;
#40489 = ORIENTED_EDGE ( 'NONE', *, *, #11385, .T. ) ;
#40490 = VERTEX_POINT ( 'NONE', #42399 ) ;
#40491 = B_SPLINE_CURVE_WITH_KNOTS ( 'NONE', 3,
 ( #32378, #6515, #21296, #36042, #28674, #6017, #21536, #16607, #47149, #13144 ),
 .UNSPECIFIED., .F., .F.,
 ( 4, 2, 2, 2, 4 ),
 ( 0.6272669072877486984, 0.7522669073072625334, 0.8772669073267762574, 1.002266907346290203, 1.127266907365803927 ),
 .UNSPECIFIED. ) ;
#40492 = CARTESIAN_POINT ( 'NONE',  ( -14.34311226469532841, -8.523215522210126238, 70.74574244503894249 ) ) ;
#40493 =( BOUNDED_SURFACE ( )  B_SPLINE_SURFACE ( 3, 1, ( 
 ( #38421, #46321 ),
 ( #19472, #7935 ),
 ( #35215, #4710 ),
 ( #23424, #16009 ),
 ( #37943, #4457 ),
 ( #19238, #38917 ),
 ( #38676, #23679 ) ),
 .UNSPECIFIED., .T., .F., .F. ) 
 B_SPLINE_SURFACE_WITH_KNOTS ( ( 4, 3, 4 ),
 ( 2, 2 ),
 ( 0.000000000000000000, 0.5000000000000000000, 1.000000000000000000 ),
 ( 0.000000000000000000, 1.000000000000000000 ),
 .UNSPECIFIED. ) 
 GEOMETRIC_REPRESENTATION_ITEM ( )  RATIONAL_B_SPLINE_SURFACE ( (
 ( 1.000000000000000000, 1.000000000000000000),
 ( 0.3333333333333335369, 0.3333333333333330373),
 ( 0.3333333333333335369, 0.3333333333333330373),
 ( 1.000000000000000000, 1.000000000000000000),
 ( 0.3333333333333333703, 0.3333333333333333703),
 ( 0.3333333333333333703, 0.3333333333333333703),
 ( 1.000000000000000000, 1.000000000000000000) ) ) 
 REPRESENTATION_ITEM ( '' )  SURFACE ( )  );
#40494 = CARTESIAN_POINT ( 'NONE',  ( -13.97958029355460852, -17.98703734140009303, 49.52966884056656482 ) ) ;
#40495 = CARTESIAN_POINT ( 'NONE',  ( -13.16256456194319391, -9.182988408105495992, 60.59517097614691039 ) ) ;
#40496 = VERTEX_POINT ( 'NONE', #38692 ) ;
#40497 = ORIENTED_EDGE ( 'NONE', *, *, #24071, .F. ) ;
#40498 = AXIS2_PLACEMENT_3D ( 'NONE', #25906, #22215, #10647 ) ;
#40499 = EDGE_CURVE ( 'NONE', #4075, #25448, #22696, .T. ) ;
#40500 = EDGE_CURVE ( 'NONE', #33937, #47544, #47888, .T. ) ;
#40501 = CARTESIAN_POINT ( 'NONE',  ( -18.28034385650551741, -6.424090610841176385, 49.80797279389977916 ) ) ;
#40502 = CARTESIAN_POINT ( 'NONE',  ( -10.81230840161673967, -17.25685697075765646, 64.64211442681141762 ) ) ;
#40503 = LINE ( 'NONE', #36318, #41806 ) ;
#40504 = CARTESIAN_POINT ( 'NONE',  ( -20.30534385650551243, -8.801233750844183135, 48.81488406609782515 ) ) ;
#40505 =( BOUNDED_CURVE ( )  B_SPLINE_CURVE ( 3, ( #5797, #17084, #35572, #43469 ),
 .UNSPECIFIED., .F., .F. ) 
 B_SPLINE_CURVE_WITH_KNOTS ( ( 4, 4 ),
 ( 0.9074455897393701731, 1.000000000000000000 ),
 .UNSPECIFIED. ) 
 CURVE ( )  GEOMETRIC_REPRESENTATION_ITEM ( )  RATIONAL_B_SPLINE_CURVE ( ( 0.6983129098261056100, 0.7760317562607090824, 0.8765941196520071754, 1.000000000000000000 ) ) 
 REPRESENTATION_ITEM ( '' )  );
#40506 = EDGE_LOOP ( 'NONE', ( #3200, #35403, #48498, #18670, #3159 ) ) ;
#40507 = ADVANCED_FACE ( 'NONE', ( #11873 ), #41909, .T. ) ;
#40508 = CARTESIAN_POINT ( 'NONE',  ( -10.40277084706750621, -15.44444119821074501, 57.86792809062919218 ) ) ;
#40509 = PLANE ( 'NONE',  #24454 ) ;
#40510 = CARTESIAN_POINT ( 'NONE',  ( -10.13784000599894597, -13.25541019000276499, 74.79322239981686948 ) ) ;
#40511 = ORIENTED_EDGE ( 'NONE', *, *, #29378, .T. ) ;
#40512 = CARTESIAN_POINT ( 'NONE',  ( -11.22967194918012268, -11.54873428709711902, 67.61864634137779717 ) ) ;
#40513 = ORIENTED_EDGE ( 'NONE', *, *, #48695, .F. ) ;
#40514 = CARTESIAN_POINT ( 'NONE',  ( -22.46951418628932728, -9.956841189560520888, 73.48161090405926643 ) ) ;
#40515 = CARTESIAN_POINT ( 'NONE',  ( -24.83596929353047145, -14.05522739703532054, 73.24554619393663302 ) ) ;
#40516 = CARTESIAN_POINT ( 'NONE',  ( -18.72680718162379421, -7.880610904852766829, 70.67068030199192208 ) ) ;
#40517 = CARTESIAN_POINT ( 'NONE',  ( -17.12409385541300111, -9.359200813967566646, 50.49621490985766314 ) ) ;
#40518 = VERTEX_POINT ( 'NONE', #4471 ) ;
#40519 = CARTESIAN_POINT ( 'NONE',  ( -12.99758330771203951, -9.386476247090117297, 70.84925353123610137 ) ) ;
#40520 = LINE ( 'NONE', #29691, #33625 ) ;
#40521 = CYLINDRICAL_SURFACE ( 'NONE', #28213, 4.686499999999997002 ) ;
#40522 = CARTESIAN_POINT ( 'NONE',  ( -24.32752796592761158, -15.96791130369872391, 66.06324927019940674 ) ) ;
#40523 = VERTEX_POINT ( 'NONE', #11378 ) ;
#40524 = DIRECTION ( 'NONE',  ( -3.071710424422018668E-17, 6.404604876783312462E-16, 1.000000000000000000 ) ) ;
#40525 = DIRECTION ( 'NONE',  ( 0.9687793358424821033, -0.2479245821708677133, 0.000000000000000000 ) ) ;
#40526 = CARTESIAN_POINT ( 'NONE',  ( -10.71355325306214645, -11.57327142899409189, 71.28849651251223918 ) ) ;
#40527 = ORIENTED_EDGE ( 'NONE', *, *, #32729, .T. ) ;
#40528 = AXIS2_PLACEMENT_3D ( 'NONE', #31122, #26706, #23026 ) ;
#40529 = CARTESIAN_POINT ( 'NONE',  ( -11.72362823715024227, -10.74660985594761797, 74.54770848788524518 ) ) ;
#40530 = ORIENTED_EDGE ( 'NONE', *, *, #40554, .F. ) ;
#40531 = DIRECTION ( 'NONE',  ( -5.731567514496413899E-31, -1.020425574103664789E-16, -1.000000000000000000 ) ) ;
#40532 = CARTESIAN_POINT ( 'NONE',  ( -13.18904211892902367, -11.30002761096173280, 54.07175714974879099 ) ) ;
#40533 = DIRECTION ( 'NONE',  ( -0.3566357048164924826, 0.9342435303763381160, -8.054691247152028744E-09 ) ) ;
#40534 = CARTESIAN_POINT ( 'NONE',  ( -23.43742028209110373, -18.48928452435560743, 72.76368265771812105 ) ) ;
#40535 = ORIENTED_EDGE ( 'NONE', *, *, #29551, .T. ) ;
#40536 = CARTESIAN_POINT ( 'NONE',  ( -10.45863924090583552, -14.11462608630872317, 61.21821294130609914 ) ) ;
#40537 = CARTESIAN_POINT ( 'NONE',  ( -24.17899325218984785, -11.66673737571591296, 59.66731058339561855 ) ) ;
#40538 = CARTESIAN_POINT ( 'NONE',  ( -23.32531047696446080, -18.57448983302084855, 69.29371930760996179 ) ) ;
#40539 = ORIENTED_EDGE ( 'NONE', *, *, #44878, .F. ) ;
#40540 = DIRECTION ( 'NONE',  ( -0.4749924142254751680, -0.8799898899579781109, -8.916637576350562172E-09 ) ) ;
#40541 = DIRECTION ( 'NONE',  ( -2.866981220435666553E-17, 1.000000000000000000, 1.190614954331866791E-16 ) ) ;
#40542 = EDGE_CURVE ( 'NONE', #28192, #8859, #17711, .T. ) ;
#40543 = ORIENTED_EDGE ( 'NONE', *, *, #797, .T. ) ;
#40544 = ORIENTED_EDGE ( 'NONE', *, *, #40837, .T. ) ;
#40545 = CARTESIAN_POINT ( 'NONE',  ( -24.16575343130564590, -12.74704122656904914, 69.92243002240397232 ) ) ;
#40546 = DIRECTION ( 'NONE',  ( -3.071710424422018668E-17, 6.404604876783312462E-16, 1.000000000000000000 ) ) ;
#40547 = DIRECTION ( 'NONE',  ( 0.000000000000000000, 0.000000000000000000, 1.000000000000000000 ) ) ;
#40548 = CARTESIAN_POINT ( 'NONE',  ( -20.69509252757554307, -8.115601716887088202, 63.49616818922779515 ) ) ;
#40549 = CARTESIAN_POINT ( 'NONE',  ( -45.37196614242555626, -14.20920654474410760, 70.87000000000000455 ) ) ;
#40550 = CARTESIAN_POINT ( 'NONE',  ( -25.31403878743076774, -21.34684298153750603, 53.49999999999995026 ) ) ;
#40551 = DIRECTION ( 'NONE',  ( -0.1240347345892086200, 1.145860353393066553E-16, -0.9922778767136676281 ) ) ;
#40552 = ORIENTED_EDGE ( 'NONE', *, *, #12885, .T. ) ;
#40553 = ORIENTED_EDGE ( 'NONE', *, *, #21755, .F. ) ;
#40554 = EDGE_CURVE ( 'NONE', #31720, #24011, #7309, .T. ) ;
#40555 = DIRECTION ( 'NONE',  ( 0.2843796944294933460, 0.9587117342539337450, 5.205739956168971478E-08 ) ) ;
#40556 = EDGE_CURVE ( 'NONE', #40648, #30065, #12108, .T. ) ;
#40557 = FACE_OUTER_BOUND ( 'NONE', #36205, .T. ) ;
#40558 = CARTESIAN_POINT ( 'NONE',  ( -21.91378931226059024, -9.437005245162470857, 63.41983640775033848 ) ) ;
#40559 = CARTESIAN_POINT ( 'NONE',  ( -19.04042241193164386, -7.536568769452434147, 67.01576393362593365 ) ) ;
#40560 = CARTESIAN_POINT ( 'NONE',  ( -18.62265789082445622, -7.456197966475932581, 73.94790266681903290 ) ) ;
#40561 = EDGE_CURVE ( 'NONE', #44055, #32492, #39686, .T. ) ;
#40562 = ORIENTED_EDGE ( 'NONE', *, *, #14735, .T. ) ;
#40563 = CARTESIAN_POINT ( 'NONE',  ( -17.96784385650551741, -6.428312510596451368, 51.20221977374900035 ) ) ;
#40564 = AXIS2_PLACEMENT_3D ( 'NONE', #40450, #40688, #6725 ) ;
#40565 = EDGE_LOOP ( 'NONE', ( #3180, #21780, #9675, #14665 ) ) ;
#40566 = CARTESIAN_POINT ( 'NONE',  ( -12.69763806180496601, -20.04058448603118592, 68.62185382311069759 ) ) ;
#40567 = EDGE_CURVE ( 'NONE', #30495, #7670, #11621, .T. ) ;
#40568 = CARTESIAN_POINT ( 'NONE',  ( -12.00532783130394776, -19.33158900886926546, 58.07115174146640157 ) ) ;
#40569 = DIRECTION ( 'NONE',  ( -3.071710424422018668E-17, 6.404604876783312462E-16, 1.000000000000000000 ) ) ;
#40570 = EDGE_LOOP ( 'NONE', ( #16668, #48100, #41301, #26383 ) ) ;
#40571 = DIRECTION ( 'NONE',  ( 1.000000000000000000, 2.866981220435666553E-17, 0.000000000000000000 ) ) ;
#40572 = CARTESIAN_POINT ( 'NONE',  ( -21.62177555926896133, -9.207315420440883358, 66.66149954055094895 ) ) ;
#40573 = ORIENTED_EDGE ( 'NONE', *, *, #2901, .T. ) ;
#40574 = CARTESIAN_POINT ( 'NONE',  ( -15.11195812866605692, -21.41632606413040918, 65.10596681519622564 ) ) ;
#40575 = DIRECTION ( 'NONE',  ( 0.8037372918934696520, -0.5949843406508663612, -7.322964617522714932E-08 ) ) ;
#40576 = ORIENTED_EDGE ( 'NONE', *, *, #13897, .T. ) ;
#40577 = CARTESIAN_POINT ( 'NONE',  ( -20.87058525438150625, -20.90343409458096602, 65.81283875100656644 ) ) ;
#40578 = ORIENTED_EDGE ( 'NONE', *, *, #39724, .T. ) ;
#40579 = CARTESIAN_POINT ( 'NONE',  ( -23.85820194903862657, -17.69173191509663567, 62.48833042115954584 ) ) ;
#40580 = CARTESIAN_POINT ( 'NONE',  ( -11.50075376218807754, -18.54175998082050825, 64.81877447156344374 ) ) ;
#40581 = ORIENTED_EDGE ( 'NONE', *, *, #40832, .F. ) ;
#40582 = CARTESIAN_POINT ( 'NONE',  ( -13.71293426195967413, -21.26916566922604801, 68.64120525947689089 ) ) ;
#40583 = FACE_OUTER_BOUND ( 'NONE', #43191, .T. ) ;
#40584 = ORIENTED_EDGE ( 'NONE', *, *, #31976, .T. ) ;
#40585 = CARTESIAN_POINT ( 'NONE',  ( -20.02395964528090033, -18.70843468947691690, 52.02966884056656482 ) ) ;
#40586 = EDGE_CURVE ( 'NONE', #166, #35459, #27918, .T. ) ;
#40587 = CARTESIAN_POINT ( 'NONE',  ( -19.63995608841934626, -21.92282860479379991, 65.65141533869274326 ) ) ;
#40588 = CARTESIAN_POINT ( 'NONE',  ( -24.86203810447890561, -14.38333402024011143, 66.36009642219894999 ) ) ;
#40589 = ORIENTED_EDGE ( 'NONE', *, *, #5408, .F. ) ;
#40590 = CARTESIAN_POINT ( 'NONE',  ( -13.38462506958126141, -20.58719851387657940, 58.04650077714654088 ) ) ;
#40591 = VECTOR ( 'NONE', #31019, 1000.000000000000000 ) ;
#40592 = AXIS2_PLACEMENT_3D ( 'NONE', #28227, #5593, #42535 ) ;
#40593 = DIRECTION ( 'NONE',  ( -2.331190579393116502E-06, 8.511884082828543324E-06, -0.9999999999610567070 ) ) ;
#40594 = DIRECTION ( 'NONE',  ( -1.224646799147353207E-16, -1.000000000000000000, 1.912410701131276611E-32 ) ) ;
#40595 = ORIENTED_EDGE ( 'NONE', *, *, #44149, .F. ) ;
#40596 = EDGE_LOOP ( 'NONE', ( #24759, #32659, #39707, #17481, #25876 ) ) ;
#40597 = CARTESIAN_POINT ( 'NONE',  ( -23.37892143032667391, -10.33223586073257572, 59.79541750854375692 ) ) ;
#40598 = CARTESIAN_POINT ( 'NONE',  ( -11.90535080888287212, -10.50279376357651095, 70.96893075550114816 ) ) ;
#40599 = DIRECTION ( 'NONE',  ( -0.4156784896208465252, -0.1649587623211697662, 0.8944271909999157444 ) ) ;
#40600 = B_SPLINE_CURVE_WITH_KNOTS ( 'NONE', 1,
 ( #35575, #24756 ),
 .UNSPECIFIED., .F., .F.,
 ( 2, 2 ),
 ( 0.000000000000000000, 1.000000000000000000 ),
 .UNSPECIFIED. ) ;
#40601 = CARTESIAN_POINT ( 'NONE',  ( -15.29909385759798823, -8.105421454601382081, 49.25000573077640098 ) ) ;
#40602 = CARTESIAN_POINT ( 'NONE',  ( -17.42409385541300892, -14.80920654474439502, 75.49999999999994316 ) ) ;
#40603 = CARTESIAN_POINT ( 'NONE',  ( -13.06813783877040969, -9.265530354883374287, 67.66470656304637998 ) ) ;
#40604 = CARTESIAN_POINT ( 'NONE',  ( -15.62222905942472018, -7.993050613273783966, 70.89517703929612935 ) ) ;
#40605 = CARTESIAN_POINT ( 'NONE',  ( -27.42409385541305156, -14.65920654474411045, 52.21286476528344878 ) ) ;
#40606 = ORIENTED_EDGE ( 'NONE', *, *, #10591, .F. ) ;
#40607 = FACE_OUTER_BOUND ( 'NONE', #46936, .T. ) ;
#40608 =( NAMED_UNIT ( * ) PLANE_ANGLE_UNIT ( ) SI_UNIT ( $, .RADIAN. ) );
#40609 = EDGE_CURVE ( 'NONE', #43726, #2066, #46152, .T. ) ;
#40610 = DIRECTION ( 'NONE',  ( 2.342027643795563533E-48, 1.912410701131276611E-32, 1.000000000000000000 ) ) ;
#40611 = CARTESIAN_POINT ( 'NONE',  ( -13.46747890590686403, -9.034676489092227314, 60.43950277890026967 ) ) ;
#40612 = EDGE_CURVE ( 'NONE', #14770, #2068, #46813, .T. ) ;
#40613 = EDGE_LOOP ( 'NONE', ( #21935, #41784, #9300, #11250, #23489, #33040, #15632, #33521, #15924, #24858, #13162, #7058, #13341, #31893, #5926, #16989, #40513, #23289, #38828, #36630, #48363, #29611, #5402, #18149, #14815, #8084, #8060, #5242, #33291, #44719, #17798, #34759, #29456, #37581, #16011, #14639, #39257, #13819, #6464, #46901, #47710, #18606, #30108, #5677, #10740, #35767, #8063, #12284, #41213, #5688, #20922, #45207, #37763, #9042, #39036, #6309, #24348, #31344, #18685, #25892, #34169, #31871, #22253, #37770, #25323, #29349, #185, #6896, #19240, #38420, #30161, #14009 ) ) ;
#40614 = EDGE_CURVE ( 'NONE', #33854, #24550, #7435, .T. ) ;
#40615 = ORIENTED_EDGE ( 'NONE', *, *, #8824, .F. ) ;
#40616 = CARTESIAN_POINT ( 'NONE',  ( -20.70232273485035890, -8.624288160964143302, 60.14125250309182036 ) ) ;
#40617 = DIRECTION ( 'NONE',  ( -8.339041841313433703E-07, -7.401745998521586792E-06, 0.9999999999722594124 ) ) ;
#40618 = CARTESIAN_POINT ( 'NONE',  ( -15.93879930885702656, -7.917138641544857691, 67.15479422225767792 ) ) ;
#40619 = CARTESIAN_POINT ( 'NONE',  ( -11.41592704872699748, -19.21438508446953364, 71.94331831479362904 ) ) ;
#40620 = ADVANCED_FACE ( 'NONE', ( #20477 ), #42540, .T. ) ;
#40621 =( BOUNDED_CURVE ( )  B_SPLINE_CURVE ( 3, ( #6651, #21443, #6170, #10588 ),
 .UNSPECIFIED., .F., .F. ) 
 B_SPLINE_CURVE_WITH_KNOTS ( ( 4, 4 ),
 ( 0.000000000000000000, 0.4074455897393706727 ),
 .UNSPECIFIED. ) 
 CURVE ( )  GEOMETRIC_REPRESENTATION_ITEM ( )  RATIONAL_B_SPLINE_CURVE ( ( 1.000000000000000000, 0.4567392136813168690, 0.3561768502900247158, 0.6983129098261233736 ) ) 
 REPRESENTATION_ITEM ( '' )  );
#40622 = ORIENTED_EDGE ( 'NONE', *, *, #48391, .F. ) ;
#40623 = CARTESIAN_POINT ( 'NONE',  ( -24.06787342886325121, -18.28917680027896608, 53.49999999999994316 ) ) ;
#40624 = AXIS2_PLACEMENT_3D ( 'NONE', #36900, #18193, #33201 ) ;
#40625 = AXIS2_PLACEMENT_3D ( 'NONE', #43449, #47137, #1830 ) ;
#40626 = LINE ( 'NONE', #10121, #17040 ) ;
#40627 = ORIENTED_EDGE ( 'NONE', *, *, #8780, .F. ) ;
#40628 = CARTESIAN_POINT ( 'NONE',  ( -13.70633956305045409, -21.26533489984594283, 68.64899269501005108 ) ) ;
#40629 = AXIS2_PLACEMENT_3D ( 'NONE', #22536, #149, #41492 ) ;
#40630 = CARTESIAN_POINT ( 'NONE',  ( -12.55524250210389425, -20.44813591936859609, 71.91315377446979085 ) ) ;
#40631 = CARTESIAN_POINT ( 'NONE',  ( -14.91112529534803066, -8.221969756899694559, 57.13527940342243028 ) ) ;
#40632 =( BOUNDED_CURVE ( )  B_SPLINE_CURVE ( 3, ( #32186, #47678, #13445, #36341 ),
 .UNSPECIFIED., .F., .F. ) 
 B_SPLINE_CURVE_WITH_KNOTS ( ( 4, 4 ),
 ( 0.9074455897393706172, 1.000000000000000000 ),
 .UNSPECIFIED. ) 
 CURVE ( )  GEOMETRIC_REPRESENTATION_ITEM ( )  RATIONAL_B_SPLINE_CURVE ( ( 0.6983129098261082746, 0.7760317562607114139, 0.8765941196520086187, 1.000000000000000000 ) ) 
 REPRESENTATION_ITEM ( '' )  );
#40633 = ORIENTED_EDGE ( 'NONE', *, *, #24197, .F. ) ;
#40634 =( BOUNDED_CURVE ( )  B_SPLINE_CURVE ( 3, ( #490, #8360, #38374, #15968 ),
 .UNSPECIFIED., .F., .F. ) 
 B_SPLINE_CURVE_WITH_KNOTS ( ( 4, 4 ),
 ( 0.9074455897393635118, 1.000000000000000000 ),
 .UNSPECIFIED. ) 
 CURVE ( )  GEOMETRIC_REPRESENTATION_ITEM ( )  RATIONAL_B_SPLINE_CURVE ( ( 0.6983129098260831835, 0.7760317562606896535, 0.8765941196519952960, 1.000000000000000000 ) ) 
 REPRESENTATION_ITEM ( '' )  );
#40635 = CARTESIAN_POINT ( 'NONE',  ( -12.01648241349452917, -10.28590705807702932, 67.49896869922172016 ) ) ;
#40636 = ORIENTED_EDGE ( 'NONE', *, *, #28908, .T. ) ;
#40637 = CARTESIAN_POINT ( 'NONE',  ( -10.47154223249567728, -17.48601752977970492, 64.82013545767874518 ) ) ;
#40638 = CARTESIAN_POINT ( 'NONE',  ( -23.65624121974494898, -11.51332442490695307, 66.42214514605623776 ) ) ;
#40639 = ORIENTED_EDGE ( 'NONE', *, *, #45578, .F. ) ;
#40640 = DIRECTION ( 'NONE',  ( 0.9410372374137780938, 0.3383029970317210089, 1.029646055599927174E-09 ) ) ;
#40641 = CARTESIAN_POINT ( 'NONE',  ( -20.06975372951847447, -8.274133229585533655, 73.73568642813194174 ) ) ;
#40642 = CARTESIAN_POINT ( 'NONE',  ( -19.74284385650551599, -8.811426318492348031, 52.18089403414751359 ) ) ;
#40643 = DIRECTION ( 'NONE',  ( 4.116680954457742276E-07, 3.835121109574216710E-07, 0.9999999999998415712 ) ) ;
#40644 = ADVANCED_FACE ( 'NONE', ( #27612 ), #8911, .T. ) ;
#40645 = DIRECTION ( 'NONE',  ( -0.06357898915124167438, 0.9979768094191900918, 0.000000000000000000 ) ) ;
#40646 = CARTESIAN_POINT ( 'NONE',  ( -10.52422430310768320, -17.61911375464911700, 68.21226508126260057 ) ) ;
#40647 = CARTESIAN_POINT ( 'NONE',  ( -12.27604185553471616, -19.62628656662749549, 58.21210303282668264 ) ) ;
#40648 = VERTEX_POINT ( 'NONE', #23929 ) ;
#40649 = CARTESIAN_POINT ( 'NONE',  ( -24.87177708793343811, -14.62301390258337896, 62.81272869172535422 ) ) ;
#40650 =( BOUNDED_SURFACE ( )  B_SPLINE_SURFACE ( 3, 1, ( 
 ( #25858, #22175 ),
 ( #3444, #36435 ),
 ( #31627, #42944 ),
 ( #24244, #39250 ),
 ( #9467, #5532 ),
 ( #20551, #1824 ),
 ( #31862, #13122 ) ),
 .UNSPECIFIED., .T., .F., .F. ) 
 B_SPLINE_SURFACE_WITH_KNOTS ( ( 4, 3, 4 ),
 ( 2, 2 ),
 ( 0.000000000000000000, 0.5000000000000000000, 1.000000000000000000 ),
 ( 0.000000000000000000, 1.000000000000000000 ),
 .UNSPECIFIED. ) 
 GEOMETRIC_REPRESENTATION_ITEM ( )  RATIONAL_B_SPLINE_SURFACE ( (
 ( 1.000000000000000000, 1.000000000000000000),
 ( 0.3333333333333335369, 0.3333333333333330373),
 ( 0.3333333333333335369, 0.3333333333333330373),
 ( 1.000000000000000000, 1.000000000000000000),
 ( 0.3333333333333333703, 0.3333333333333333703),
 ( 0.3333333333333333703, 0.3333333333333333703),
 ( 1.000000000000000000, 1.000000000000000000) ) ) 
 REPRESENTATION_ITEM ( '' )  SURFACE ( )  );
#40651 = CARTESIAN_POINT ( 'NONE',  ( -10.43125892716163960, -13.91323834088958122, 57.44825034920751960 ) ) ;
#40652 = CARTESIAN_POINT ( 'NONE',  ( -22.69189081882976566, -20.07747925453471183, 69.35134909049985197 ) ) ;
#40653 = CYLINDRICAL_SURFACE ( 'NONE', #43119, 0.1500000000000043521 ) ;
#40654 = CARTESIAN_POINT ( 'NONE',  ( -13.49409790474204840, -20.66256726344224504, 61.53118467422925164 ) ) ;
#40655 = CARTESIAN_POINT ( 'NONE',  ( -24.29232374648589854, -16.16102685949518403, 62.89328677060923667 ) ) ;
#40656 = VERTEX_POINT ( 'NONE', #20216 ) ;
#40657 = ORIENTED_EDGE ( 'NONE', *, *, #37704, .T. ) ;
#40658 = CARTESIAN_POINT ( 'NONE',  ( -24.50093619861336336, -12.48040563361249333, 73.38192204494465898 ) ) ;
#40659 = CARTESIAN_POINT ( 'NONE',  ( -40.92409385541305511, -14.80920654474410725, 74.99999999999998579 ) ) ;
#40660 = ORIENTED_EDGE ( 'NONE', *, *, #12755, .T. ) ;
#40662 = CARTESIAN_POINT ( 'NONE',  ( -20.52631159502315938, -8.474406804437011331, 60.04945086230327433 ) ) ;
#40661 = DIRECTION ( 'NONE',  ( -0.9687793358424822143, 0.2479245821708672415, 0.000000000000000000 ) ) ;
#40663 = CARTESIAN_POINT ( 'NONE',  ( -21.23484681875272528, -20.74088929683185611, 69.33978048267414351 ) ) ;
#40664 = CARTESIAN_POINT ( 'NONE',  ( -21.80513198786261597, -9.285521334292361928, 63.48593961849922351 ) ) ;
#40665 = CARTESIAN_POINT ( 'NONE',  ( -12.51133688094842888, -19.86980477907010822, 61.28190024782882972 ) ) ;
#40666 = FACE_BOUND ( 'NONE', #23163, .T. ) ;
#40667 = EDGE_CURVE ( 'NONE', #21578, #24254, #6174, .T. ) ;
#40668 = CARTESIAN_POINT ( 'NONE',  ( -23.89968641036289299, -17.46782332651663339, 66.24357233134217893 ) ) ;
#40669 = VECTOR ( 'NONE', #7949, 1000.000000000000000 ) ;
#40670 = DIRECTION ( 'NONE',  ( -0.06357898915124166050, 0.9979768094191900918, 0.000000000000000000 ) ) ;
#40671 = AXIS2_PLACEMENT_3D ( 'NONE', #42171, #4993, #46825 ) ;
#40672 = CARTESIAN_POINT ( 'NONE',  ( -17.42260713176972686, -20.05920633423509258, 52.02966884056656482 ) ) ;
#40673 = ORIENTED_EDGE ( 'NONE', *, *, #39353, .F. ) ;
#40674 = CARTESIAN_POINT ( 'NONE',  ( -24.12706943888446887, -11.55726411819128785, 63.09184898997396829 ) ) ;
#40675 = CARTESIAN_POINT ( 'NONE',  ( -13.92409385541305511, -25.10920654474410441, 81.99999999999998579 ) ) ;
#40676 = EDGE_CURVE ( 'NONE', #18426, #44255, #36189, .T. ) ;
#40677 = CARTESIAN_POINT ( 'NONE',  ( -24.71152906796918458, -13.26113485863129071, 59.55606250353000775 ) ) ;
#40678 = VECTOR ( 'NONE', #28662, 1000.000000000000114 ) ;
#40679 = DIRECTION ( 'NONE',  ( 1.224646799147353207E-16, 1.000000000000000000, -1.912410701131276611E-32 ) ) ;
#40680 = FACE_OUTER_BOUND ( 'NONE', #37671, .T. ) ;
#40681 = CARTESIAN_POINT ( 'NONE',  ( -11.84468983566281608, -9.872329927957173012, 64.17914326340513753 ) ) ;
#40682 = CARTESIAN_POINT ( 'NONE',  ( -16.51570212919159530, -21.75045681730355795, 65.50947872143868267 ) ) ;
#40683 = VERTEX_POINT ( 'NONE', #16516 ) ;
#40684 = VERTEX_POINT ( 'NONE', #42881 ) ;
#40685 = CARTESIAN_POINT ( 'NONE',  ( -15.66159385541304339, -7.228003583438117552, 51.38655588711986155 ) ) ;
#40686 = ADVANCED_FACE ( 'NONE', ( #9147 ), #13539, .T. ) ;
#40687 = ORIENTED_EDGE ( 'NONE', *, *, #34330, .T. ) ;
#40688 = DIRECTION ( 'NONE',  ( -0.000000000000000000, 1.000000000000000000, -0.000000000000000000 ) ) ;
#40689 = CARTESIAN_POINT ( 'NONE',  ( -26.42409385541305511, -6.859206544744110623, 50.50000000000000000 ) ) ;
#40690 = ADVANCED_FACE ( 'NONE', ( #1992 ), #39367, .T. ) ;
#40691 = CARTESIAN_POINT ( 'NONE',  ( -24.61377439452271076, -12.85684087295677891, 66.49585060569550876 ) ) ;
#40692 = CARTESIAN_POINT ( 'NONE',  ( -16.16379340615718618, -22.15191857530921382, 58.47080845268740035 ) ) ;
#40693 = ORIENTED_EDGE ( 'NONE', *, *, #18591, .T. ) ;
#40694 = CARTESIAN_POINT ( 'NONE',  ( -40.92409385541305511, -15.80920654474410725, 74.99999999999998579 ) ) ;
#40695 = VECTOR ( 'NONE', #33538, 1000.000000000000000 ) ;
#40696 = CARTESIAN_POINT ( 'NONE',  ( -22.09234465700630423, -20.09219189623108548, 62.23439162498055310 ) ) ;
#40697 = ORIENTED_EDGE ( 'NONE', *, *, #28705, .T. ) ;
#40698 = B_SPLINE_CURVE_WITH_KNOTS ( 'NONE', 3,
 ( #19902, #34908, #46007, #1906, #24328, #34670, #28005, #1175, #31221, #12262 ),
 .UNSPECIFIED., .F., .F.,
 ( 4, 2, 2, 2, 4 ),
 ( 0.1272669073658189987, 0.2522669073463225109, 0.3772669073268261064, 0.5022669073073295909, 0.6272669072878331864 ),
 .UNSPECIFIED. ) ;
#40699 = CARTESIAN_POINT ( 'NONE',  ( -26.42409385541305511, -8.109206544744111511, 49.25000000000000000 ) ) ;
#40700 = ADVANCED_FACE ( 'NONE', ( #25600 ), #27191, .F. ) ;
#40701 = LINE ( 'NONE', #6980, #18839 ) ;
#40702 = ADVANCED_FACE ( 'NONE', ( #28816 ), #17715, .T. ) ;
#40703 = AXIS2_PLACEMENT_3D ( 'NONE', #13914, #39320, #21095 ) ;
#40704 = EDGE_CURVE ( 'NONE', #40683, #1179, #44107, .T. ) ;
#40705 = ORIENTED_EDGE ( 'NONE', *, *, #12216, .T. ) ;
#40706 = CARTESIAN_POINT ( 'NONE',  ( -17.82542875633258106, -7.370011655844420417, 60.18086518042608901 ) ) ;
#40707 = CARTESIAN_POINT ( 'NONE',  ( -11.07356217608303695, -11.86355251018914991, 74.84223526849542907 ) ) ;
#40708 = CARTESIAN_POINT ( 'NONE',  ( -23.38313847423633263, -10.33780256150599541, 59.85849373767491954 ) ) ;
#40709 = EDGE_CURVE ( 'NONE', #8636, #46413, #44410, .T. ) ;
#40710 = ORIENTED_EDGE ( 'NONE', *, *, #35921, .T. ) ;
#40711 = CARTESIAN_POINT ( 'NONE',  ( -11.10681587527927938, -11.67891925637714223, 71.10332952723315714 ) ) ;
#40712 = CARTESIAN_POINT ( 'NONE',  ( -24.41841346439724347, -17.37497344050957437, 69.45693887357894880 ) ) ;
#40713 = AXIS2_PLACEMENT_3D ( 'NONE', #24259, #45935, #12195 ) ;
#40714 = CARTESIAN_POINT ( 'NONE',  ( -10.68602809008750576, -16.88409676349039046, 57.70232650191087487 ) ) ;
#40715 = DIRECTION ( 'NONE',  ( 0.8447509909909733938, -0.5351595679979650466, 0.000000000000000000 ) ) ;
#40716 = VERTEX_POINT ( 'NONE', #40151 ) ;
#40717 = LINE ( 'NONE', #6992, #33651 ) ;
#40718 = AXIS2_PLACEMENT_3D ( 'NONE', #32554, #47355, #28627 ) ;
#40719 = DIRECTION ( 'NONE',  ( 0.1240347345892083841, 0.000000000000000000, 0.9922778767136676281 ) ) ;
#40720 = CARTESIAN_POINT ( 'NONE',  ( -11.42962537269896117, -10.38539323336976494, 74.62380298385740218 ) ) ;
#40721 = B_SPLINE_CURVE_WITH_KNOTS ( 'NONE', 3,
 ( #35639, #20149, #35159, #20402, #12987, #13219, #31957, #35405, #12765, #27779 ),
 .UNSPECIFIED., .F., .F.,
 ( 4, 2, 2, 2, 4 ),
 ( 0.000000000000000000, 0.2500000000000000000, 0.5000000000000000000, 0.7500000000000000000, 1.000000000000000000 ),
 .UNSPECIFIED. ) ;
#40722 = VERTEX_POINT ( 'NONE', #29540 ) ;
#40723 = CARTESIAN_POINT ( 'NONE',  ( -46.29409385541305966, -14.20920654474410760, 70.91501325280044910 ) ) ;
#40724 = CARTESIAN_POINT ( 'NONE',  ( -14.41428275390769365, -7.994163218335415877, 63.97474169571218283 ) ) ;
#40725 = EDGE_LOOP ( 'NONE', ( #38716, #18070, #14271, #9956 ) ) ;
#40726 = CARTESIAN_POINT ( 'NONE',  ( -11.32138995524401182, -19.08233857334280970, 68.31665992013745381 ) ) ;
#40727 = DIRECTION ( 'NONE',  ( -3.071710424422018668E-17, 6.404604876783312462E-16, 1.000000000000000000 ) ) ;
#40728 = DIRECTION ( 'NONE',  ( 1.000000000000000000, -4.164305804376849788E-17, 1.614929280266638808E-16 ) ) ;
#40729 = ORIENTED_EDGE ( 'NONE', *, *, #41275, .T. ) ;
#40730 = DIRECTION ( 'NONE',  ( -5.731567514496413899E-31, -1.020425574103664789E-16, -1.000000000000000000 ) ) ;
#40731 = EDGE_LOOP ( 'NONE', ( #32587, #4852, #43309, #48476, #2562 ) ) ;
#40732 = ORIENTED_EDGE ( 'NONE', *, *, #34835, .T. ) ;
#40733 = ORIENTED_EDGE ( 'NONE', *, *, #35384, .T. ) ;
#40734 = CARTESIAN_POINT ( 'NONE',  ( -19.65534385650552451, -7.417179338643134834, 52.18511593390279302 ) ) ;
#40735 = CARTESIAN_POINT ( 'NONE',  ( -14.40713916828295460, -8.490940588968131308, 70.91884656573979839 ) ) ;
#40736 = VECTOR ( 'NONE', #29593, 1000.000000000000000 ) ;
#40737 = CARTESIAN_POINT ( 'NONE',  ( -10.90759852523040507, -17.49952041063523822, 68.09721944423129969 ) ) ;
#40738 = CARTESIAN_POINT ( 'NONE',  ( -21.94242186726961208, -9.397052521110282441, 60.00699132926281010 ) ) ;
#40739 = CARTESIAN_POINT ( 'NONE',  ( -12.79487214375358839, -8.971058656907512585, 71.03580700614087107 ) ) ;
#40740 = AXIS2_PLACEMENT_3D ( 'NONE', #29762, #23112, #40831 ) ;
#40741 = AXIS2_PLACEMENT_3D ( 'NONE', #21301, #42973, #47405 ) ;
#40742 = EDGE_LOOP ( 'NONE', ( #19908, #3754, #23763, #26316, #45196 ) ) ;
#40743 = ORIENTED_EDGE ( 'NONE', *, *, #48695, .T. ) ;
#40744 = CARTESIAN_POINT ( 'NONE',  ( -13.49909385650551563, -8.114302828567740988, 52.18300498402516041 ) ) ;
#40745 = EDGE_CURVE ( 'NONE', #31233, #15954, #30335, .T. ) ;
#40746 = CARTESIAN_POINT ( 'NONE',  ( 18.54465614458695910, 0.6410078225857483991, 50.44245483349490655 ) ) ;
#40747 = AXIS2_PLACEMENT_3D ( 'NONE', #38415, #34480, #1235 ) ;
#40748 = CARTESIAN_POINT ( 'NONE',  ( -23.45031237530261947, -11.14340064005916098, 70.10030580274290912 ) ) ;
#40749 = CARTESIAN_POINT ( 'NONE',  ( -20.19284385650551528, -7.406986770994973490, 48.81910596585309747 ) ) ;
#40750 = ORIENTED_EDGE ( 'NONE', *, *, #47455, .T. ) ;
#40751 = CARTESIAN_POINT ( 'NONE',  ( -10.72530867274958410, -17.00760959713300835, 57.97288447305809456 ) ) ;
#40752 = DIRECTION ( 'NONE',  ( 0.9687793358424821033, -0.2479245821708677133, 0.000000000000000000 ) ) ;
#40753 = DIRECTION ( 'NONE',  ( 0.000000000000000000, 0.000000000000000000, -1.000000000000000000 ) ) ;
#40754 = ORIENTED_EDGE ( 'NONE', *, *, #675, .F. ) ;
#40755 = CARTESIAN_POINT ( 'NONE',  ( -11.27324709396361335, -11.46480877714557778, 67.69034896821969483 ) ) ;
#40756 = ADVANCED_FACE ( 'NONE', ( #10361 ), #3684, .T. ) ;
#40757 = ORIENTED_EDGE ( 'NONE', *, *, #8334, .T. ) ;
#40758 = CARTESIAN_POINT ( 'NONE',  ( -7.334870405450504727, -11.98365049024292972, 53.49999999999995026 ) ) ;
#40759 = LINE ( 'NONE', #45212, #44653 ) ;
#40760 = ADVANCED_FACE ( 'NONE', ( #21444 ), #14253, .T. ) ;
#40762 = EDGE_CURVE ( 'NONE', #25517, #43113, #36427, .T. ) ;
#40761 = CARTESIAN_POINT ( 'NONE',  ( -10.12326218194131044, -13.32541594658350448, 74.86312942357149325 ) ) ;
#40763 = CARTESIAN_POINT ( 'NONE',  ( -17.57409385541300395, -6.859212275519753099, 50.50378509014294792 ) ) ;
#40764 = VERTEX_POINT ( 'NONE', #17954 ) ;
#40765 = CARTESIAN_POINT ( 'NONE',  ( -11.12943539273130611, -10.82423919798514689, 57.30928973319082331 ) ) ;
#40766 = VECTOR ( 'NONE', #46561, 1000.000000000000000 ) ;
#40767 = CARTESIAN_POINT ( 'NONE',  ( -24.42401512115494455, -14.72416081258524834, 62.72913071971822063 ) ) ;
#40768 = AXIS2_PLACEMENT_3D ( 'NONE', #10421, #40442, #29119 ) ;
#40769 = CARTESIAN_POINT ( 'NONE',  ( -19.44376929052122449, -7.638105555415076076, 60.07597592072836790 ) ) ;
#40770 = CARTESIAN_POINT ( 'NONE',  ( -42.79688797306011594, -14.80920654474413745, 60.01764705882352047 ) ) ;
#40771 = ORIENTED_EDGE ( 'NONE', *, *, #30139, .F. ) ;
#40772 = LINE ( 'NONE', #22553, #48015 ) ;
#40773 = VECTOR ( 'NONE', #895, 1000.000000000000227 ) ;
#40775 = CARTESIAN_POINT ( 'NONE',  ( -12.65090885562174350, -19.92943164506675657, 64.97561006052195864 ) ) ;
#40774 = VECTOR ( 'NONE', #2489, 1000.000000000000114 ) ;
#40776 = ORIENTED_EDGE ( 'NONE', *, *, #38567, .F. ) ;
#40777 = FACE_BOUND ( 'NONE', #7332, .T. ) ;
#40778 = ORIENTED_EDGE ( 'NONE', *, *, #38718, .F. ) ;
#40779 = CARTESIAN_POINT ( 'NONE',  ( -17.21153000696512336, -19.50285887057015444, 49.52966884056656482 ) ) ;
#40780 = CARTESIAN_POINT ( 'NONE',  ( -13.43447785487663637, -11.00382355316531147, 53.88362224778187226 ) ) ;
#40781 = LINE ( 'NONE', #22560, #15566 ) ;
#40782 = CARTESIAN_POINT ( 'NONE',  ( -21.56016804333223646, -8.612711131324969571, 73.64482796973915413 ) ) ;
#40783 = VERTEX_POINT ( 'NONE', #32970 ) ;
#40784 = CARTESIAN_POINT ( 'NONE',  ( -10.53028993777715883, -16.28642212234895226, 71.73278239416407587 ) ) ;
#40785 = ORIENTED_EDGE ( 'NONE', *, *, #42083, .F. ) ;
#40786 = PLANE ( 'NONE',  #6971 ) ;
#40787 =( BOUNDED_CURVE ( )  B_SPLINE_CURVE ( 3, ( #40115, #13972, #43573, #9836 ),
 .UNSPECIFIED., .F., .F. ) 
 B_SPLINE_CURVE_WITH_KNOTS ( ( 4, 4 ),
 ( 0.5000000000000000000, 0.9074455897393635118 ),
 .UNSPECIFIED. ) 
 CURVE ( )  GEOMETRIC_REPRESENTATION_ITEM ( )  RATIONAL_B_SPLINE_CURVE ( ( 1.000000000000000888, 0.4567392136813381853, 0.3561768502900318212, 0.6983129098260827394 ) ) 
 REPRESENTATION_ITEM ( '' )  );
#40788 = PLANE ( 'NONE',  #43214 ) ;
#40789 = ORIENTED_EDGE ( 'NONE', *, *, #12268, .F. ) ;
#40790 = CARTESIAN_POINT ( 'NONE',  ( -16.16379449968008331, -22.15191876840708929, 58.47080954035841671 ) ) ;
#40791 = CARTESIAN_POINT ( 'NONE',  ( -13.44724237933888134, -20.56996776775315183, 58.34650027598461719 ) ) ;
#40792 = EDGE_CURVE ( 'NONE', #27869, #34125, #8887, .T. ) ;
#40793 = VERTEX_POINT ( 'NONE', #6894 ) ;
#40794 = VERTEX_POINT ( 'NONE', #21910 ) ;
#40795 = FACE_OUTER_BOUND ( 'NONE', #14161, .T. ) ;
#40796 = CARTESIAN_POINT ( 'NONE',  ( -20.67761229128902656, -8.545853924536821467, 66.92536870251414882 ) ) ;
#40797 = CARTESIAN_POINT ( 'NONE',  ( -20.82184643845504723, -8.178298495136663959, 63.49776821231386492 ) ) ;
#40798 = CARTESIAN_POINT ( 'NONE',  ( -21.25156111013253835, -21.20098409628925396, 65.70641164036103987 ) ) ;
#40799 = CARTESIAN_POINT ( 'NONE',  ( -14.16498672988215191, -8.109065889264286398, 70.91612917212019340 ) ) ;
#40800 = CARTESIAN_POINT ( 'NONE',  ( -14.73375560093340120, -21.75656996136207866, 61.75105004614717785 ) ) ;
#40801 =( BOUNDED_SURFACE ( )  B_SPLINE_SURFACE ( 3, 1, ( 
 ( #9456, #6241 ),
 ( #17776, #21732 ),
 ( #28646, #35772 ),
 ( #24481, #25432 ),
 ( #39486, #28879 ),
 ( #47115, #18016 ),
 ( #36259, #17301 ) ),
 .UNSPECIFIED., .T., .F., .F. ) 
 B_SPLINE_SURFACE_WITH_KNOTS ( ( 4, 3, 4 ),
 ( 2, 2 ),
 ( 0.000000000000000000, 0.5000000000000000000, 1.000000000000000000 ),
 ( 0.000000000000000000, 1.000000000000000000 ),
 .UNSPECIFIED. ) 
 GEOMETRIC_REPRESENTATION_ITEM ( )  RATIONAL_B_SPLINE_SURFACE ( (
 ( 1.000000000000000000, 1.000000000000000000),
 ( 0.3333333333333335369, 0.3333333333333330373),
 ( 0.3333333333333335369, 0.3333333333333330373),
 ( 1.000000000000000000, 1.000000000000000000),
 ( 0.3333333333333333703, 0.3333333333333333703),
 ( 0.3333333333333333703, 0.3333333333333333703),
 ( 1.000000000000000000, 1.000000000000000000) ) ) 
 REPRESENTATION_ITEM ( '' )  SURFACE ( )  );
#40802 = ORIENTED_EDGE ( 'NONE', *, *, #24628, .T. ) ;
#40803 = VERTEX_POINT ( 'NONE', #33451 ) ;
#40804 = EDGE_CURVE ( 'NONE', #18527, #25029, #20119, .T. ) ;
#40805 = DIRECTION ( 'NONE',  ( -3.071710424422018668E-17, 6.404604876783312462E-16, 1.000000000000000000 ) ) ;
#40806 = VECTOR ( 'NONE', #47802, 1000.000000000000000 ) ;
#40807 = PLANE ( 'NONE',  #37791 ) ;
#40808 = PLANE ( 'NONE',  #47670 ) ;
#40809 = LINE ( 'NONE', #7094, #42542 ) ;
#40810 = AXIS2_PLACEMENT_3D ( 'NONE', #36910, #48244, #48488 ) ;
#40811 = VERTEX_POINT ( 'NONE', #48489 ) ;
#40812 = CARTESIAN_POINT ( 'NONE',  ( -19.43034385650552309, -9.794322478646142471, 51.19202720610083901 ) ) ;
#40813 = VECTOR ( 'NONE', #34015, 1000.000000000000000 ) ;
#40814 = CIRCLE ( 'NONE', #14846, 6.899999999999997691 ) ;
#40815 = VERTEX_POINT ( 'NONE', #3195 ) ;
#40816 = CARTESIAN_POINT ( 'NONE',  ( -22.00056318799662591, -20.10656996550254050, 62.25055788910309218 ) ) ;
#40817 = CARTESIAN_POINT ( 'NONE',  ( -12.27604185553471616, -19.62628656662749549, 58.21210303282668264 ) ) ;
#40818 = CARTESIAN_POINT ( 'NONE',  ( -15.95285335075216970, -19.84884456522215146, 50.77966884056656482 ) ) ;
#40819 = AXIS2_PLACEMENT_3D ( 'NONE', #16430, #2391, #9556 ) ;
#40820 = B_SPLINE_CURVE_WITH_KNOTS ( 'NONE', 3,
 ( #31353, #23746, #16563, #11924, #20277, #41958, #15838, #39226, #8463, #1303 ),
 .UNSPECIFIED., .F., .F.,
 ( 4, 2, 2, 2, 4 ),
 ( 0.000000000000000000, 0.2500000000000000000, 0.5000000000000000000, 0.7500000000000000000, 1.000000000000000000 ),
 .UNSPECIFIED. ) ;
#40821 = VERTEX_POINT ( 'NONE', #18204 ) ;
#40822 = DIRECTION ( 'NONE',  ( 1.000000000000000000, -0.000000000000000000, -0.000000000000000000 ) ) ;
#40823 = CARTESIAN_POINT ( 'NONE',  ( -21.54616816135207813, -9.151524939380248469, 66.88823273622162446 ) ) ;
#40824 = EDGE_CURVE ( 'NONE', #3267, #8796, #33211, .T. ) ;
#40825 = VERTEX_POINT ( 'NONE', #29796 ) ;
#40826 = CARTESIAN_POINT ( 'NONE',  ( -15.24014793263337531, -21.45986350121160058, 65.33270079998744961 ) ) ;
#40827 = CARTESIAN_POINT ( 'NONE',  ( -9.424093855413055110, -25.10920654474410441, 56.99999999999997868 ) ) ;
#40828 = ORIENTED_EDGE ( 'NONE', *, *, #26167, .T. ) ;
#40829 = CARTESIAN_POINT ( 'NONE',  ( -19.04784696903935881, -9.816619457272704352, 50.77966884056655772 ) ) ;
#40830 = VERTEX_POINT ( 'NONE', #44827 ) ;
#40831 = DIRECTION ( 'NONE',  ( 0.3688590060343596155, -0.9294853595766554566, 0.000000000000000000 ) ) ;
#40832 = EDGE_CURVE ( 'NONE', #4358, #35167, #11080, .T. ) ;
#40833 = EDGE_CURVE ( 'NONE', #18877, #31039, #42048, .T. ) ;
#40834 = PLANE ( 'NONE',  #34306 ) ;
#40835 = ORIENTED_EDGE ( 'NONE', *, *, #6694, .T. ) ;
#40836 = CARTESIAN_POINT ( 'NONE',  ( -12.84691039585993444, -8.931012183600500975, 67.56438067310742213 ) ) ;
#40837 = EDGE_CURVE ( 'NONE', #2827, #15007, #14985, .T. ) ;
#40838 = CARTESIAN_POINT ( 'NONE',  ( -16.50454536406711981, -22.20232556258728351, 65.34068991928313608 ) ) ;
#40839 = VECTOR ( 'NONE', #26817, 1000.000000000000227 ) ;
#40840 = EDGE_LOOP ( 'NONE', ( #45067, #6181, #46398, #30974 ) ) ;
#40841 = CARTESIAN_POINT ( 'NONE',  ( -13.71339110807025641, -20.80363600241853561, 65.13628881288371986 ) ) ;
#40842 = EDGE_CURVE ( 'NONE', #26529, #35577, #47559, .T. ) ;
#40843 = CARTESIAN_POINT ( 'NONE',  ( -19.67760665824181388, -21.48965406232008490, 65.75014118398131302 ) ) ;
#40844 = CYLINDRICAL_SURFACE ( 'NONE', #46342, 4.686499999999997002 ) ;
#40845 = ORIENTED_EDGE ( 'NONE', *, *, #36924, .T. ) ;
#40846 = DIRECTION ( 'NONE',  ( 0.000000000000000000, -0.000000000000000000, -1.000000000000000000 ) ) ;
#40847 = AXIS2_PLACEMENT_3D ( 'NONE', #16679, #39344, #38616 ) ;
#40848 = VECTOR ( 'NONE', #28400, 1000.000000000000000 ) ;
#40849 = CARTESIAN_POINT ( 'NONE',  ( -11.38016085489450901, -11.27755116225183230, 60.67885732596114678 ) ) ;
#40850 = EDGE_CURVE ( 'NONE', #33575, #45950, #13845, .T. ) ;
#40851 = ORIENTED_EDGE ( 'NONE', *, *, #11581, .F. ) ;
#40852 = EDGE_LOOP ( 'NONE', ( #25988, #31032, #24699, #21532 ) ) ;
#40853 = CARTESIAN_POINT ( 'NONE',  ( -12.96596534320165794, -9.347742485070138940, 70.84925352874383009 ) ) ;
#40854 = CARTESIAN_POINT ( 'NONE',  ( -24.66733291767277692, -16.55538881886969804, 59.30987817879385915 ) ) ;
#40855 = DIRECTION ( 'NONE',  ( 1.000000000000000000, 2.866981220435666553E-17, 0.000000000000000000 ) ) ;
#40856 = VECTOR ( 'NONE', #46857, 1000.000000000000000 ) ;
#40857 = CARTESIAN_POINT ( 'NONE',  ( -15.01784385759799356, -6.860780111191487229, 51.02154966934377711 ) ) ;
#40858 = CARTESIAN_POINT ( 'NONE',  ( -23.25757715627672795, -10.17517474196413474, 63.18690702823881367 ) ) ;
#40859 = CARTESIAN_POINT ( 'NONE',  ( -16.78865592400587659, -21.78030535593112305, 68.99560651886281448 ) ) ;
#40860 = CARTESIAN_POINT ( 'NONE',  ( -23.93648101794248362, -17.51022725521227841, 65.95829288617392194 ) ) ;
#40861 = PLANE ( 'NONE',  #16616 ) ;
#40862 = ORIENTED_EDGE ( 'NONE', *, *, #23553, .T. ) ;
#40863 = CARTESIAN_POINT ( 'NONE',  ( -24.31482381427648676, -13.31912605980313735, 59.36267924676594987 ) ) ;
#40864 = CIRCLE ( 'NONE', #32233, 2.000000000000000444 ) ;
#40865 = DIRECTION ( 'NONE',  ( -1.148482744091818979E-06, 2.957121237693701878E-08, 0.9999999999993399724 ) ) ;
#40866 = DIRECTION ( 'NONE',  ( -3.071710424422018668E-17, 6.404604876783312462E-16, 1.000000000000000000 ) ) ;
#40867 = VERTEX_POINT ( 'NONE', #30052 ) ;
#40868 = ORIENTED_EDGE ( 'NONE', *, *, #1578, .F. ) ;
#40869 = DIRECTION ( 'NONE',  ( 2.866981220435666553E-17, -1.000000000000000000, -1.190614954331866791E-16 ) ) ;
#40870 = CARTESIAN_POINT ( 'NONE',  ( -24.85884029783971982, -14.32113974155904046, 66.29637463883811677 ) ) ;
#40871 = AXIS2_PLACEMENT_3D ( 'NONE', #1049, #565, #4028 ) ;
#40872 = CARTESIAN_POINT ( 'NONE',  ( -15.37142651463144460, -21.97085505939421779, 72.14551830437926583 ) ) ;
#40873 = CARTESIAN_POINT ( 'NONE',  ( -11.65600162890749303, -18.86286912916044400, 68.51689600618566089 ) ) ;
#40874 = ADVANCED_FACE ( 'NONE', ( #26336 ), #30295, .T. ) ;
#40875 = VERTEX_POINT ( 'NONE', #256 ) ;
#40876 = VECTOR ( 'NONE', #16195, 1000.000000000000000 ) ;
#40877 = CARTESIAN_POINT ( 'NONE',  ( -23.54032652647746104, -11.40454826030700808, 66.61317707917329756 ) ) ;
#40878 = CARTESIAN_POINT ( 'NONE',  ( -10.39215594834096024, -14.30487625923878880, 64.53803863383089379 ) ) ;
#40879 = EDGE_CURVE ( 'NONE', #46319, #34661, #43803, .T. ) ;
#40880 = ORIENTED_EDGE ( 'NONE', *, *, #5131, .F. ) ;
#40881 = CARTESIAN_POINT ( 'NONE',  ( -50.42609385541305755, -14.90920654474414775, 61.92352941176469727 ) ) ;
#40882 = VECTOR ( 'NONE', #24093, 1000.000000000000227 ) ;
#40883 = CARTESIAN_POINT ( 'NONE',  ( -22.17153284776674482, -17.05070671513899683, 49.52966884056655772 ) ) ;
#40884 = CARTESIAN_POINT ( 'NONE',  ( -24.38756562526642213, -15.91227465074932290, 66.34852784166324113 ) ) ;
#40885 = EDGE_LOOP ( 'NONE', ( #23603, #10441, #23129, #9927 ) ) ;
#40886 = CARTESIAN_POINT ( 'NONE',  ( -13.51659408464697698, -24.65568926594394128, 53.49999999999995026 ) ) ;
#40887 = ORIENTED_EDGE ( 'NONE', *, *, #13012, .T. ) ;
#40888 = CARTESIAN_POINT ( 'NONE',  ( -24.38143503755601316, -15.58083059521001168, 73.30303748419844112 ) ) ;
#40889 = CARTESIAN_POINT ( 'NONE',  ( -15.38020936669038008, -6.822612233742264110, 53.49999999999995026 ) ) ;
#40890 = ORIENTED_EDGE ( 'NONE', *, *, #26673, .T. ) ;
#40891 = CARTESIAN_POINT ( 'NONE',  ( -21.43532435649834866, -21.08734459619973123, 69.19303634238183065 ) ) ;
#40892 = CARTESIAN_POINT ( 'NONE',  ( -10.64854695470030599, -12.86019059820356958, 64.55364013863997741 ) ) ;
#40893 = EDGE_CURVE ( 'NONE', #33146, #14550, #39066, .T. ) ;
#40894 = CARTESIAN_POINT ( 'NONE',  ( -22.10534385650552025, -8.801233750844183135, 48.81488406609782515 ) ) ;
#40895 = DIRECTION ( 'NONE',  ( 0.9687793358424821033, -0.2479245821708680464, 0.000000000000000000 ) ) ;
#40896 = EDGE_CURVE ( 'NONE', #9377, #6262, #40634, .T. ) ;
#40897 = LINE ( 'NONE', #7186, #13282 ) ;
#40898 = CARTESIAN_POINT ( 'NONE',  ( -6.424093855413055110, -27.10920654474410796, 47.99999999999998579 ) ) ;
#40899 = DIRECTION ( 'NONE',  ( 0.3124635249310678264, 0.8422251632096483531, 0.4393441931380604459 ) ) ;
#40900 = ORIENTED_EDGE ( 'NONE', *, *, #7163, .T. ) ;
#40901 = CARTESIAN_POINT ( 'NONE',  ( -46.46711114793018282, -12.76354662275040219, 70.13000000000000966 ) ) ;
#40902 = DIRECTION ( 'NONE',  ( 0.000000000000000000, 0.9999954153791273948, 0.003028072113820366902 ) ) ;
#40903 = DIRECTION ( 'NONE',  ( 0.9687793358424821033, -0.2479245821708679909, 0.000000000000000000 ) ) ;
#40904 = DIRECTION ( 'NONE',  ( -3.071710424422018668E-17, 6.404604876783312462E-16, 1.000000000000000000 ) ) ;
#40905 = ORIENTED_EDGE ( 'NONE', *, *, #17608, .F. ) ;
#40906 = EDGE_LOOP ( 'NONE', ( #42508, #39395 ) ) ;
#40907 = AXIS2_PLACEMENT_3D ( 'NONE', #21460, #22185, #29324 ) ;
#40908 = CARTESIAN_POINT ( 'NONE',  ( -11.14144638094932382, -18.81445342923831987, 61.39055447797494480 ) ) ;
#40909 = CARTESIAN_POINT ( 'NONE',  ( -10.52215087187021325, -13.37195826583270986, 74.67817647370830514 ) ) ;
#40910 = ORIENTED_EDGE ( 'NONE', *, *, #10973, .T. ) ;
#40912 = CARTESIAN_POINT ( 'NONE',  ( -13.55534385650551243, -7.417179338643134834, 52.18511593390279302 ) ) ;
#40911 = CARTESIAN_POINT ( 'NONE',  ( -24.02655244371635845, -11.35792869308308717, 66.53719207489109522 ) ) ;
#40913 = CARTESIAN_POINT ( 'NONE',  ( -28.42409385541305511, -6.859206544744110623, 47.99999999999997868 ) ) ;
#40914 = CIRCLE ( 'NONE', #47977, 5.249999999999998224 ) ;
#40915 = FACE_OUTER_BOUND ( 'NONE', #31073, .T. ) ;
#40916 = CARTESIAN_POINT ( 'NONE',  ( -14.78766009005058812, -21.34800739930362568, 58.45145834864037937 ) ) ;
#40917 = ADVANCED_FACE ( 'NONE', ( #7887 ), #30368, .F. ) ;
#40918 = CARTESIAN_POINT ( 'NONE',  ( -24.72725712452650981, -16.28144042551206638, 62.84974626185121593 ) ) ;
#40919 = CARTESIAN_POINT ( 'NONE',  ( -19.05047292022263505, -10.41396213884962840, 49.52966884056655772 ) ) ;
#40920 = AXIS2_PLACEMENT_3D ( 'NONE', #42212, #5033, #27676 ) ;
#40921 = LINE ( 'NONE', #3488, #33408 ) ;
#40922 = PRODUCT_DEFINITION_SHAPE ( 'NONE', 'NONE',  #18332 ) ;
#40923 = CARTESIAN_POINT ( 'NONE',  ( -16.42344266294433908, -21.79157980633116054, 58.28585275688816836 ) ) ;
#40924 = ORIENTED_EDGE ( 'NONE', *, *, #28908, .F. ) ;
#40925 = CARTESIAN_POINT ( 'NONE',  ( -14.04638888798549701, -8.616795679365674587, 70.72957572181515218 ) ) ;
#40926 = CARTESIAN_POINT ( 'NONE',  ( -10.23569597183452728, -12.85201410577908732, 67.99478283741052564 ) ) ;
#40927 = AXIS2_PLACEMENT_3D ( 'NONE', #8477, #19815, #38753 ) ;
#40928 = CARTESIAN_POINT ( 'NONE',  ( -24.71334378318632830, -13.26952680650525274, 59.47772536435775947 ) ) ;
#40929 = CARTESIAN_POINT ( 'NONE',  ( -24.27425269666204244, -13.36807298356958817, 59.66267976136047935 ) ) ;
#40930 = CARTESIAN_POINT ( 'NONE',  ( 6.575906144586949331, -6.109215713985405749, 50.50605614422795497 ) ) ;
#40931 =( BOUNDED_CURVE ( )  B_SPLINE_CURVE ( 3, ( #24856, #39627, #44308, #32252 ),
 .UNSPECIFIED., .F., .F. ) 
 B_SPLINE_CURVE_WITH_KNOTS ( ( 4, 4 ),
 ( 0.5000000000000000000, 0.9074455897393751691 ),
 .UNSPECIFIED. ) 
 CURVE ( )  GEOMETRIC_REPRESENTATION_ITEM ( )  RATIONAL_B_SPLINE_CURVE ( ( 0.9999999999999952260, 0.4567392136813065440, 0.3561768502900240496, 0.6983129098261426915 ) ) 
 REPRESENTATION_ITEM ( '' )  );
#40932 = CARTESIAN_POINT ( 'NONE',  ( -11.51143670280680986, -18.65567654335754355, 68.51689928321519574 ) ) ;
#40933 = CARTESIAN_POINT ( 'NONE',  ( -23.82366728017863622, -10.99486018697619372, 73.47698013610775547 ) ) ;
#40934 = ORIENTED_EDGE ( 'NONE', *, *, #16565, .F. ) ;
#40935 = EDGE_LOOP ( 'NONE', ( #42565, #30995, #24005, #8154 ) ) ;
#40936 = CARTESIAN_POINT ( 'NONE',  ( -13.80534385541303877, -7.595227055684746986, 51.75156210489594599 ) ) ;
#40937 = ORIENTED_EDGE ( 'NONE', *, *, #5687, .T. ) ;
#40938 = CYLINDRICAL_SURFACE ( 'NONE', #13841, 0.1500000000000045186 ) ;
#40939 = AXIS2_PLACEMENT_3D ( 'NONE', #156, #45449, #29941 ) ;
#40940 = CARTESIAN_POINT ( 'NONE',  ( -18.90223155190902915, -7.506551502853892721, 67.01416387246997886 ) ) ;
#40941 = EDGE_CURVE ( 'NONE', #38177, #40280, #17734, .T. ) ;
#40942 =( BOUNDED_CURVE ( )  B_SPLINE_CURVE ( 3, ( #14165, #10742, #40780, #40532 ),
 .UNSPECIFIED., .F., .F. ) 
 B_SPLINE_CURVE_WITH_KNOTS ( ( 4, 4 ),
 ( 4.712388980384689674, 4.921828490624010399 ),
 .UNSPECIFIED. ) 
 CURVE ( )  GEOMETRIC_REPRESENTATION_ITEM ( )  RATIONAL_B_SPLINE_CURVE ( ( 1.000000000000000000, 0.9963479302455154896, 0.9963479302455154896, 1.000000000000000000 ) ) 
 REPRESENTATION_ITEM ( '' )  );
#40943 = CIRCLE ( 'NONE', #23672, 1.749999999999997558 ) ;
#40944 = CARTESIAN_POINT ( 'NONE',  ( -24.60930328113607501, -12.84061010741178066, 66.50257946727398917 ) ) ;
#40945 = CARTESIAN_POINT ( 'NONE',  ( -15.62101046192594289, -7.580605815997546237, 70.72494447658496597 ) ) ;
#40946 = ORIENTED_EDGE ( 'NONE', *, *, #25630, .T. ) ;
#40947 = VECTOR ( 'NONE', #13515, 999.9999999999998863 ) ;
#40948 = LINE ( 'NONE', #15306, #9546 ) ;
#40949 = LINE ( 'NONE', #7721, #18656 ) ;
#40950 = EDGE_LOOP ( 'NONE', ( #41865, #45313, #46658, #40924, #32248 ) ) ;
#40951 = CARTESIAN_POINT ( 'NONE',  ( -10.37462440636232053, -14.89569459299594634, 75.09778901493891112 ) ) ;
#40952 = AXIS2_PLACEMENT_3D ( 'NONE', #16156, #30968, #46474 ) ;
#40953 = DIRECTION ( 'NONE',  ( -6.471065199890530885E-06, -1.909039593073236381E-06, 0.9999999999772404280 ) ) ;
#40954 =( BOUNDED_CURVE ( )  B_SPLINE_CURVE ( 3, ( #23725, #39198, #12135, #27639 ),
 .UNSPECIFIED., .F., .F. ) 
 B_SPLINE_CURVE_WITH_KNOTS ( ( 4, 4 ),
 ( 0.000000000000000000, 0.4074455897393634562 ),
 .UNSPECIFIED. ) 
 CURVE ( )  GEOMETRIC_REPRESENTATION_ITEM ( )  RATIONAL_B_SPLINE_CURVE ( ( 1.000000000000000000, 0.4567392136813290815, 0.3561768502900292122, 0.6983129098261003920 ) ) 
 REPRESENTATION_ITEM ( '' )  );
#40955 = EDGE_LOOP ( 'NONE', ( #37035, #38983, #22197, #22128, #34140 ) ) ;
#40956 = CARTESIAN_POINT ( 'NONE',  ( 18.87590614458706995, 1.890747609047893185, 50.53028072113869484 ) ) ;
#40957 = CARTESIAN_POINT ( 'NONE',  ( -14.98927377128267047, -8.246306944878837086, 57.14999999999994884 ) ) ;
#40958 = CARTESIAN_POINT ( 'NONE',  ( -42.93585856129541156, -14.80920654474411613, 58.90588235294116970 ) ) ;
#40959 = ORIENTED_EDGE ( 'NONE', *, *, #47650, .T. ) ;
#40960 = CARTESIAN_POINT ( 'NONE',  ( -11.97137584462052828, -19.88590378904827460, 58.06535876572594645 ) ) ;
#40961 = EDGE_CURVE ( 'NONE', #31485, #10695, #44127, .T. ) ;
#40962 = CARTESIAN_POINT ( 'NONE',  ( -15.65237751681051570, -7.981625683898254664, 67.14006984041519388 ) ) ;
#40963 = VECTOR ( 'NONE', #39364, 1000.000000000000114 ) ;
#40964 = EDGE_CURVE ( 'NONE', #48084, #11232, #37902, .T. ) ;
#40965 = CARTESIAN_POINT ( 'NONE',  ( -24.72409385541305582, -14.80920654474427423, 73.99411764705880046 ) ) ;
#40966 = CARTESIAN_POINT ( 'NONE',  ( -10.55090139406780558, -17.68373120125836806, 68.14076041135473361 ) ) ;
#40967 = EDGE_LOOP ( 'NONE', ( #25216, #33905, #47758, #9794, #2432 ) ) ;
#40968 = CARTESIAN_POINT ( 'NONE',  ( -10.58771178721467798, -11.84651422905517926, 74.67185031923813199 ) ) ;
#40969 = DIRECTION ( 'NONE',  ( 0.9687793358424821033, -0.2479245821708677133, 0.000000000000000000 ) ) ;
#40970 = CARTESIAN_POINT ( 'NONE',  ( -19.49109506855409180, -21.54969648977046148, 62.28031529404344013 ) ) ;
#40971 = PLANE ( 'NONE',  #39980 ) ;
#40972 = ADVANCED_FACE ( 'NONE', ( #23635 ), #18689, .T. ) ;
#40973 = CARTESIAN_POINT ( 'NONE',  ( -20.94909385650551670, -8.104110260919577868, 48.81699501597546487 ) ) ;
#40974 = AXIS2_PLACEMENT_3D ( 'NONE', #11968, #31394, #39020 ) ;
#40975 = ORIENTED_EDGE ( 'NONE', *, *, #27377, .F. ) ;
#40976 = CARTESIAN_POINT ( 'NONE',  ( -17.72612443559818018, -7.765381109175947927, 60.36588690973874094 ) ) ;
#40977 = CARTESIAN_POINT ( 'NONE',  ( -45.36595154876284397, -14.19714313411803985, 70.52197034960535404 ) ) ;
#40978 = EDGE_LOOP ( 'NONE', ( #23077, #9511, #38694, #42040, #15868 ) ) ;
#40979 = CARTESIAN_POINT ( 'NONE',  ( -18.52415950777489684, -7.896185818571675341, 74.14064402152244782 ) ) ;
#40980 = EDGE_CURVE ( 'NONE', #22485, #44170, #23827, .T. ) ;
#40981 = CARTESIAN_POINT ( 'NONE',  ( -22.60138646627221348, -10.09559420857893741, 73.67088087145607744 ) ) ;
#40982 = CARTESIAN_POINT ( 'NONE',  ( -11.72709874728437107, -10.00842693884592549, 67.69235173591077626 ) ) ;
#40983 = ORIENTED_EDGE ( 'NONE', *, *, #17444, .F. ) ;
#40984 = CYLINDRICAL_SURFACE ( 'NONE', #37280, 0.1500000000000029088 ) ;
#40985 = VECTOR ( 'NONE', #29803, 1000.000000000000000 ) ;
#40986 = CARTESIAN_POINT ( 'NONE',  ( -14.61429364226973782, -21.70915942589378744, 58.28805155203381361 ) ) ;
#40987 = ORIENTED_EDGE ( 'NONE', *, *, #30655, .T. ) ;
#40988 = VERTEX_POINT ( 'NONE', #35172 ) ;
#40989 = CARTESIAN_POINT ( 'NONE',  ( -16.33659385650551599, -6.915538690918074494, 49.31353937987644542 ) ) ;
#40990 = CIRCLE ( 'NONE', #47289, 0.4000000000000010214 ) ;
#40991 = CARTESIAN_POINT ( 'NONE',  ( -21.67230677980763431, -11.72453687863643523, 50.77966884056655772 ) ) ;
#40992 = CARTESIAN_POINT ( 'NONE',  ( 18.82590614458706924, 1.890747609047893185, 50.53028072113869484 ) ) ;
#40993 = DIRECTION ( 'NONE',  ( 3.071710424422018668E-17, -6.404604876783312462E-16, -1.000000000000000000 ) ) ;
#40994 = ADVANCED_FACE ( 'NONE', ( #13234 ), #20163, .T. ) ;
#40995 = CARTESIAN_POINT ( 'NONE',  ( -22.04909385759799179, -8.112991634885936776, 51.74999426922421719 ) ) ;
#40996 = AXIS2_PLACEMENT_3D ( 'NONE', #33466, #33716, #44123 ) ;
#40997 = EDGE_CURVE ( 'NONE', #15954, #29084, #44522, .T. ) ;
#40998 = ORIENTED_EDGE ( 'NONE', *, *, #24031, .T. ) ;
#40999 = ORIENTED_EDGE ( 'NONE', *, *, #15531, .T. ) ;
#41000 = CARTESIAN_POINT ( 'NONE',  ( -13.17364594312814852, -9.395205385347631832, 49.41430265251966603 ) ) ;
#41001 = CARTESIAN_POINT ( 'NONE',  ( -11.48094281790512738, -10.31654952874404962, 74.57851759402076652 ) ) ;
#41002 = AXIS2_PLACEMENT_3D ( 'NONE', #29548, #32521, #3204 ) ;
#41003 = CARTESIAN_POINT ( 'NONE',  ( -16.06050865347321732, -9.480920197610746669, 54.07175714974878389 ) ) ;
#41004 = EDGE_CURVE ( 'NONE', #10587, #24671, #2057, .T. ) ;
#41005 = CARTESIAN_POINT ( 'NONE',  ( -15.52409385650551421, -6.426201560718813433, 50.50509628382439331 ) ) ;
#41006 = ORIENTED_EDGE ( 'NONE', *, *, #38145, .T. ) ;
#41007 = CARTESIAN_POINT ( 'NONE',  ( -16.44703096029287437, -9.650926977002853846, 50.77966884056655772 ) ) ;
#41008 = AXIS2_PLACEMENT_3D ( 'NONE', #15141, #33122, #22307 ) ;
#41009 = CARTESIAN_POINT ( 'NONE',  ( -10.48067351556794158, -16.03044098841782628, 68.27767830705533925 ) ) ;
#41010 = FACE_OUTER_BOUND ( 'NONE', #35985, .T. ) ;
#41011 = ORIENTED_EDGE ( 'NONE', *, *, #26194, .T. ) ;
#41012 = CARTESIAN_POINT ( 'NONE',  ( -9.939267784769082681, -14.33236412611010913, 53.49999999999994316 ) ) ;
#41013 = ORIENTED_EDGE ( 'NONE', *, *, #42763, .T. ) ;
#41014 = CARTESIAN_POINT ( 'NONE',  ( -12.95699726224880699, -8.846094125884357950, 64.02291131566488502 ) ) ;
#41015 = CARTESIAN_POINT ( 'NONE',  ( -19.52605192831022407, -21.48662393483848376, 65.74869660756507983 ) ) ;
#41016 = CARTESIAN_POINT ( 'NONE',  ( -17.42409385541299471, -14.80920654474435594, 52.02966884056656482 ) ) ;
#41017 = CARTESIAN_POINT ( 'NONE',  ( -9.990077291455589759, -14.31953385297554071, 64.56520754649302773 ) ) ;
#41018 = AXIS2_PLACEMENT_3D ( 'NONE', #1857, #5567, #35578 ) ;
#41019 = VERTEX_POINT ( 'NONE', #24835 ) ;
#41020 = CARTESIAN_POINT ( 'NONE',  ( -17.91610874870965020, -22.24302035646641684, 62.13181838639658139 ) ) ;
#41021 = CARTESIAN_POINT ( 'NONE',  ( -24.72409385541305582, -14.80920654474412679, 59.01176470588234224 ) ) ;
#41022 = PLANE ( 'NONE',  #16388 ) ;
#41023 = DIRECTION ( 'NONE',  ( 0.9862050927915949616, 0.1655279884246635413, 7.765682856207886445E-08 ) ) ;
#41024 = ORIENTED_EDGE ( 'NONE', *, *, #13550, .F. ) ;
#41025 = CARTESIAN_POINT ( 'NONE',  ( -22.99015471925471843, -19.14192088663603997, 62.44587121756105574 ) ) ;
#41026 = CARTESIAN_POINT ( 'NONE',  ( -24.69822963474414479, -13.19963333263893190, 59.54763306486673713 ) ) ;
#41027 = LINE ( 'NONE', #7310, #43555 ) ;
#41028 = EDGE_LOOP ( 'NONE', ( #8116, #39192, #31422, #2143 ) ) ;
#41029 = DIRECTION ( 'NONE',  ( 0.000000000000000000, 1.000000000000000000, -0.000000000000000000 ) ) ;
#41031 = ORIENTED_EDGE ( 'NONE', *, *, #31433, .F. ) ;
#41030 = EDGE_CURVE ( 'NONE', #2787, #15048, #48487, .T. ) ;
#41032 = CYLINDRICAL_SURFACE ( 'NONE', #46279, 0.1499999999999987454 ) ;
#41033 = CARTESIAN_POINT ( 'NONE',  ( -13.70219457171530841, -20.73773636609404036, 61.70749392003438061 ) ) ;
#41034 = CARTESIAN_POINT ( 'NONE',  ( -24.41779626044834828, -14.51093891981887651, 62.78584623703071799 ) ) ;
#41035 = EDGE_CURVE ( 'NONE', #18330, #38687, #19107, .T. ) ;
#41036 = CARTESIAN_POINT ( 'NONE',  ( -14.70534385541304800, -7.595227055684751427, 51.75156210489594599 ) ) ;
#41037 = ORIENTED_EDGE ( 'NONE', *, *, #35816, .T. ) ;
#41038 = CARTESIAN_POINT ( 'NONE',  ( -10.13226805943771858, -16.33660356775173739, 71.49104427242312454 ) ) ;
#41039 = VECTOR ( 'NONE', #10194, 1000.000000000000227 ) ;
#41040 = ORIENTED_EDGE ( 'NONE', *, *, #47434, .T. ) ;
#41041 = FACE_OUTER_BOUND ( 'NONE', #33836, .T. ) ;
#41042 = DIRECTION ( 'NONE',  ( 0.9687793358424821033, -0.2479245821708680464, 0.000000000000000000 ) ) ;
#41043 = CARTESIAN_POINT ( 'NONE',  ( -24.34138250757122535, -16.17068267630804002, 62.89328676667767581 ) ) ;
#41044 = ORIENTED_EDGE ( 'NONE', *, *, #48683, .T. ) ;
#41045 = CARTESIAN_POINT ( 'NONE',  ( -21.53861886228549949, -21.02004079589906027, 72.63951149839988375 ) ) ;
#41046 = CARTESIAN_POINT ( 'NONE',  ( -23.05807922735651161, -10.57113180461529822, 59.60203456339924344 ) ) ;
#41047 = ORIENTED_EDGE ( 'NONE', *, *, #25562, .T. ) ;
#41048 = EDGE_LOOP ( 'NONE', ( #15873, #21484, #32371, #13991 ) ) ;
#41049 = DIRECTION ( 'NONE',  ( 0.9562635972186041000, -0.2925062950340273638, 4.666065131241568958E-08 ) ) ;
#41050 = CARTESIAN_POINT ( 'NONE',  ( -22.28902059852239503, -19.84295448483234736, 69.45801383501738258 ) ) ;
#41051 = CARTESIAN_POINT ( 'NONE',  ( -19.38982564003701725, -21.99536589193390412, 58.66360838363829799 ) ) ;
#41052 = CARTESIAN_POINT ( 'NONE',  ( -10.03904597514415009, -13.82694077737217242, 57.56329639008353638 ) ) ;
#41053 = ADVANCED_FACE ( 'NONE', ( #16933 ), #31738, .T. ) ;
#41054 = CARTESIAN_POINT ( 'NONE',  ( -14.13370316840849483, -8.630624890407778693, 74.19954649408759906 ) ) ;
#41055 = EDGE_CURVE ( 'NONE', #14468, #20890, #7964, .T. ) ;
#41056 = VERTEX_POINT ( 'NONE', #5396 ) ;
#41057 = ORIENTED_EDGE ( 'NONE', *, *, #25902, .T. ) ;
#41058 = CARTESIAN_POINT ( 'NONE',  ( -17.38762135442090795, -7.756298984960698917, 63.43568405917763897 ) ) ;
#41059 = EDGE_CURVE ( 'NONE', #31013, #20972, #9589, .T. ) ;
#41060 = EDGE_CURVE ( 'NONE', #31825, #46443, #46099, .T. ) ;
#41061 = EDGE_CURVE ( 'NONE', #28368, #26240, #46528, .T. ) ;
#41062 = AXIS2_PLACEMENT_3D ( 'NONE', #11935, #34077, #7019 ) ;
#41063 = DIRECTION ( 'NONE',  ( -3.071710424422018668E-17, 6.404604876783312462E-16, 1.000000000000000000 ) ) ;
#41064 = CARTESIAN_POINT ( 'NONE',  ( -11.57789998141014820, -10.19135890511387110, 71.11893103769725144 ) ) ;
#41065 = CARTESIAN_POINT ( 'NONE',  ( -27.42409385541305511, -25.10920654474410441, 63.99999999999998579 ) ) ;
#41066 = ORIENTED_EDGE ( 'NONE', *, *, #20153, .F. ) ;
#41067 = CARTESIAN_POINT ( 'NONE',  ( -15.54909385650551634, -8.104110260919579645, 48.81699501597546487 ) ) ;
#41068 = ORIENTED_EDGE ( 'NONE', *, *, #2858, .F. ) ;
#41069 = DIRECTION ( 'NONE',  ( -2.866981220435666553E-17, 1.000000000000000000, 1.190614954331866791E-16 ) ) ;
#41070 = LINE ( 'NONE', #11278, #35534 ) ;
#41071 = CARTESIAN_POINT ( 'NONE',  ( -10.38863864971416184, -14.24588297309210816, 57.60391932725825370 ) ) ;
#41072 = EDGE_LOOP ( 'NONE', ( #20498, #31007, #26941, #27871, #33539 ) ) ;
#41073 = PLANE ( 'NONE',  #36828 ) ;
#41074 = CARTESIAN_POINT ( 'NONE',  ( -10.53028993777715883, -16.28642212234895226, 71.73278239416407587 ) ) ;
#41075 = CARTESIAN_POINT ( 'NONE',  ( -21.53594150109643834, -20.54048459808615235, 72.52446133926662242 ) ) ;
#41076 = ADVANCED_FACE ( 'NONE', ( #12530 ), #400, .T. ) ;
#41077 = ORIENTED_EDGE ( 'NONE', *, *, #16820, .F. ) ;
#41078 = DIRECTION ( 'NONE',  ( -0.9999247414263408018, 0.01226831216845469807, 5.367905339378915168E-08 ) ) ;
#41079 =( BOUNDED_CURVE ( )  B_SPLINE_CURVE ( 3, ( #19526, #31336, #34534, #15324 ),
 .UNSPECIFIED., .F., .F. ) 
 B_SPLINE_CURVE_WITH_KNOTS ( ( 4, 4 ),
 ( 0.9074455897393685078, 1.000000000000000000 ),
 .UNSPECIFIED. ) 
 CURVE ( )  GEOMETRIC_REPRESENTATION_ITEM ( )  RATIONAL_B_SPLINE_CURVE ( ( 0.6983129098261100509, 0.7760317562607128572, 0.8765941196520095069, 1.000000000000000000 ) ) 
 REPRESENTATION_ITEM ( '' )  );
#41080 = CARTESIAN_POINT ( 'NONE',  ( -17.42409385541299471, -14.80920654474435771, 49.52966884056655772 ) ) ;
#41081 = ORIENTED_EDGE ( 'NONE', *, *, #22285, .F. ) ;
#41082 = CARTESIAN_POINT ( 'NONE',  ( -10.51956558245075080, -15.96174594004655312, 64.73444859219196701 ) ) ;
#41083 = ORIENTED_EDGE ( 'NONE', *, *, #29163, .T. ) ;
#41084 = PLANE ( 'NONE',  #610 ) ;
#41085 = CARTESIAN_POINT ( 'NONE',  ( -24.31057894323393143, -16.31947677049899781, 59.41772612388854924 ) ) ;
#41086 = VERTEX_POINT ( 'NONE', #46274 ) ;
#41087 = FACE_OUTER_BOUND ( 'NONE', #5149, .T. ) ;
#41088 = CARTESIAN_POINT ( 'NONE',  ( -18.97054302448013985, -7.521389842619064403, 67.08567168106696954 ) ) ;
#41089 = ORIENTED_EDGE ( 'NONE', *, *, #47053, .T. ) ;
#41090 = CARTESIAN_POINT ( 'NONE',  ( -4.424093855413056886, -6.859206544744110623, 47.99999999999998579 ) ) ;
#41091 = DIRECTION ( 'NONE',  ( 0.09855345062332551698, 0.9951317587989213509, 3.188559572831062401E-08 ) ) ;
#41092 = CARTESIAN_POINT ( 'NONE',  ( -21.62985240417965827, -8.659687547922406026, 73.76275303717041254 ) ) ;
#41093 = ORIENTED_EDGE ( 'NONE', *, *, #19086, .F. ) ;
#41094 = CARTESIAN_POINT ( 'NONE',  ( -36.42409385541304800, -8.109206544743658540, 50.50000000000030553 ) ) ;
#41095 =( BOUNDED_CURVE ( )  B_SPLINE_CURVE ( 3, ( #38131, #15229, #45797, #38366 ),
 .UNSPECIFIED., .F., .F. ) 
 B_SPLINE_CURVE_WITH_KNOTS ( ( 4, 4 ),
 ( 0.9074455897393632897, 1.000000000000000000 ),
 .UNSPECIFIED. ) 
 CURVE ( )  GEOMETRIC_REPRESENTATION_ITEM ( )  RATIONAL_B_SPLINE_CURVE ( ( 0.6983129098260925094, 0.7760317562606977582, 0.8765941196520002920, 1.000000000000000000 ) ) 
 REPRESENTATION_ITEM ( '' )  );
#41096 = CARTESIAN_POINT ( 'NONE',  ( -10.44202778021669609, -14.30845378979165794, 64.68803863533310050 ) ) ;
#41097 = CARTESIAN_POINT ( 'NONE',  ( -10.08672033063305840, -16.09972936581058889, 68.12767827759553541 ) ) ;
#41098 = VERTEX_POINT ( 'NONE', #32691 ) ;
#41099 = EDGE_LOOP ( 'NONE', ( #13161, #29463, #45966, #22089 ) ) ;
#41100 = PLANE ( 'NONE',  #4738 ) ;
#41101 = CARTESIAN_POINT ( 'NONE',  ( -19.57409385759799036, -6.859212275519751323, 50.50378509014259265 ) ) ;
#41102 = B_SPLINE_CURVE_WITH_KNOTS ( 'NONE', 3,
 ( #39908, #9651, #29065, #24422, #6427, #20718, #6659, #44113, #10117, #25379 ),
 .UNSPECIFIED., .F., .F.,
 ( 4, 2, 2, 2, 4 ),
 ( 0.000000000000000000, 0.2500000000000000000, 0.5000000000000000000, 0.7500000000000000000, 1.000000000000000000 ),
 .UNSPECIFIED. ) ;
#41103 = FACE_OUTER_BOUND ( 'NONE', #40570, .T. ) ;
#41104 = ORIENTED_EDGE ( 'NONE', *, *, #37328, .F. ) ;
#41105 = CARTESIAN_POINT ( 'NONE',  ( -15.24284385759798788, -7.587656875400194068, 49.25157356644813689 ) ) ;
#41106 = CARTESIAN_POINT ( 'NONE',  ( -24.42668993457695592, -13.99045928592870958, 73.40799407547365263 ) ) ;
#41107 = DIRECTION ( 'NONE',  ( -1.000000000000000000, 0.000000000000000000, 0.000000000000000000 ) ) ;
#41108 = CARTESIAN_POINT ( 'NONE',  ( -24.31883679440356261, -17.63164986302842152, 66.20003142906764992 ) ) ;
#41109 = CARTESIAN_POINT ( 'NONE',  ( -17.17596094306194487, -7.763534178167762256, 70.79035842408370627 ) ) ;
#41110 = ORIENTED_EDGE ( 'NONE', *, *, #38974, .T. ) ;
#41111 = CARTESIAN_POINT ( 'NONE',  ( -14.65765131015531253, -21.78034674156931061, 54.27966884056655061 ) ) ;
#41112 = ADVANCED_FACE ( 'NONE', ( #17666 ), #28764, .F. ) ;
#41113 = EDGE_CURVE ( 'NONE', #17561, #6337, #5190, .T. ) ;
#41114 = B_SPLINE_CURVE_WITH_KNOTS ( 'NONE', 3,
 ( #29398, #22494, #2802, #30143, #29155, #37008, #3529, #48342, #40472, #37491 ),
 .UNSPECIFIED., .F., .F.,
 ( 4, 2, 2, 2, 4 ),
 ( 0.000000000000000000, 0.2500000000000000000, 0.5000000000000000000, 0.7500000000000000000, 1.000000000000000000 ),
 .UNSPECIFIED. ) ;
#41115 = CARTESIAN_POINT ( 'NONE',  ( -14.60689809042302834, -8.346551666329650843, 64.08978840692947188 ) ) ;
#41116 = CARTESIAN_POINT ( 'NONE',  ( -13.49987391503245426, -9.012479888650673843, 60.43950329012445621 ) ) ;
#41117 = B_SPLINE_CURVE_WITH_KNOTS ( 'NONE', 1,
 ( #4692, #19716 ),
 .UNSPECIFIED., .F., .F.,
 ( 2, 2 ),
 ( 0.000000000000000000, 1.000000000000000000 ),
 .UNSPECIFIED. ) ;
#41118 = VERTEX_POINT ( 'NONE', #25794 ) ;
#41119 = EDGE_CURVE ( 'NONE', #6698, #32393, #6359, .T. ) ;
#41120 = EDGE_CURVE ( 'NONE', #22754, #16663, #37306, .T. ) ;
#41121 = ORIENTED_EDGE ( 'NONE', *, *, #19302, .T. ) ;
#41122 = CARTESIAN_POINT ( 'NONE',  ( -12.36794914932409561, -19.72224030764921565, 61.39678633597973345 ) ) ;
#41123 = CARTESIAN_POINT ( 'NONE',  ( -10.64449958474462932, -13.06134669730016995, 71.43658536801360981 ) ) ;
#41124 = CARTESIAN_POINT ( 'NONE',  ( -11.68224399338930297, -10.06205091296609488, 67.62084114930100043 ) ) ;
#41125 = CYLINDRICAL_SURFACE ( 'NONE', #38240, 0.1500000000000035194 ) ;
#41126 = EDGE_LOOP ( 'NONE', ( #40562, #13413, #40862, #9001, #19119 ) ) ;
#41127 = CARTESIAN_POINT ( 'NONE',  ( -23.61204160381034711, -11.53669949605622769, 66.42214514747726639 ) ) ;
#41128 = CARTESIAN_POINT ( 'NONE',  ( -14.28769015366465567, -8.051497000463099241, 67.51620991724109899 ) ) ;
#41129 = EDGE_CURVE ( 'NONE', #10747, #32823, #685, .T. ) ;
#41130 = VERTEX_POINT ( 'NONE', #39844 ) ;
#41131 = CARTESIAN_POINT ( 'NONE',  ( -22.24652905638778577, -19.95594847178128362, 62.11950460074248781 ) ) ;
#41132 = CARTESIAN_POINT ( 'NONE',  ( -11.25989433568915032, -11.38792842781904469, 64.44882039367774951 ) ) ;
#41133 = CARTESIAN_POINT ( 'NONE',  ( -24.78881009142557090, -15.93819564886128148, 66.17669525438618905 ) ) ;
#41134 = VERTEX_POINT ( 'NONE', #6111 ) ;
#41135 = CARTESIAN_POINT ( 'NONE',  ( -17.43688372600657743, -7.809108077429288919, 67.02039585984587688 ) ) ;
#41136 = EDGE_LOOP ( 'NONE', ( #39912, #16225 ) ) ;
#41137 = CARTESIAN_POINT ( 'NONE',  ( -22.78262153964987036, -19.98509753430224833, 72.90046450679021461 ) ) ;
#41138 = CARTESIAN_POINT ( 'NONE',  ( -19.47283698296378418, -21.55511232968401814, 62.28943840551588806 ) ) ;
#41139 = ORIENTED_EDGE ( 'NONE', *, *, #27239, .F. ) ;
#41140 = CARTESIAN_POINT ( 'NONE',  ( -16.58751391467172098, -21.80939466075598077, 65.52564390317479592 ) ) ;
#41141 = CARTESIAN_POINT ( 'NONE',  ( -9.908656216309283948, -19.57032361137281384, 53.49999999999995026 ) ) ;
#41142 = VECTOR ( 'NONE', #6014, 1000.000000000000000 ) ;
#41143 = CARTESIAN_POINT ( 'NONE',  ( -19.79909385650551457, -8.114302828567740988, 52.18300498402516041 ) ) ;
#41144 = CARTESIAN_POINT ( 'NONE',  ( -21.35639191854221508, -21.13703508191276015, 69.17733319344661425 ) ) ;
#41145 = CARTESIAN_POINT ( 'NONE',  ( -13.97958029355460852, -17.98703734140009303, 52.02966884056656482 ) ) ;
#41146 = CARTESIAN_POINT ( 'NONE',  ( -13.72409385759798894, -9.359200813967568422, 50.49621490985803263 ) ) ;
#41147 = PLANE ( 'NONE',  #47876 ) ;
#41148 = ORIENTED_EDGE ( 'NONE', *, *, #2044, .F. ) ;
#41149 = CARTESIAN_POINT ( 'NONE',  ( -12.18719842096713357, -10.08886484896570934, 64.04386393395434141 ) ) ;
#41150 = CARTESIAN_POINT ( 'NONE',  ( -11.39127492490111315, -11.16067319722467843, 60.69357916181100876 ) ) ;
#41151 = DIRECTION ( 'NONE',  ( -3.071710424422018668E-17, 6.404604876783312462E-16, 1.000000000000000000 ) ) ;
#41152 = DIRECTION ( 'NONE',  ( 0.000000000000000000, -0.9999954153791273948, -0.003028072113819836944 ) ) ;
#41153 = LINE ( 'NONE', #7683, #21176 ) ;
#41154 = LINE ( 'NONE', #48532, #42100 ) ;
#41155 = ORIENTED_EDGE ( 'NONE', *, *, #24832, .F. ) ;
#41156 = ORIENTED_EDGE ( 'NONE', *, *, #31692, .T. ) ;
#41157 = CARTESIAN_POINT ( 'NONE',  ( -11.14611441067771658, -11.60115924236117024, 67.91304812855648265 ) ) ;
#41158 = CARTESIAN_POINT ( 'NONE',  ( -20.19053640067075506, -7.838066347919499854, 54.27966884056654351 ) ) ;
#41159 = EDGE_LOOP ( 'NONE', ( #47887, #4176, #28791, #46469, #33945 ) ) ;
#41161 = CARTESIAN_POINT ( 'NONE',  ( -24.09792889798371007, -17.08130376423426000, 73.18336032035891492 ) ) ;
#41160 = CARTESIAN_POINT ( 'NONE',  ( -15.33667684601822856, -7.657446057057493150, 74.21839124043556524 ) ) ;
#41162 = CARTESIAN_POINT ( 'NONE',  ( -13.43921408130402995, -8.993432070331126127, 60.73950277491898930 ) ) ;
#41163 = CARTESIAN_POINT ( 'NONE',  ( -11.61693612796584141, -18.71788356627799388, 64.76209452048259152 ) ) ;
#41164 = CARTESIAN_POINT ( 'NONE',  ( -24.74352993119518374, -16.19876237476239922, 62.75361995816021476 ) ) ;
#41165 = FACE_BOUND ( 'NONE', #12609, .T. ) ;
#41166 = CARTESIAN_POINT ( 'NONE',  ( -19.59076105604923868, -21.93735943072320538, 62.15536986693265931 ) ) ;
#41167 = CARTESIAN_POINT ( 'NONE',  ( -13.62948724496060215, -8.926948417807865965, 57.26967755883410405 ) ) ;
#41168 = CARTESIAN_POINT ( 'NONE',  ( -16.65537282897929927, -21.76815620359785797, 68.76730947549657458 ) ) ;
#41169 = LINE ( 'NONE', #5813, #30477 ) ;
#41170 = EDGE_CURVE ( 'NONE', #29820, #20335, #9127, .T. ) ;
#41171 = ORIENTED_EDGE ( 'NONE', *, *, #9221, .T. ) ;
#41172 = CARTESIAN_POINT ( 'NONE',  ( -24.12071557656922494, -11.54438865435207795, 63.06722852297808402 ) ) ;
#41173 = CARTESIAN_POINT ( 'NONE',  ( -9.990623027812100432, -14.31192454061599229, 64.57299275950818185 ) ) ;
#41174 = CARTESIAN_POINT ( 'NONE',  ( -12.10000935918735010, -20.02047918228639034, 61.50340342271149296 ) ) ;
#41175 =( BOUNDED_CURVE ( )  B_SPLINE_CURVE ( 2, ( #29361, #44633, #44393 ),
 .UNSPECIFIED., .F., .F. ) 
 B_SPLINE_CURVE_WITH_KNOTS ( ( 3, 3 ),
 ( 0.9166666666666666297, 0.9259045776023205887 ),
 .UNSPECIFIED. ) 
 CURVE ( )  GEOMETRIC_REPRESENTATION_ITEM ( )  RATIONAL_B_SPLINE_CURVE ( ( 1.000000000000000000, 0.9324933664920571630, 0.9847218244232577300 ) ) 
 REPRESENTATION_ITEM ( '' )  );
#41176 = CARTESIAN_POINT ( 'NONE',  ( -45.92409385541306222, -14.20920654474410760, 70.50000000000000000 ) ) ;
#41177 = CARTESIAN_POINT ( 'NONE',  ( -21.17409385541299116, -6.859212275519752211, 50.50378509014304029 ) ) ;
#41178 = CARTESIAN_POINT ( 'NONE',  ( -11.81178692268928643, -10.62566621335946770, 74.43885052268630886 ) ) ;
#41179 = DIRECTION ( 'NONE',  ( 1.000000000000000000, 2.866981220435666553E-17, 0.000000000000000000 ) ) ;
#41180 = EDGE_LOOP ( 'NONE', ( #29194, #39994, #4208, #2487 ) ) ;
#41181 = ORIENTED_EDGE ( 'NONE', *, *, #39002, .F. ) ;
#41182 = CARTESIAN_POINT ( 'NONE',  ( -14.81784385541304339, -6.860780111191487229, 51.02154966934377711 ) ) ;
#41183 = EDGE_CURVE ( 'NONE', #47012, #25059, #33730, .T. ) ;
#41184 = ORIENTED_EDGE ( 'NONE', *, *, #42541, .F. ) ;
#41185 = DIRECTION ( 'NONE',  ( -6.258914682829359833E-07, 5.777405174637831559E-07, 0.9999999999996371791 ) ) ;
#41186 = AXIS2_PLACEMENT_3D ( 'NONE', #8384, #19713, #7422 ) ;
#41187 = EDGE_CURVE ( 'NONE', #42844, #28760, #24869, .T. ) ;
#41188 = CARTESIAN_POINT ( 'NONE',  ( -18.97054410961560578, -7.521390078327941708, 67.08567059339527816 ) ) ;
#41189 = EDGE_CURVE ( 'NONE', #5480, #9880, #3221, .T. ) ;
#41190 = LINE ( 'NONE', #8924, #25699 ) ;
#41191 = CARTESIAN_POINT ( 'NONE',  ( -10.37541943412130863, -14.96049300415475436, 75.08306784598362071 ) ) ;
#41192 = ORIENTED_EDGE ( 'NONE', *, *, #3544, .T. ) ;
#41193 = FACE_OUTER_BOUND ( 'NONE', #28555, .T. ) ;
#41194 = ORIENTED_EDGE ( 'NONE', *, *, #28294, .T. ) ;
#41195 = PLANE ( 'NONE',  #13141 ) ;
#41196 = CARTESIAN_POINT ( 'NONE',  ( -13.86230672564574284, -20.89334503125211029, 68.45625163552200831 ) ) ;
#41197 = VERTEX_POINT ( 'NONE', #29487 ) ;
#41198 = CARTESIAN_POINT ( 'NONE',  ( -23.92719435707370224, -11.17417392741853988, 70.00715344888816105 ) ) ;
#41199 = CARTESIAN_POINT ( 'NONE',  ( -11.10300331676175567, -11.79817459733614093, 74.74767048167663575 ) ) ;
#41200 = CARTESIAN_POINT ( 'NONE',  ( -22.80623672001925328, -19.96042370788389064, 72.79400547454775960 ) ) ;
#41201 = EDGE_LOOP ( 'NONE', ( #3367, #20092 ) ) ;
#41202 = DIRECTION ( 'NONE',  ( 0.9687793358424822143, -0.2479245821708672415, 0.000000000000000000 ) ) ;
#41203 = PLANE ( 'NONE',  #34413 ) ;
#41204 = CARTESIAN_POINT ( 'NONE',  ( -24.30112618867181240, -13.25578303422174997, 59.64795780745660636 ) ) ;
#41205 = DIRECTION ( 'NONE',  ( 0.6973657521612035559, -0.7167154300785206766, 1.015100524683467946E-08 ) ) ;
#41206 = EDGE_LOOP ( 'NONE', ( #13760, #22445, #35688, #11488, #41329 ) ) ;
#41207 = LINE ( 'NONE', #4041, #3632 ) ;
#41208 = DIRECTION ( 'NONE',  ( 0.9687793358424821033, -0.2479245821708677133, 0.000000000000000000 ) ) ;
#41209 = CARTESIAN_POINT ( 'NONE',  ( -10.77303329795002895, -12.62668660113453178, 60.79853568451941470 ) ) ;
#41210 = CARTESIAN_POINT ( 'NONE',  ( -17.95971906749393554, -21.78880692639934225, 61.87535914958314009 ) ) ;
#41211 = VECTOR ( 'NONE', #37022, 1000.000000000000114 ) ;
#41212 = CARTESIAN_POINT ( 'NONE',  ( -18.64284385650552167, -8.811426318492348031, 52.18089403414751359 ) ) ;
#41213 = ORIENTED_EDGE ( 'NONE', *, *, #3886, .F. ) ;
#41214 = CARTESIAN_POINT ( 'NONE',  ( -17.77159098340391097, -22.25115097675990583, 58.59827546209168503 ) ) ;
#41215 = CARTESIAN_POINT ( 'NONE',  ( -24.27133562072960871, -13.11802050994479707, 59.24779033130878503 ) ) ;
#41216 = ORIENTED_EDGE ( 'NONE', *, *, #44587, .T. ) ;
#41217 = CARTESIAN_POINT ( 'NONE',  ( -11.29821430689275630, -19.04912289309577744, 68.32415498359496553 ) ) ;
#41218 = CARTESIAN_POINT ( 'NONE',  ( -15.37833354036149380, -8.114753493370539417, 74.15273655567226285 ) ) ;
#41219 = PLANE ( 'NONE',  #18726 ) ;
#41220 =( BOUNDED_SURFACE ( )  B_SPLINE_SURFACE ( 3, 1, ( 
 ( #22577, #29476 ),
 ( #37090, #26767 ),
 ( #26515, #18883 ),
 ( #3876, #3616 ),
 ( #40796, #34369 ),
 ( #45250, #30226 ),
 ( #8070, #7334 ) ),
 .UNSPECIFIED., .T., .F., .F. ) 
 B_SPLINE_SURFACE_WITH_KNOTS ( ( 4, 3, 4 ),
 ( 2, 2 ),
 ( 0.000000000000000000, 0.5000000000000000000, 1.000000000000000000 ),
 ( 0.000000000000000000, 1.000000000000000000 ),
 .UNSPECIFIED. ) 
 GEOMETRIC_REPRESENTATION_ITEM ( )  RATIONAL_B_SPLINE_SURFACE ( (
 ( 1.000000000000000000, 1.000000000000000000),
 ( 0.3333333333333335369, 0.3333333333333330373),
 ( 0.3333333333333335369, 0.3333333333333330373),
 ( 1.000000000000000000, 1.000000000000000000),
 ( 0.3333333333333333703, 0.3333333333333333703),
 ( 0.3333333333333333703, 0.3333333333333333703),
 ( 1.000000000000000000, 1.000000000000000000) ) ) 
 REPRESENTATION_ITEM ( '' )  SURFACE ( )  );
#41221 = ADVANCED_FACE ( 'NONE', ( #10302 ), #14195, .T. ) ;
#41222 = ORIENTED_EDGE ( 'NONE', *, *, #30174, .T. ) ;
#41223 = CARTESIAN_POINT ( 'NONE',  ( -17.06879511326789256, -7.767867012253359071, 73.97490359703523666 ) ) ;
#41224 = CARTESIAN_POINT ( 'NONE',  ( -10.07990710174555460, -16.41795825442990520, 53.76227901944321985 ) ) ;
#41225 = ORIENTED_EDGE ( 'NONE', *, *, #155, .T. ) ;
#41226 = CARTESIAN_POINT ( 'NONE',  ( -13.13034385650551883, -9.794322478646142471, 51.19202720610083901 ) ) ;
#41227 = DIRECTION ( 'NONE',  ( 1.000000000000000000, 2.866981220435666553E-17, 0.000000000000000000 ) ) ;
#41228 = CARTESIAN_POINT ( 'NONE',  ( -24.79685378108793259, -15.88006503112767476, 69.71120271104469168 ) ) ;
#41229 = CARTESIAN_POINT ( 'NONE',  ( -13.33738394060092070, -12.51528319768659436, 49.52966884056655772 ) ) ;
#41230 = CARTESIAN_POINT ( 'NONE',  ( -10.84199182719153320, -17.34482810118634433, 61.36563051411450687 ) ) ;
#41231 =( BOUNDED_CURVE ( )  B_SPLINE_CURVE ( 3, ( #38587, #27268, #42545, #15430 ),
 .UNSPECIFIED., .F., .F. ) 
 B_SPLINE_CURVE_WITH_KNOTS ( ( 4, 4 ),
 ( 0.4074455897393674531, 0.5000000000000000000 ),
 .UNSPECIFIED. ) 
 CURVE ( )  GEOMETRIC_REPRESENTATION_ITEM ( )  RATIONAL_B_SPLINE_CURVE ( ( 0.6983129098261020573, 0.7760317562606975361, 0.8765941196519944079, 0.9999999999999865663 ) ) 
 REPRESENTATION_ITEM ( '' )  );
#41232 = EDGE_LOOP ( 'NONE', ( #25000, #35426, #31014, #5841 ) ) ;
#41233 = ORIENTED_EDGE ( 'NONE', *, *, #44073, .F. ) ;
#41234 = CARTESIAN_POINT ( 'NONE',  ( -14.23034385650551492, -9.794322478646142471, 51.19202720610083901 ) ) ;
#41235 = ADVANCED_FACE ( 'NONE', ( #36138 ), #47962, .T. ) ;
#41236 = CARTESIAN_POINT ( 'NONE',  ( -10.45452701611611168, -14.15586467111139690, 61.21821260753697658 ) ) ;
#41237 = CARTESIAN_POINT ( 'NONE',  ( -11.35719102664687874, -18.40077844947705188, 58.09242476654641507 ) ) ;
#41238 = ADVANCED_FACE ( 'NONE', ( #43797 ), #40808, .F. ) ;
#41239 = CARTESIAN_POINT ( 'NONE',  ( -15.91784385650552025, -9.790100578890868377, 49.79778022625163203 ) ) ;
#41240 =( BOUNDED_SURFACE ( )  B_SPLINE_SURFACE ( 3, 1, ( 
 ( #23828, #42543 ),
 ( #5107, #12956 ),
 ( #31443, #46479 ),
 ( #20120, #22926 ),
 ( #12732, #45323 ),
 ( #28239, #30313 ),
 ( #11575, #16887 ) ),
 .UNSPECIFIED., .T., .F., .F. ) 
 B_SPLINE_SURFACE_WITH_KNOTS ( ( 4, 3, 4 ),
 ( 2, 2 ),
 ( 0.000000000000000000, 0.5000000000000000000, 1.000000000000000000 ),
 ( 0.000000000000000000, 1.000000000000000000 ),
 .UNSPECIFIED. ) 
 GEOMETRIC_REPRESENTATION_ITEM ( )  RATIONAL_B_SPLINE_SURFACE ( (
 ( 1.000000000000000000, 1.000000000000000000),
 ( 0.3333333333333335369, 0.3333333333333330373),
 ( 0.3333333333333335369, 0.3333333333333330373),
 ( 1.000000000000000000, 1.000000000000000000),
 ( 0.3333333333333333703, 0.3333333333333333703),
 ( 0.3333333333333333703, 0.3333333333333333703),
 ( 1.000000000000000000, 1.000000000000000000) ) ) 
 REPRESENTATION_ITEM ( '' )  SURFACE ( )  );
#41241 = VECTOR ( 'NONE', #11261, 1000.000000000000000 ) ;
#41242 = ORIENTED_EDGE ( 'NONE', *, *, #48261, .T. ) ;
#41243 = EDGE_CURVE ( 'NONE', #33165, #36602, #5434, .T. ) ;
#41244 = CARTESIAN_POINT ( 'NONE',  ( -15.39388989008627995, -21.97733388496078177, 72.23070757706680922 ) ) ;
#41245 = CARTESIAN_POINT ( 'NONE',  ( -46.29409385541305255, -14.20920654474410760, 69.94787228701220272 ) ) ;
#41246 = CARTESIAN_POINT ( 'NONE',  ( -24.77723877343947478, -16.00713684962007122, 66.24820200538215431 ) ) ;
#41247 = EDGE_CURVE ( 'NONE', #11764, #31313, #7007, .T. ) ;
#41248 = ORIENTED_EDGE ( 'NONE', *, *, #5616, .F. ) ;
#41249 = CARTESIAN_POINT ( 'NONE',  ( -15.87557675045462169, -7.931373007531637320, 67.29007279016111909 ) ) ;
#41250 = ORIENTED_EDGE ( 'NONE', *, *, #44993, .F. ) ;
#41251 = CARTESIAN_POINT ( 'NONE',  ( -24.85757945293173776, -20.98010847878158813, 54.49999999999995026 ) ) ;
#41252 = LINE ( 'NONE', #625, #28406 ) ;
#41253 = CARTESIAN_POINT ( 'NONE',  ( -11.32469144785208925, -18.34471071427194389, 57.80714594245691984 ) ) ;
#41254 = ORIENTED_EDGE ( 'NONE', *, *, #44401, .F. ) ;
#41255 = CARTESIAN_POINT ( 'NONE',  ( -20.00946575929301474, -8.250368826910309039, 74.02096600124984604 ) ) ;
#41256 = CARTESIAN_POINT ( 'NONE',  ( -15.31160308370628442, -21.95360096069865108, 72.20721981275677592 ) ) ;
#41257 = CARTESIAN_POINT ( 'NONE',  ( -17.26958401828953171, -19.65204229739824626, 49.52966884056656482 ) ) ;
#41258 = CARTESIAN_POINT ( 'NONE',  ( -17.42409385541305511, -14.80920654474410725, 52.21286476528345588 ) ) ;
#41259 = ORIENTED_EDGE ( 'NONE', *, *, #27664, .F. ) ;
#41260 = B_SPLINE_CURVE_WITH_KNOTS ( 'NONE', 3,
 ( #19505, #30857, #19025, #38203, #45868, #41680, #34031, #4255, #7965, #19766 ),
 .UNSPECIFIED., .F., .F.,
 ( 4, 2, 2, 2, 4 ),
 ( 0.000000000000000000, 0.2500000000000000000, 0.5000000000000000000, 0.7500000000000000000, 1.000000000000000000 ),
 .UNSPECIFIED. ) ;
#41261 = CARTESIAN_POINT ( 'NONE',  ( -12.77796340496265870, -17.75258416873320400, 53.49999999999995026 ) ) ;
#41262 = CARTESIAN_POINT ( 'NONE',  ( -10.74038475888173672, -11.51784756383862351, 71.22827500095982600 ) ) ;
#41263 = FACE_BOUND ( 'NONE', #31319, .T. ) ;
#41264 = B_SPLINE_CURVE_WITH_KNOTS ( 'NONE', 3,
 ( #28840, #10136, #25155, #21696, #6449, #2730, #17738, #45822, #15991, #4211 ),
 .UNSPECIFIED., .F., .F.,
 ( 4, 2, 2, 2, 4 ),
 ( 0.000000000000000000, 0.2500000000000000000, 0.5000000000000000000, 0.7500000000000000000, 1.000000000000000000 ),
 .UNSPECIFIED. ) ;
#41265 = ORIENTED_EDGE ( 'NONE', *, *, #7171, .T. ) ;
#41266 = DIRECTION ( 'NONE',  ( 1.000000000000000000, -4.164305804376849788E-17, 1.614929280266638808E-16 ) ) ;
#41267 = CARTESIAN_POINT ( 'NONE',  ( -14.97188219925329378, -8.199429090594037461, 57.14999999999994174 ) ) ;
#41268 = CARTESIAN_POINT ( 'NONE',  ( -17.42409385541299471, -14.80920654474435771, 49.52966884056655772 ) ) ;
#41269 = CARTESIAN_POINT ( 'NONE',  ( -23.93648101794248362, -17.51022725521227841, 65.95829288617392194 ) ) ;
#41270 = EDGE_LOOP ( 'NONE', ( #15789, #33606, #47841, #5856, #34895 ) ) ;
#41271 = CARTESIAN_POINT ( 'NONE',  ( -10.47603521207407518, -16.02136065384195973, 71.86239274348770323 ) ) ;
#41272 = ORIENTED_EDGE ( 'NONE', *, *, #38732, .T. ) ;
#41273 = CARTESIAN_POINT ( 'NONE',  ( -12.72371041375474299, -9.029147237807901405, 70.94951108828513497 ) ) ;
#41274 = CARTESIAN_POINT ( 'NONE',  ( -16.97112922959608383, -7.770054067326150005, 70.49035865952242830 ) ) ;
#41275 = EDGE_CURVE ( 'NONE', #36030, #26171, #38784, .T. ) ;
#41276 = DIRECTION ( 'NONE',  ( 1.000000000000000000, -0.000000000000000000, -0.000000000000000000 ) ) ;
#41277 = EDGE_LOOP ( 'NONE', ( #15550, #29718, #16890, #7917, #16816 ) ) ;
#41278 = CARTESIAN_POINT ( 'NONE',  ( -16.17771238455266314, -22.15437642958356435, 58.42439015775072875 ) ) ;
#41279 = VECTOR ( 'NONE', #41227, 1000.000000000000000 ) ;
#41280 = CARTESIAN_POINT ( 'NONE',  ( -18.37541875070384734, -22.19822623024843011, 69.01503475768117823 ) ) ;
#41281 = ORIENTED_EDGE ( 'NONE', *, *, #17651, .T. ) ;
#41282 = AXIS2_PLACEMENT_3D ( 'NONE', #45946, #45722, #15387 ) ;
#41283 = EDGE_LOOP ( 'NONE', ( #237, #43437, #1856, #34674 ) ) ;
#41284 = VERTEX_POINT ( 'NONE', #45917 ) ;
#41285 = CARTESIAN_POINT ( 'NONE',  ( -24.72409385541305582, -14.80920654474410902, 57.89999999999999147 ) ) ;
#41286 = DIRECTION ( 'NONE',  ( 0.000000000000000000, 1.000000000000000000, -0.000000000000000000 ) ) ;
#41287 = CARTESIAN_POINT ( 'NONE',  ( -21.26726687448728015, -20.65992264386038713, 69.28123431651795272 ) ) ;
#41288 = CARTESIAN_POINT ( 'NONE',  ( -16.64495962069230117, -22.21910613783234822, 65.33909019606271329 ) ) ;
#41289 = CARTESIAN_POINT ( 'NONE',  ( -24.23813412381375088, -12.99935709875259526, 66.31718868320673721 ) ) ;
#41290 = FACE_OUTER_BOUND ( 'NONE', #38325, .T. ) ;
#41291 = EDGE_CURVE ( 'NONE', #11910, #1437, #42467, .T. ) ;
#41292 = CARTESIAN_POINT ( 'NONE',  ( -19.41839133894716340, -8.097970443116885519, 60.03263303940221363 ) ) ;
#41293 = ORIENTED_EDGE ( 'NONE', *, *, #12542, .F. ) ;
#41294 = EDGE_LOOP ( 'NONE', ( #4936, #8563, #35437, #19350, #26824 ) ) ;
#41295 = CARTESIAN_POINT ( 'NONE',  ( -16.22958052549516950, -7.455513305798441515, 60.45674424308347739 ) ) ;
#41296 = CARTESIAN_POINT ( 'NONE',  ( -9.990623107247818879, -14.31192343302863179, 64.57299167182827659 ) ) ;
#41297 = CARTESIAN_POINT ( 'NONE',  ( -10.40860991809309155, -15.50898095412354571, 57.85320721669017985 ) ) ;
#41298 = LINE ( 'NONE', #14931, #14984 ) ;
#41299 = ORIENTED_EDGE ( 'NONE', *, *, #35759, .F. ) ;
#41300 = CARTESIAN_POINT ( 'NONE',  ( -14.03034385650551563, -9.794322478646142471, 51.19202720610083901 ) ) ;
#41301 = ORIENTED_EDGE ( 'NONE', *, *, #6116, .F. ) ;
#41302 = EDGE_CURVE ( 'NONE', #26240, #44533, #33110, .T. ) ;
#41303 = CARTESIAN_POINT ( 'NONE',  ( -16.05912136036848636, -21.67647323057698827, 58.39658775893972376 ) ) ;
#41304 = DIRECTION ( 'NONE',  ( -3.413470714839332458E-33, 1.190614954331866791E-16, -1.000000000000000000 ) ) ;
#41305 = EDGE_CURVE ( 'NONE', #41870, #37220, #20232, .T. ) ;
#41306 = DIRECTION ( 'NONE',  ( -3.071710424422018668E-17, 6.404604876783312462E-16, 1.000000000000000000 ) ) ;
#41307 = EDGE_CURVE ( 'NONE', #3548, #2848, #1320, .T. ) ;
#41308 = ORIENTED_EDGE ( 'NONE', *, *, #37047, .T. ) ;
#41309 = FACE_OUTER_BOUND ( 'NONE', #48678, .T. ) ;
#41310 = AXIS2_PLACEMENT_3D ( 'NONE', #17105, #9982, #36310 ) ;
#41311 = DIRECTION ( 'NONE',  ( -0.5263399769092093061, 0.8502742079512978224, 7.678741024442198749E-08 ) ) ;
#41312 = DIRECTION ( 'NONE',  ( -3.071710424422018668E-17, 6.404604876783312462E-16, 1.000000000000000000 ) ) ;
#41313 = VERTEX_POINT ( 'NONE', #46401 ) ;
#41314 = EDGE_CURVE ( 'NONE', #42407, #29156, #35844, .T. ) ;
#41315 = DIRECTION ( 'NONE',  ( 0.9687793358424821033, -0.2479245821708680464, 0.000000000000000000 ) ) ;
#41316 = CARTESIAN_POINT ( 'NONE',  ( -22.09139187696106887, -9.002414929697756918, 63.34153754183413554 ) ) ;
#41317 = ORIENTED_EDGE ( 'NONE', *, *, #12761, .F. ) ;
#41318 = CARTESIAN_POINT ( 'NONE',  ( -10.50465667362414912, -15.86897300143100331, 64.50771547874023781 ) ) ;
#41319 = EDGE_CURVE ( 'NONE', #1220, #31794, #32013, .T. ) ;
#41320 = VERTEX_POINT ( 'NONE', #16089 ) ;
#41321 = DIRECTION ( 'NONE',  ( -3.071710424422018668E-17, 6.404604876783312462E-16, 1.000000000000000000 ) ) ;
#41322 = DIRECTION ( 'NONE',  ( 4.664556981411351282E-06, -8.285185778185610086E-06, 0.9999999999547987128 ) ) ;
#41323 = ORIENTED_EDGE ( 'NONE', *, *, #19487, .T. ) ;
#41324 = EDGE_CURVE ( 'NONE', #18740, #23020, #17252, .T. ) ;
#41325 = EDGE_CURVE ( 'NONE', #14412, #27215, #33830, .T. ) ;
#41326 = CARTESIAN_POINT ( 'NONE',  ( -21.35358943365839579, -4.907296734360127033, 54.60745305979834541 ) ) ;
#41327 = CARTESIAN_POINT ( 'NONE',  ( -24.47217469005601131, -14.64471752244405067, 62.71296487297676947 ) ) ;
#41328 = LINE ( 'NONE', #44797, #23396 ) ;
#41329 = ORIENTED_EDGE ( 'NONE', *, *, #9712, .F. ) ;
#41330 = LINE ( 'NONE', #37621, #24491 ) ;
#41331 = CARTESIAN_POINT ( 'NONE',  ( -22.31145688432076568, -19.82056192467315370, 65.81307812901205523 ) ) ;
#41332 = DIRECTION ( 'NONE',  ( -0.3688590060343657773, 0.9294853595766529031, 0.000000000000000000 ) ) ;
#41333 = EDGE_LOOP ( 'NONE', ( #38938, #37128 ) ) ;
#41334 = CARTESIAN_POINT ( 'NONE',  ( -19.61601503992405071, -21.50980213996393786, 65.76486213821364402 ) ) ;
#41335 = CARTESIAN_POINT ( 'NONE',  ( -17.42409385541299471, -14.80920654474435771, 49.52966884056655772 ) ) ;
#41336 = LINE ( 'NONE', #7628, #27924 ) ;
#41337 = ORIENTED_EDGE ( 'NONE', *, *, #22932, .T. ) ;
#41338 = VERTEX_POINT ( 'NONE', #23997 ) ;
#41339 = CARTESIAN_POINT ( 'NONE',  ( -22.89702288877819214, -9.753446293288515534, 73.66816357947271854 ) ) ;
#41340 = DIRECTION ( 'NONE',  ( 0.3047757271037810356, -0.002884009000655191491, 0.9524197806957002133 ) ) ;
#41341 = CARTESIAN_POINT ( 'NONE',  ( -10.39386236808646480, -14.28108337702217945, 64.38803875189576331 ) ) ;
#41342 = CARTESIAN_POINT ( 'NONE',  ( -13.78034385759799108, -9.360768649639302552, 51.01397948905922419 ) ) ;
#41343 = CARTESIAN_POINT ( 'NONE',  ( -20.00308622248979162, -8.244632374337111713, 70.13611736960565679 ) ) ;
#41344 = CARTESIAN_POINT ( 'NONE',  ( -11.12358220677134035, -11.75903396576748605, 71.08860871065073184 ) ) ;
#41345 = CARTESIAN_POINT ( 'NONE',  ( -20.51476236319894753, -8.030485483676169878, 66.97378244640404432 ) ) ;
#41346 = CARTESIAN_POINT ( 'NONE',  ( -17.42409385541299471, -14.80920654474434883, 62.02966884056656482 ) ) ;
#41347 = AXIS2_PLACEMENT_3D ( 'NONE', #13291, #28585, #39171 ) ;
#41348 = ORIENTED_EDGE ( 'NONE', *, *, #41738, .F. ) ;
#41349 = CARTESIAN_POINT ( 'NONE',  ( -11.53247046633659245, -18.68106308600668441, 64.74707076449911369 ) ) ;
#41350 = EDGE_CURVE ( 'NONE', #43006, #37616, #7350, .T. ) ;
#41351 = CARTESIAN_POINT ( 'NONE',  ( -16.17583575424048092, -10.27959207348368764, 49.52966884056655772 ) ) ;
#41352 = CYLINDRICAL_SURFACE ( 'NONE', #11963, 1.999999999999999556 ) ;
#41353 = ORIENTED_EDGE ( 'NONE', *, *, #28625, .F. ) ;
#41354 = ORIENTED_EDGE ( 'NONE', *, *, #28769, .T. ) ;
#41355 = ADVANCED_FACE ( 'NONE', ( #41732 ), #39000, .T. ) ;
#41356 = CARTESIAN_POINT ( 'NONE',  ( -17.42409385541299471, -14.80920654474435594, 52.02966884056656482 ) ) ;
#41357 = CARTESIAN_POINT ( 'NONE',  ( -7.424093855413048892, -27.10920654474410796, 63.99999999999998579 ) ) ;
#41358 = CARTESIAN_POINT ( 'NONE',  ( -22.00903739223959477, -8.936221312270376416, 63.30498424023031845 ) ) ;
#41359 = CARTESIAN_POINT ( 'NONE',  ( -14.98659385541304445, -7.222650657624106962, 49.61879703869476543 ) ) ;
#41360 =( BOUNDED_CURVE ( )  B_SPLINE_CURVE ( 3, ( #22010, #29154, #33544, #45167 ),
 .UNSPECIFIED., .F., .F. ) 
 B_SPLINE_CURVE_WITH_KNOTS ( ( 4, 4 ),
 ( 0.4074455897393693959, 0.5000000000000000000 ),
 .UNSPECIFIED. ) 
 CURVE ( )  GEOMETRIC_REPRESENTATION_ITEM ( )  RATIONAL_B_SPLINE_CURVE ( ( 0.6983129098261122714, 0.7760317562607196296, 0.8765941196520169454, 1.000000000000007550 ) ) 
 REPRESENTATION_ITEM ( '' )  );
#41361 = ORIENTED_EDGE ( 'NONE', *, *, #46117, .T. ) ;
#41362 = CARTESIAN_POINT ( 'NONE',  ( -15.09544296547830022, -21.46351980780830715, 65.25596681500472585 ) ) ;
#41363 = CARTESIAN_POINT ( 'NONE',  ( -24.16575343130564590, -12.74704122656904914, 69.92243002240397232 ) ) ;
#41364 = EDGE_LOOP ( 'NONE', ( #41337, #13616, #1281, #11286 ) ) ;
#41365 = CARTESIAN_POINT ( 'NONE',  ( -22.04378365035703879, -20.13510231884741231, 62.24911246861644543 ) ) ;
#41366 = PLANE ( 'NONE',  #24971 ) ;
#41367 = ORIENTED_EDGE ( 'NONE', *, *, #27051, .T. ) ;
#41368 = CARTESIAN_POINT ( 'NONE',  ( -19.96689475682054038, -8.233588121658772963, 74.01536847284175735 ) ) ;
#41369 =( BOUNDED_CURVE ( )  B_SPLINE_CURVE ( 3, ( #28312, #42845, #38896, #9113 ),
 .UNSPECIFIED., .F., .F. ) 
 B_SPLINE_CURVE_WITH_KNOTS ( ( 4, 4 ),
 ( 0.5000000000000000000, 0.9074455897393642889 ),
 .UNSPECIFIED. ) 
 CURVE ( )  GEOMETRIC_REPRESENTATION_ITEM ( )  RATIONAL_B_SPLINE_CURVE ( ( 1.000000000000013323, 0.4567392136813366310, 0.3561768502900224953, 0.6983129098260856260 ) ) 
 REPRESENTATION_ITEM ( '' )  );
#41370 = EDGE_CURVE ( 'NONE', #15782, #18613, #23267, .T. ) ;
#41371 = AXIS2_PLACEMENT_3D ( 'NONE', #39121, #39372, #982 ) ;
#41372 = VERTEX_POINT ( 'NONE', #5278 ) ;
#41373 = DIRECTION ( 'NONE',  ( 0.7364384864160969935, -0.6765045127160409510, -1.031360483216681931E-08 ) ) ;
#41374 = CARTESIAN_POINT ( 'NONE',  ( -20.52762743779272014, -8.534807845156915818, 63.31121513079826713 ) ) ;
#41375 = ORIENTED_EDGE ( 'NONE', *, *, #35383, .F. ) ;
#41376 = CARTESIAN_POINT ( 'NONE',  ( 23.52590614458706852, 1.876518846661452411, 52.53023010607846288 ) ) ;
#41377 = EDGE_CURVE ( 'NONE', #47695, #48717, #23511, .T. ) ;
#41378 = EDGE_CURVE ( 'NONE', #25345, #31288, #17059, .T. ) ;
#41379 = CARTESIAN_POINT ( 'NONE',  ( -21.13535303541993926, -18.52256826949110646, 49.52966884056656482 ) ) ;
#41380 = CARTESIAN_POINT ( 'NONE',  ( -19.63034385650552238, -9.794322478646142471, 51.19202720610083190 ) ) ;
#41381 = DIRECTION ( 'NONE',  ( 2.662580029140978055E-06, -1.091441817711415488E-05, 0.9999999999368930359 ) ) ;
#41382 = CARTESIAN_POINT ( 'NONE',  ( -10.79572390357762046, -11.40795830647630282, 67.80360014157953685 ) ) ;
#41383 = CARTESIAN_POINT ( 'NONE',  ( -10.54224321960240651, -17.66275930416250262, 68.29710731422549941 ) ) ;
#41384 = CARTESIAN_POINT ( 'NONE',  ( -13.36191307535780659, -8.564050219684345322, 57.16241883859221673 ) ) ;
#41385 = ORIENTED_EDGE ( 'NONE', *, *, #36823, .T. ) ;
#41386 = B_SPLINE_CURVE_WITH_KNOTS ( 'NONE', 1,
 ( #41555, #30730 ),
 .UNSPECIFIED., .F., .F.,
 ( 2, 2 ),
 ( 0.000000000000000000, 1.000000000000000000 ),
 .UNSPECIFIED. ) ;
#41387 = CARTESIAN_POINT ( 'NONE',  ( -15.23931321672068329, -21.51228997375478968, 68.58152699338896241 ) ) ;
#41388 = CARTESIAN_POINT ( 'NONE',  ( -10.37743716876973643, -14.51010320183636715, 64.27315137562472103 ) ) ;
#41389 = CARTESIAN_POINT ( 'NONE',  ( -24.27033198218900978, -13.12649362337911718, 62.83264177274070050 ) ) ;
#41390 = EDGE_CURVE ( 'NONE', #6207, #45223, #40085, .T. ) ;
#41391 = DIRECTION ( 'NONE',  ( -2.866981220435666553E-17, 1.000000000000000000, 1.190614954331866791E-16 ) ) ;
#41392 = LINE ( 'NONE', #11121, #8601 ) ;
#41393 = DIRECTION ( 'NONE',  ( 4.267285103686815209E-17, -5.292884291094200710E-16, -1.000000000000000000 ) ) ;
#41394 = VERTEX_POINT ( 'NONE', #35778 ) ;
#41395 = EDGE_LOOP ( 'NONE', ( #33923, #30359, #15743, #1316, #28795 ) ) ;
#41396 = CARTESIAN_POINT ( 'NONE',  ( -16.84904595140906025, -21.78683020288652372, 72.23713474854929473 ) ) ;
#41397 = CARTESIAN_POINT ( 'NONE',  ( -45.92409385541306222, -14.90920654474410867, 69.15000000000000568 ) ) ;
#41398 = EDGE_LOOP ( 'NONE', ( #30815, #9277 ) ) ;
#41399 = CARTESIAN_POINT ( 'NONE',  ( -13.10965166868813903, -12.97921450448603231, 52.02966884056656482 ) ) ;
#41400 = CARTESIAN_POINT ( 'NONE',  ( -23.96075645138428456, -17.45014240273063066, 65.94357239682317129 ) ) ;
#41401 = CARTESIAN_POINT ( 'NONE',  ( -11.91470689456726717, -9.793200236000155101, 64.21569601040394559 ) ) ;
#41402 = DIRECTION ( 'NONE',  ( 0.3224496555704357559, 0.8691421305882567339, 0.3749909018349820711 ) ) ;
#41403 = CARTESIAN_POINT ( 'NONE',  ( -21.59090693955708318, -20.98503893958440258, 72.63108097743202052 ) ) ;
#41404 = CARTESIAN_POINT ( 'NONE',  ( -10.82793724842355765, -11.34591556451386651, 67.87510537416113721 ) ) ;
#41405 = DIRECTION ( 'NONE',  ( -1.000000000000000000, 0.000000000000000000, -0.000000000000000000 ) ) ;
#41406 = CARTESIAN_POINT ( 'NONE',  ( -10.90759836534377492, -17.49952001658422063, 68.39721944423101263 ) ) ;
#41407 = CARTESIAN_POINT ( 'NONE',  ( 18.57590614458706924, 2.144455078683968452, 49.30629848276639393 ) ) ;
#41408 = ADVANCED_FACE ( 'NONE', ( #6494 ), #6249, .T. ) ;
#41409 = DIRECTION ( 'NONE',  ( -4.436160455182634911E-06, -7.761523761658527715E-06, 0.9999999999600395206 ) ) ;
#41410 = CARTESIAN_POINT ( 'NONE',  ( -14.98927377128279304, -8.246306944878790901, 47.99999999999994316 ) ) ;
#41411 = CARTESIAN_POINT ( 'NONE',  ( -15.54561509764458371, -8.065849839147006151, 74.37985694181431029 ) ) ;
#41412 = DIRECTION ( 'NONE',  ( -3.413470714839332458E-33, 1.190614954331866791E-16, -1.000000000000000000 ) ) ;
#41413 = DIRECTION ( 'NONE',  ( -0.000000000000000000, -1.000000000000000000, 0.000000000000000000 ) ) ;
#41414 = DIRECTION ( 'NONE',  ( 0.7489133456531319455, 0.6626679415081376812, -6.686399186099785819E-09 ) ) ;
#41415 = CARTESIAN_POINT ( 'NONE',  ( -17.78516316699992217, -21.85793681952389989, 65.48965078530844153 ) ) ;
#41416 = EDGE_LOOP ( 'NONE', ( #46599, #44596, #2232, #27915 ) ) ;
#41417 = AXIS2_PLACEMENT_3D ( 'NONE', #41869, #30310, #14740 ) ;
#41418 = VERTEX_POINT ( 'NONE', #9218 ) ;
#41419 = AXIS2_PLACEMENT_3D ( 'NONE', #7155, #11331, #26342 ) ;
#41420 = ORIENTED_EDGE ( 'NONE', *, *, #11660, .T. ) ;
#41421 = FACE_OUTER_BOUND ( 'NONE', #7528, .T. ) ;
#41422 = CARTESIAN_POINT ( 'NONE',  ( -47.22409385541305937, -12.70920654474410760, 70.13000000000000966 ) ) ;
#41423 = VECTOR ( 'NONE', #23042, 1000.000000000000000 ) ;
#41424 = CARTESIAN_POINT ( 'NONE',  ( -11.28350022557402177, -11.44842874720234427, 64.44882000253240051 ) ) ;
#41425 = CARTESIAN_POINT ( 'NONE',  ( -17.04413539470109740, -21.84925844046378174, 72.45071136019464575 ) ) ;
#41426 = ORIENTED_EDGE ( 'NONE', *, *, #11192, .T. ) ;
#41427 = CARTESIAN_POINT ( 'NONE',  ( -42.92262326717776943, -14.80920654474410547, 59.01176470588234224 ) ) ;
#41428 = CARTESIAN_POINT ( 'NONE',  ( -24.72409385541305582, -14.80920654474427423, 73.99411764705880046 ) ) ;
#41429 = ORIENTED_EDGE ( 'NONE', *, *, #46729, .T. ) ;
#41430 = DIRECTION ( 'NONE',  ( 2.866981220435666553E-17, -1.000000000000000000, -1.190614954331866791E-16 ) ) ;
#41431 = CARTESIAN_POINT ( 'NONE',  ( -19.17437844398820701, -7.979623566120205957, 63.44561363416070776 ) ) ;
#41432 = VERTEX_POINT ( 'NONE', #32103 ) ;
#41433 = CARTESIAN_POINT ( 'NONE',  ( -10.37795889460693033, -14.56696403379599225, 68.14328054657653411 ) ) ;
#41434 = FACE_OUTER_BOUND ( 'NONE', #5862, .T. ) ;
#41435 = CARTESIAN_POINT ( 'NONE',  ( -17.23716279620991187, -7.361383508276583498, 70.63002447061150235 ) ) ;
#41436 = ORIENTED_EDGE ( 'NONE', *, *, #36722, .T. ) ;
#41437 = CARTESIAN_POINT ( 'NONE',  ( -19.78614083979442029, -21.39864764726399216, 69.23482476778590922 ) ) ;
#41438 = EDGE_CURVE ( 'NONE', #454, #6966, #21270, .T. ) ;
#41439 = DIRECTION ( 'NONE',  ( -2.575747231244379256E-06, 1.267954838346457742E-05, 0.9999999999162972886 ) ) ;
#41440 = CARTESIAN_POINT ( 'NONE',  ( -24.72811879990099726, -13.33785195616451169, 59.54923321989076612 ) ) ;
#41441 = CARTESIAN_POINT ( 'NONE',  ( -17.94839601134439633, -19.47832453368858552, 49.52966884056656482 ) ) ;
#41442 = ORIENTED_EDGE ( 'NONE', *, *, #34226, .T. ) ;
#41443 = CARTESIAN_POINT ( 'NONE',  ( -21.24651499925844078, -18.40803921647045982, 52.02966884056656482 ) ) ;
#41444 = CARTESIAN_POINT ( 'NONE',  ( 18.57590614458706924, 0.6652513346187085563, 50.77657095919166608 ) ) ;
#41445 = CARTESIAN_POINT ( 'NONE',  ( -10.74942749874026759, -12.69977847772782376, 61.08388229708562989 ) ) ;
#41446 = AXIS2_PLACEMENT_3D ( 'NONE', #27181, #42203, #12397 ) ;
#41447 = CARTESIAN_POINT ( 'NONE',  ( -23.70015231925135168, -18.82353928378165975, 69.47867257277708575 ) ) ;
#41448 = CARTESIAN_POINT ( 'NONE',  ( -23.90395749478602383, -11.13306750868542316, 70.09199524523918967 ) ) ;
#41449 = EDGE_CURVE ( 'NONE', #34559, #26512, #41966, .T. ) ;
#41450 = EDGE_CURVE ( 'NONE', #26955, #35971, #28444, .T. ) ;
#41451 = CARTESIAN_POINT ( 'NONE',  ( -11.09851747596991700, -11.69606064988821714, 71.09420651392984780 ) ) ;
#41452 = CARTESIAN_POINT ( 'NONE',  ( -18.58659385650551599, -9.302874398569244363, 51.68646062012417985 ) ) ;
#41454 = ADVANCED_FACE ( 'NONE', ( #10190 ), #47126, .F. ) ;
#41453 = VERTEX_POINT ( 'NONE', #28886 ) ;
#41455 = CARTESIAN_POINT ( 'NONE',  ( -24.65023673758593148, -12.99629830290576038, 63.01759453279318279 ) ) ;
#41456 = CARTESIAN_POINT ( 'NONE',  ( -14.54749350918765671, -8.372447261038937327, 64.07506791522041567 ) ) ;
#41457 = ORIENTED_EDGE ( 'NONE', *, *, #45976, .F. ) ;
#41458 = CARTESIAN_POINT ( 'NONE',  ( -11.33913397532896461, -19.10776957548626953, 68.39406486076410374 ) ) ;
#41459 = SHAPE_REPRESENTATION ( 'Tuned Steel Comb Vibration Teeth', ( #29031 ), #42412 ) ;
#41460 = AXIS2_PLACEMENT_3D ( 'NONE', #11461, #45452, #11710 ) ;
#41461 = EDGE_CURVE ( 'NONE', #47803, #7640, #16114, .T. ) ;
#41462 = CARTESIAN_POINT ( 'NONE',  ( -15.43407032490635267, -8.097972375076935236, 74.36520272443641488 ) ) ;
#41463 = CARTESIAN_POINT ( 'NONE',  ( -13.65828898514496359, -20.76952646431350757, 65.00101022825411690 ) ) ;
#41464 = ORIENTED_EDGE ( 'NONE', *, *, #36587, .T. ) ;
#41465 = CARTESIAN_POINT ( 'NONE',  ( -18.39951258112534305, -22.19516185762106275, 69.00009993223443416 ) ) ;
#41466 = CARTESIAN_POINT ( 'NONE',  ( -10.06879755192725412, -15.99802040037407203, 64.62116216602396435 ) ) ;
#41467 = CYLINDRICAL_SURFACE ( 'NONE', #15714, 0.5000000000000004441 ) ;
#41468 = ADVANCED_FACE ( 'NONE', ( #24727 ), #12893, .T. ) ;
#41469 = ORIENTED_EDGE ( 'NONE', *, *, #4246, .F. ) ;
#41470 = CARTESIAN_POINT ( 'NONE',  ( -15.15534385650552096, -7.417179338643134834, 52.18511593390279302 ) ) ;
#41471 = CARTESIAN_POINT ( 'NONE',  ( -20.57278697373333998, -8.057206101692887756, 66.89608655064280640 ) ) ;
#41472 = DIRECTION ( 'NONE',  ( -3.549360974551883545E-17, 6.371834667872732552E-18, 1.000000000000000000 ) ) ;
#41473 = CARTESIAN_POINT ( 'NONE',  ( -24.85158094034050436, -14.23037817089475787, 69.85286472968408589 ) ) ;
#41474 = DIRECTION ( 'NONE',  ( -0.1240347345892086200, 1.145860353393066553E-16, -0.9922778767136676281 ) ) ;
#41475 = EDGE_LOOP ( 'NONE', ( #15314, #40357, #23637, #15672 ) ) ;
#41476 = ORIENTED_EDGE ( 'NONE', *, *, #829, .F. ) ;
#41477 = B_SPLINE_CURVE_WITH_KNOTS ( 'NONE', 1,
 ( #31914, #27732 ),
 .UNSPECIFIED., .F., .F.,
 ( 2, 2 ),
 ( 0.000000000000000000, 1.000000000000000000 ),
 .UNSPECIFIED. ) ;
#41478 = CARTESIAN_POINT ( 'NONE',  ( -14.73659385650551457, -6.915538690918075382, 49.31353937987644542 ) ) ;
#41479 = CARTESIAN_POINT ( 'NONE',  ( -20.25191534917341230, -8.350868906188830820, 70.26572394742477456 ) ) ;
#41480 = CARTESIAN_POINT ( 'NONE',  ( -19.36518065869528726, -8.031383756764064685, 59.97565108339750850 ) ) ;
#41481 = CARTESIAN_POINT ( 'NONE',  ( -14.73659385650551457, -6.915538690918075382, 49.31353937987644542 ) ) ;
#41482 = VECTOR ( 'NONE', #8126, 999.9999999999998863 ) ;
#41483 = CIRCLE ( 'NONE', #578, 0.3999999999999978018 ) ;
#41484 = B_SPLINE_CURVE_WITH_KNOTS ( 'NONE', 3,
 ( #2932, #2216, #47530, #17226, #28575, #32273, #25590, #47293, #9861, #44559 ),
 .UNSPECIFIED., .F., .F.,
 ( 4, 2, 2, 2, 4 ),
 ( 0.000000000000000000, 0.2500000000000000000, 0.5000000000000000000, 0.7500000000000000000, 1.000000000000000000 ),
 .UNSPECIFIED. ) ;
#41485 = CARTESIAN_POINT ( 'NONE',  ( -16.29356323290813435, -7.846682106953448255, 63.97011323776958847 ) ) ;
#41486 = CARTESIAN_POINT ( 'NONE',  ( -10.21805405031902225, -12.91800167290361578, 67.78186406512817541 ) ) ;
#41487 = DIRECTION ( 'NONE',  ( 0.000000000000000000, -0.9999954153791273948, -0.003028072113819838245 ) ) ;
#41488 = VECTOR ( 'NONE', #26193, 1000.000000000000114 ) ;
#41489 = DIRECTION ( 'NONE',  ( -1.674255585786183705E-21, 0.9999746924698832418, 0.007114381193220235301 ) ) ;
#41490 = EDGE_CURVE ( 'NONE', #13929, #38445, #40223, .T. ) ;
#41491 = ORIENTED_EDGE ( 'NONE', *, *, #29731, .T. ) ;
#41492 = DIRECTION ( 'NONE',  ( -5.731567514496413899E-31, -1.020425574103664789E-16, -1.000000000000000000 ) ) ;
#41493 = AXIS2_PLACEMENT_3D ( 'NONE', #44872, #14527, #2993 ) ;
#41494 = ORIENTED_EDGE ( 'NONE', *, *, #22726, .T. ) ;
#41495 = CARTESIAN_POINT ( 'NONE',  ( -13.12790236870489302, -8.721809449924828428, 64.09601920791236296 ) ) ;
#41496 = CARTESIAN_POINT ( 'NONE',  ( -21.12516169987187098, -20.80993955427394582, 69.06922321213187388 ) ) ;
#41497 = DIRECTION ( 'NONE',  ( 0.9375570856950865561, -0.3478314405900308492, 0.000000000000000000 ) ) ;
#41498 = CARTESIAN_POINT ( 'NONE',  ( -17.72634068467203505, -21.85272461955047874, 58.70553378267869249 ) ) ;
#41499 = EDGE_CURVE ( 'NONE', #36571, #27722, #9881, .T. ) ;
#41500 = ORIENTED_EDGE ( 'NONE', *, *, #16489, .T. ) ;
#41501 = FACE_OUTER_BOUND ( 'NONE', #32354, .T. ) ;
#41502 = CARTESIAN_POINT ( 'NONE',  ( -24.42218830102925509, -14.64588410380239480, 62.71296487252168816 ) ) ;
#41503 =( BOUNDED_CURVE ( )  B_SPLINE_CURVE ( 3, ( #28222, #9038, #16875, #47428 ),
 .UNSPECIFIED., .F., .F. ) 
 B_SPLINE_CURVE_WITH_KNOTS ( ( 4, 4 ),
 ( 0.9074455897393589598, 1.000000000000000000 ),
 .UNSPECIFIED. ) 
 CURVE ( )  GEOMETRIC_REPRESENTATION_ITEM ( )  RATIONAL_B_SPLINE_CURVE ( ( 0.6983129098260747458, 0.7760317562606824371, 0.8765941196519908551, 1.000000000000000000 ) ) 
 REPRESENTATION_ITEM ( '' )  );
#41504 = CARTESIAN_POINT ( 'NONE',  ( -20.04802834295863789, -8.319537469032344035, 70.32388470383602908 ) ) ;
#41505 = CARTESIAN_POINT ( 'NONE',  ( -10.07920524814866958, -16.05700196042000272, 68.10050966415293772 ) ) ;
#41506 = ORIENTED_EDGE ( 'NONE', *, *, #25160, .T. ) ;
#41507 = LINE ( 'NONE', #44731, #38556 ) ;
#41508 = CARTESIAN_POINT ( 'NONE',  ( -15.62037199135231980, -25.42245057690201193, 54.61912878955446615 ) ) ;
#41509 = CARTESIAN_POINT ( 'NONE',  ( -18.83585931754296183, -7.494105970839488151, 70.48572750873847781 ) ) ;
#41510 = FACE_BOUND ( 'NONE', #4350, .T. ) ;
#41511 = ORIENTED_EDGE ( 'NONE', *, *, #5297, .T. ) ;
#41512 = CYLINDRICAL_SURFACE ( 'NONE', #39981, 0.1500000000000022704 ) ;
#41513 = CARTESIAN_POINT ( 'NONE',  ( -10.48067290732983281, -16.03043740265091444, 67.97767830707738312 ) ) ;
#41514 = CARTESIAN_POINT ( 'NONE',  ( -10.93232766038821424, -17.55941949638709687, 68.38249893951126523 ) ) ;
#41515 = EDGE_CURVE ( 'NONE', #35967, #11672, #886, .T. ) ;
#41516 = AXIS2_PLACEMENT_3D ( 'NONE', #5233, #6196, #16780 ) ;
#41517 = FACE_OUTER_BOUND ( 'NONE', #11517, .T. ) ;
#41518 = ORIENTED_EDGE ( 'NONE', *, *, #33554, .F. ) ;
#41519 = LINE ( 'NONE', #10999, #23678 ) ;
#41520 = EDGE_CURVE ( 'NONE', #4699, #46319, #41962, .T. ) ;
#41521 = ORIENTED_EDGE ( 'NONE', *, *, #39975, .F. ) ;
#41522 = CARTESIAN_POINT ( 'NONE',  ( -10.34288728022239923, -21.73268535153714254, 53.49999999999995026 ) ) ;
#41523 = CARTESIAN_POINT ( 'NONE',  ( -10.99655737938916289, -18.57624151290433900, 57.99209991576458378 ) ) ;
#41524 = CARTESIAN_POINT ( 'NONE',  ( -21.59992848427141965, -8.639514894543184553, 73.70154514716914207 ) ) ;
#41525 = VERTEX_POINT ( 'NONE', #28166 ) ;
#41526 =( BOUNDED_CURVE ( )  B_SPLINE_CURVE ( 3, ( #30210, #23062, #33613, #44992 ),
 .UNSPECIFIED., .F., .F. ) 
 B_SPLINE_CURVE_WITH_KNOTS ( ( 4, 4 ),
 ( 0.4074455897393624570, 0.5000000000000000000 ),
 .UNSPECIFIED. ) 
 CURVE ( )  GEOMETRIC_REPRESENTATION_ITEM ( )  RATIONAL_B_SPLINE_CURVE ( ( 0.6983129098260937306, 0.7760317562606965369, 0.8765941196519979606, 0.9999999999999963363 ) ) 
 REPRESENTATION_ITEM ( '' )  );
#41527 = AXIS2_PLACEMENT_3D ( 'NONE', #14830, #4045, #14581 ) ;
#41528 = CIRCLE ( 'NONE', #27362, 1.999999999999999334 ) ;
#41529 = EDGE_CURVE ( 'NONE', #12464, #16419, #38494, .T. ) ;
#41530 = LINE ( 'NONE', #15399, #39274 ) ;
#41531 = VERTEX_POINT ( 'NONE', #33044 ) ;
#41532 = ORIENTED_EDGE ( 'NONE', *, *, #28067, .T. ) ;
#41533 = ORIENTED_EDGE ( 'NONE', *, *, #26318, .F. ) ;
#41534 = LINE ( 'NONE', #424, #2890 ) ;
#41535 = DIRECTION ( 'NONE',  ( 0.000000000000000000, 0.000000000000000000, 1.000000000000000000 ) ) ;
#41536 = AXIS2_PLACEMENT_3D ( 'NONE', #8167, #30577, #26880 ) ;
#41537 = CARTESIAN_POINT ( 'NONE',  ( -19.37616851487812752, -21.99900361761337919, 58.71002773933979313 ) ) ;
#41539 = EDGE_CURVE ( 'NONE', #9250, #5475, #43550, .T. ) ;
#41538 = CARTESIAN_POINT ( 'NONE',  ( -10.57910610510154470, -13.34370840258270441, 74.97817676091081296 ) ) ;
#41540 = CARTESIAN_POINT ( 'NONE',  ( -18.98034385541304303, -9.360768649638925964, 51.01397948905978552 ) ) ;
#41541 = CARTESIAN_POINT ( 'NONE',  ( -14.21691873732594402, -8.585707597842299421, 74.27124835653124535 ) ) ;
#41542 = DIRECTION ( 'NONE',  ( 1.424565731581784133E-06, -1.060674514654238452E-05, 0.9999999999427338082 ) ) ;
#41543 = CIRCLE ( 'NONE', #7743, 5.249999999999998224 ) ;
#41544 =( BOUNDED_CURVE ( )  B_SPLINE_CURVE ( 1, ( #14097, #2567 ),
 .UNSPECIFIED., .F., .F. ) 
 B_SPLINE_CURVE_WITH_KNOTS ( ( 2, 2 ),
 ( 0.000000000000000000, 1.000000000000000000 ),
 .UNSPECIFIED. ) 
 CURVE ( )  GEOMETRIC_REPRESENTATION_ITEM ( )  RATIONAL_B_SPLINE_CURVE ( ( 0.9847233224627454096, 0.9847233224627454096 ) ) 
 REPRESENTATION_ITEM ( '' )  );
#41545 = ORIENTED_EDGE ( 'NONE', *, *, #6056, .F. ) ;
#41546 = EDGE_LOOP ( 'NONE', ( #11781, #35821, #23341, #6874, #3458 ) ) ;
#41547 = CARTESIAN_POINT ( 'NONE',  ( -17.56717618076180187, -7.360494862701306928, 63.73552352176282909 ) ) ;
#41548 = CARTESIAN_POINT ( 'NONE',  ( -11.86838291625971742, -9.845553222893467904, 64.14418898700822069 ) ) ;
#41549 = DIRECTION ( 'NONE',  ( 0.9893521221787096032, -0.1455416721783832079, -6.188545272020241572E-08 ) ) ;
#41550 = PLANE ( 'NONE',  #46478 ) ;
#41551 = ORIENTED_EDGE ( 'NONE', *, *, #29829, .T. ) ;
#41552 = CARTESIAN_POINT ( 'NONE',  ( -15.60534385650551847, -8.801233750844183135, 48.81488406609782515 ) ) ;
#41553 = B_SPLINE_CURVE_WITH_KNOTS ( 'NONE', 3,
 ( #38414, #520, #34733, #45111, #33746, #22436, #11357, #37430, #3979, #3725 ),
 .UNSPECIFIED., .F., .F.,
 ( 4, 2, 2, 2, 4 ),
 ( 0.000000000000000000, 0.2500000000000000000, 0.5000000000000000000, 0.7500000000000000000, 1.000000000000000000 ),
 .UNSPECIFIED. ) ;
#41554 = ORIENTED_EDGE ( 'NONE', *, *, #46908, .F. ) ;
#41555 = CARTESIAN_POINT ( 'NONE',  ( -10.41531639268335496, -14.04517892474411589, 60.93293405735092705 ) ) ;
#41556 = CARTESIAN_POINT ( 'NONE',  ( 18.57590614458695200, 0.6315104036983664182, 50.27646649643033783 ) ) ;
#41557 = CIRCLE ( 'NONE', #44696, 1.250000000000001998 ) ;
#41558 = STYLED_ITEM ( 'NONE', ( #27243 ), #48318 ) ;
#41559 = ADVANCED_FACE ( 'NONE', ( #74 ), #48089, .T. ) ;
#41560 = VERTEX_POINT ( 'NONE', #25443 ) ;
#41561 = CARTESIAN_POINT ( 'NONE',  ( -16.39887994223181167, -21.73372354711506560, 61.75568132718285597 ) ) ;
#41562 = VECTOR ( 'NONE', #46502, 1000.000000000000227 ) ;
#41563 = AXIS2_PLACEMENT_3D ( 'NONE', #16427, #27521, #23843 ) ;
#41564 = CARTESIAN_POINT ( 'NONE',  ( -10.47368616940683772, -17.49164935309025282, 64.67093470525151133 ) ) ;
#41565 = CARTESIAN_POINT ( 'NONE',  ( -24.18257650347943866, -11.67453741916809662, 59.58897441446281817 ) ) ;
#41566 = ORIENTED_EDGE ( 'NONE', *, *, #46092, .T. ) ;
#41567 = AXIS2_PLACEMENT_3D ( 'NONE', #43954, #36041, #32606 ) ;
#41568 = LINE ( 'NONE', #45520, #42274 ) ;
#41569 = CARTESIAN_POINT ( 'NONE',  ( -10.06879755192725412, -15.99802040037407203, 64.62116216602396435 ) ) ;
#41570 = LINE ( 'NONE', #7853, #4052 ) ;
#41571 = EDGE_LOOP ( 'NONE', ( #24535, #42806, #45433, #4114 ) ) ;
#41572 = CARTESIAN_POINT ( 'NONE',  ( -16.04133765461606842, -7.488482771185046794, 63.80977704063102607 ) ) ;
#41573 = ORIENTED_EDGE ( 'NONE', *, *, #30490, .T. ) ;
#41574 = CARTESIAN_POINT ( 'NONE',  ( -12.85925802207596114, -13.69662874518197171, 49.52966884056655772 ) ) ;
#41575 = CARTESIAN_POINT ( 'NONE',  ( -24.27661814142333796, -16.49973396376381984, 62.73761853866894711 ) ) ;
#41576 = VERTEX_POINT ( 'NONE', #14553 ) ;
#41577 = CARTESIAN_POINT ( 'NONE',  ( -12.43150676794136089, -13.18545343111793855, 52.02966884056656482 ) ) ;
#41578 = CARTESIAN_POINT ( 'NONE',  ( -20.60192465206874246, -18.25372010660273503, 49.52966884056656482 ) ) ;
#41579 = CARTESIAN_POINT ( 'NONE',  ( -20.29576920503309623, -8.423958534466374104, 70.47930128339966416 ) ) ;
#41580 = EDGE_CURVE ( 'NONE', #501, #9159, #15383, .T. ) ;
#41581 = ORIENTED_EDGE ( 'NONE', *, *, #6660, .T. ) ;
#41582 = DIRECTION ( 'NONE',  ( 0.7800143876985550229, -0.6257615799833393666, 5.505484597913564244E-08 ) ) ;
#41583 = DIRECTION ( 'NONE',  ( 1.927470528863119542E-16, 0.000000000000000000, -1.000000000000000000 ) ) ;
#41584 = FACE_OUTER_BOUND ( 'NONE', #103, .T. ) ;
#41585 = EDGE_LOOP ( 'NONE', ( #35494, #40657, #44990, #14335, #38423 ) ) ;
#41586 = CARTESIAN_POINT ( 'NONE',  ( -11.10470791607724550, -18.75498134223953883, 61.46206221440264983 ) ) ;
#41587 = EDGE_CURVE ( 'NONE', #6672, #7125, #37221, .T. ) ;
#41588 = CARTESIAN_POINT ( 'NONE',  ( -21.25455046938168735, -8.881090050001144931, 70.28699408244519020 ) ) ;
#41589 = ORIENTED_EDGE ( 'NONE', *, *, #29043, .F. ) ;
#41590 = ORIENTED_EDGE ( 'NONE', *, *, #3580, .T. ) ;
#41591 = CARTESIAN_POINT ( 'NONE',  ( -10.47299162366406478, -15.63514707757639854, 61.33789045486464886 ) ) ;
#41592 = DIRECTION ( 'NONE',  ( -5.731567514496413899E-31, -1.020425574103664789E-16, -1.000000000000000000 ) ) ;
#41594 = PLANE ( 'NONE',  #5261 ) ;
#41593 = AXIS2_PLACEMENT_3D ( 'NONE', #19784, #38723, #31098 ) ;
#41595 = FILL_AREA_STYLE_COLOUR ( '', #38579 ) ;
#41596 = ADVANCED_FACE ( 'NONE', ( #41421 ), #29374, .F. ) ;
#41597 = CARTESIAN_POINT ( 'NONE',  ( -21.51159385650551670, -6.922745924619793101, 51.69366785382590024 ) ) ;
#41598 = AXIS2_PLACEMENT_3D ( 'NONE', #32907, #29477, #13474 ) ;
#41599 = DIRECTION ( 'NONE',  ( -3.071710424422018668E-17, 6.404604876783312462E-16, 1.000000000000000000 ) ) ;
#41600 = CARTESIAN_POINT ( 'NONE',  ( -10.70566866894272984, -16.94585410378973123, 57.98760548748136046 ) ) ;
#41601 = AXIS2_PLACEMENT_3D ( 'NONE', #44172, #3005, #35768 ) ;
#41602 = AXIS2_PLACEMENT_3D ( 'NONE', #16277, #1042, #8429 ) ;
#41603 = CARTESIAN_POINT ( 'NONE',  ( -9.974215857974789046, -14.86484893678357544, 74.91283499353951925 ) ) ;
#41604 = ORIENTED_EDGE ( 'NONE', *, *, #25555, .T. ) ;
#41605 = CARTESIAN_POINT ( 'NONE',  ( -20.37299750454370439, -8.405577324698718655, 66.78104082189589974 ) ) ;
#41606 = CARTESIAN_POINT ( 'NONE',  ( -19.39856565954547207, -21.58093498248654996, 65.76486340091366856 ) ) ;
#41607 = CARTESIAN_POINT ( 'NONE',  ( -21.84382042562961246, -9.380945574151434485, 59.91274429023591352 ) ) ;
#41608 = EDGE_CURVE ( 'NONE', #12328, #24536, #14359, .T. ) ;
#41609 = ORIENTED_EDGE ( 'NONE', *, *, #9276, .T. ) ;
#41610 = EDGE_CURVE ( 'NONE', #18022, #4434, #30805, .T. ) ;
#41611 = ORIENTED_EDGE ( 'NONE', *, *, #44912, .T. ) ;
#41612 = ADVANCED_FACE ( 'NONE', ( #44645 ), #40938, .T. ) ;
#41613 = CARTESIAN_POINT ( 'NONE',  ( -23.40706704545067041, -18.44294168544361057, 72.76368236816873036 ) ) ;
#41614 = DIRECTION ( 'NONE',  ( -0.2771212459065067191, 0.9608349572466771127, 4.100231986695772107E-08 ) ) ;
#41615 = CARTESIAN_POINT ( 'NONE',  ( -13.29845767883066543, -21.01266560759323809, 61.63150935275904629 ) ) ;
#41616 = CARTESIAN_POINT ( 'NONE',  ( -14.87409385541153917, -6.859212275519794844, 50.50378509015643402 ) ) ;
#41617 = ORIENTED_EDGE ( 'NONE', *, *, #813, .F. ) ;
#41618 = CARTESIAN_POINT ( 'NONE',  ( -10.61330328728660533, -12.98831903967553636, 67.73832347272893628 ) ) ;
#41619 = FACE_OUTER_BOUND ( 'NONE', #41294, .T. ) ;
#41620 = EDGE_LOOP ( 'NONE', ( #19816, #32049, #7385, #38146 ) ) ;
#41621 = CARTESIAN_POINT ( 'NONE',  ( -14.80056147340629380, -21.78207226143426922, 61.82095877133116346 ) ) ;
#41622 = CIRCLE ( 'NONE', #31391, 2.000000000000000444 ) ;
#41623 = DIRECTION ( 'NONE',  ( 1.000000000000000000, -4.164305804376849172E-17, 1.614929280266638808E-16 ) ) ;
#41624 = AXIS2_PLACEMENT_3D ( 'NONE', #12527, #12999, #27554 ) ;
#41625 = LINE ( 'NONE', #18465, #24948 ) ;
#41626 = ORIENTED_EDGE ( 'NONE', *, *, #22288, .F. ) ;
#41627 = CARTESIAN_POINT ( 'NONE',  ( -12.30444741248500051, -20.22242042389802918, 64.98019641849691652 ) ) ;
#41628 = AXIS2_PLACEMENT_3D ( 'NONE', #3871, #33891, #29715 ) ;
#41629 = VECTOR ( 'NONE', #8395, 1000.000000000000000 ) ;
#41630 = ORIENTED_EDGE ( 'NONE', *, *, #37603, .F. ) ;
#41631 = DIRECTION ( 'NONE',  ( -3.071710424422018668E-17, 6.404604876783312462E-16, 1.000000000000000000 ) ) ;
#41632 = DIRECTION ( 'NONE',  ( -3.071710424422018668E-17, 6.404604876783312462E-16, 1.000000000000000000 ) ) ;
#41633 = ORIENTED_EDGE ( 'NONE', *, *, #35045, .T. ) ;
#41634 = CARTESIAN_POINT ( 'NONE',  ( -50.42609385541305755, -14.80920654474422271, 68.06470588235292496 ) ) ;
#41635 = CARTESIAN_POINT ( 'NONE',  ( -21.59909385650551528, -8.114302828567740988, 52.18300498402516041 ) ) ;
#41636 = CARTESIAN_POINT ( 'NONE',  ( -17.68496342731873483, -21.80445415968011247, 58.40553376440286115 ) ) ;
#41637 = DIRECTION ( 'NONE',  ( -0.4501286257827956661, -0.8929637284072021730, 1.500157795982635103E-08 ) ) ;
#41638 = CARTESIAN_POINT ( 'NONE',  ( -22.20320197231171733, -19.92390356480266433, 66.00421731406686376 ) ) ;
#41639 = DIRECTION ( 'NONE',  ( -9.637352644315596475E-17, 0.000000000000000000, -1.000000000000000000 ) ) ;
#41640 = ORIENTED_EDGE ( 'NONE', *, *, #42600, .T. ) ;
#41641 = CARTESIAN_POINT ( 'NONE',  ( -30.42409385541305156, -6.859206544744110623, 47.99999999999997868 ) ) ;
#41642 = CARTESIAN_POINT ( 'NONE',  ( -12.52476177601987040, -19.87868524014693605, 65.16674890854918090 ) ) ;
#41643 = ADVANCED_FACE ( 'NONE', ( #317 ), #45630, .T. ) ;
#41644 = CARTESIAN_POINT ( 'NONE',  ( -45.42186609336205549, -13.24559821555319239, 70.13000000000000966 ) ) ;
#41645 = CARTESIAN_POINT ( 'NONE',  ( -17.20139249542113191, -7.812750000685961815, 70.49035839633111777 ) ) ;
#41646 = ORIENTED_EDGE ( 'NONE', *, *, #37354, .F. ) ;
#41647 = VERTEX_POINT ( 'NONE', #12596 ) ;
#41648 = ADVANCED_FACE ( 'NONE', ( #8196 ), #38878, .T. ) ;
#41649 = CARTESIAN_POINT ( 'NONE',  ( -21.36950656924352288, -9.026883429518402835, 73.90128804929361195 ) ) ;
#41650 = CARTESIAN_POINT ( 'NONE',  ( -14.66963140629840190, -7.887024584555132556, 60.57642187187276051 ) ) ;
#41651 = ORIENTED_EDGE ( 'NONE', *, *, #44238, .F. ) ;
#41652 = CARTESIAN_POINT ( 'NONE',  ( -20.99144087168200912, -21.34977411167369610, 62.27617921724772998 ) ) ;
#41653 = CARTESIAN_POINT ( 'NONE',  ( -24.71334378318632830, -13.26952680650525274, 59.47772536435775947 ) ) ;
#41654 = CARTESIAN_POINT ( 'NONE',  ( -10.27345454978659944, -12.71824136398891980, 64.45331520391344782 ) ) ;
#41655 = CARTESIAN_POINT ( 'NONE',  ( -10.45256735519816615, -15.43993469624229853, 57.56792809193251514 ) ) ;
#41656 =( BOUNDED_CURVE ( )  B_SPLINE_CURVE ( 3, ( #303, #7446, #21719, #25650 ),
 .UNSPECIFIED., .F., .F. ) 
 B_SPLINE_CURVE_WITH_KNOTS ( ( 4, 4 ),
 ( 0.000000000000000000, 0.4074455897393669535 ),
 .UNSPECIFIED. ) 
 CURVE ( )  GEOMETRIC_REPRESENTATION_ITEM ( )  RATIONAL_B_SPLINE_CURVE ( ( 1.000000000000000000, 0.4567392136813300807, 0.3561768502900296007, 0.6983129098260987266 ) ) 
 REPRESENTATION_ITEM ( '' )  );
#41657 = CARTESIAN_POINT ( 'NONE',  ( -21.53861794036900079, -21.02004141303368101, 72.63951040967180006 ) ) ;
#41658 = CARTESIAN_POINT ( 'NONE',  ( -23.57293185872052632, -19.01568291639688724, 65.92365791119206619 ) ) ;
#41659 = DIRECTION ( 'NONE',  ( 1.000000000000000000, -4.164305804376849788E-17, 1.614929280266638808E-16 ) ) ;
#41660 = DIRECTION ( 'NONE',  ( -0.6380325334150318550, 0.7700094066334490783, 0.000000000000000000 ) ) ;
#41661 = CIRCLE ( 'NONE', #48716, 5.249999999999998224 ) ;
#41662 = CARTESIAN_POINT ( 'NONE',  ( -10.56492563526530759, -13.18000101695786341, 71.20828586226983248 ) ) ;
#41663 = CARTESIAN_POINT ( 'NONE',  ( -40.92409385541305511, -14.80920654474410725, 74.99999999999998579 ) ) ;
#41664 = CARTESIAN_POINT ( 'NONE',  ( -24.16627971075339332, -12.73851560842801867, 66.18757903754330130 ) ) ;
#41665 =( BOUNDED_CURVE ( )  B_SPLINE_CURVE ( 3, ( #16773, #44125, #21216, #2008 ),
 .UNSPECIFIED., .F., .F. ) 
 B_SPLINE_CURVE_WITH_KNOTS ( ( 4, 4 ),
 ( 0.9074455897393635118, 1.000000000000000000 ),
 .UNSPECIFIED. ) 
 CURVE ( )  GEOMETRIC_REPRESENTATION_ITEM ( )  RATIONAL_B_SPLINE_CURVE ( ( 0.6983129098260841827, 0.7760317562606905417, 0.8765941196519958512, 1.000000000000000000 ) ) 
 REPRESENTATION_ITEM ( '' )  );
#41666 = CARTESIAN_POINT ( 'NONE',  ( -33.42409385541304800, -6.859212275519750435, 50.50378509014258555 ) ) ;
#41667 = VECTOR ( 'NONE', #20826, 1000.000000000000114 ) ;
#41669 = ORIENTED_EDGE ( 'NONE', *, *, #14171, .T. ) ;
#41668 = EDGE_CURVE ( 'NONE', #28824, #4171, #48386, .T. ) ;
#41670 = ORIENTED_EDGE ( 'NONE', *, *, #14894, .T. ) ;
#41671 = CARTESIAN_POINT ( 'NONE',  ( -15.32409385541304303, -9.359200813967568422, 50.49621490985803263 ) ) ;
#41672 = VERTEX_POINT ( 'NONE', #23935 ) ;
#41673 = EDGE_CURVE ( 'NONE', #1437, #9257, #19758, .T. ) ;
#41674 = EDGE_CURVE ( 'NONE', #19332, #16810, #37267, .T. ) ;
#41675 = ADVANCED_FACE ( 'NONE', ( #37966 ), #30852, .T. ) ;
#41676 = CARTESIAN_POINT ( 'NONE',  ( -22.97409385541299542, -6.859212275519753099, 50.50378509014307582 ) ) ;
#41677 = CARTESIAN_POINT ( 'NONE',  ( -10.52215064345839757, -13.37195933026064232, 74.82817647370434599 ) ) ;
#41678 = VECTOR ( 'NONE', #4065, 1000.000000000000000 ) ;
#41679 =( BOUNDED_SURFACE ( )  B_SPLINE_SURFACE ( 3, 1, ( 
 ( #25089, #32701 ),
 ( #47729, #6614 ),
 ( #40109, #14211 ),
 ( #39617, #47498 ),
 ( #13967, #32239 ),
 ( #29016, #44064 ),
 ( #35904, #13248 ) ),
 .UNSPECIFIED., .T., .F., .F. ) 
 B_SPLINE_SURFACE_WITH_KNOTS ( ( 4, 3, 4 ),
 ( 2, 2 ),
 ( 0.000000000000000000, 0.5000000000000000000, 1.000000000000000000 ),
 ( 0.000000000000000000, 1.000000000000000000 ),
 .UNSPECIFIED. ) 
 GEOMETRIC_REPRESENTATION_ITEM ( )  RATIONAL_B_SPLINE_SURFACE ( (
 ( 1.000000000000000000, 1.000000000000000000),
 ( 0.3333333333333335369, 0.3333333333333330373),
 ( 0.3333333333333335369, 0.3333333333333330373),
 ( 1.000000000000000000, 1.000000000000000000),
 ( 0.3333333333333333703, 0.3333333333333333703),
 ( 0.3333333333333333703, 0.3333333333333333703),
 ( 1.000000000000000000, 1.000000000000000000) ) ) 
 REPRESENTATION_ITEM ( '' )  SURFACE ( )  );
#41680 = CARTESIAN_POINT ( 'NONE',  ( -13.61216739602634007, -20.68217155920894967, 65.17556062011875895 ) ) ;
#41681 = DIRECTION ( 'NONE',  ( -0.3478314405900341799, -0.9375570856950852239, 0.000000000000000000 ) ) ;
#41682 = VECTOR ( 'NONE', #30024, 1000.000000000000227 ) ;
#41683 = EDGE_LOOP ( 'NONE', ( #5025, #48165 ) ) ;
#41684 = CARTESIAN_POINT ( 'NONE',  ( -13.95528965362524332, -21.40322351219866093, 72.03952346373179694 ) ) ;
#41685 = CARTESIAN_POINT ( 'NONE',  ( -18.59601872632196518, -7.856991649524070809, 73.85536540707786912 ) ) ;
#41686 = ORIENTED_EDGE ( 'NONE', *, *, #14473, .F. ) ;
#41687 = CARTESIAN_POINT ( 'NONE',  ( -11.47316209429933132, -11.02906371526824536, 57.20903242655475651 ) ) ;
#41688 = DIRECTION ( 'NONE',  ( -3.071710424422018668E-17, 6.404604876783312462E-16, 1.000000000000000000 ) ) ;
#41689 = ORIENTED_EDGE ( 'NONE', *, *, #32969, .T. ) ;
#41690 = CARTESIAN_POINT ( 'NONE',  ( -24.47432067347917695, -14.77756146504815327, 59.52828185648635184 ) ) ;
#41691 = DIRECTION ( 'NONE',  ( 1.000000000000000000, -4.164305804376849788E-17, 1.614929280266638808E-16 ) ) ;
#41692 = CARTESIAN_POINT ( 'NONE',  ( -24.72409385541305582, -14.80920654474414810, 61.92352941176469727 ) ) ;
#41693 = ORIENTED_EDGE ( 'NONE', *, *, #31431, .F. ) ;
#41694 = CARTESIAN_POINT ( 'NONE',  ( -23.20398631485561225, -10.10837353526244087, 63.21039459454670606 ) ) ;
#41695 = ADVANCED_FACE ( 'NONE', ( #27375 ), #27134, .T. ) ;
#41696 = DIRECTION ( 'NONE',  ( 1.000000000000000000, 2.866981220435666553E-17, 0.000000000000000000 ) ) ;
#41697 = AXIS2_PLACEMENT_3D ( 'NONE', #17683, #6134, #13737 ) ;
#41698 = VECTOR ( 'NONE', #41691, 1000.000000000000000 ) ;
#41699 = CARTESIAN_POINT ( 'NONE',  ( -16.11719258475605443, -7.932175852977164432, 63.67011080781733057 ) ) ;
#41700 = CARTESIAN_POINT ( 'NONE',  ( -24.47405849404658795, -12.40054206295432770, 73.28579645182460922 ) ) ;
#41701 = VERTEX_POINT ( 'NONE', #30605 ) ;
#41702 = CARTESIAN_POINT ( 'NONE',  ( -11.08030728566740741, -11.72680384936461806, 74.97328630331448096 ) ) ;
#41703 = CARTESIAN_POINT ( 'NONE',  ( -15.81235419205221504, -7.945607373518417837, 67.42535135806457447 ) ) ;
#41704 = AXIS2_PLACEMENT_3D ( 'NONE', #11414, #7747, #581 ) ;
#41705 = DIRECTION ( 'NONE',  ( -5.551115123125782702E-17, -1.232595164407830946E-32, -1.000000000000000000 ) ) ;
#41706 = CARTESIAN_POINT ( 'NONE',  ( -23.93425983466340057, -11.18667287686709777, 70.03177400573818545 ) ) ;
#41707 = CARTESIAN_POINT ( 'NONE',  ( -10.47914967500843986, -15.69558290523237076, 64.57941926453548831 ) ) ;
#41708 = CARTESIAN_POINT ( 'NONE',  ( -20.66784385650552025, -6.428312510596449592, 51.20221977374900035 ) ) ;
#41709 = ORIENTED_EDGE ( 'NONE', *, *, #47185, .F. ) ;
#41710 = ADVANCED_FACE ( 'NONE', ( #4982 ), #3637, .T. ) ;
#41711 = CARTESIAN_POINT ( 'NONE',  ( -11.03962565240155591, -10.96946996027528876, 60.81852449360508928 ) ) ;
#41712 = ORIENTED_EDGE ( 'NONE', *, *, #37651, .F. ) ;
#41713 = CARTESIAN_POINT ( 'NONE',  ( -24.43817019563415371, -15.55591454009146979, 69.53307225875056474 ) ) ;
#41714 = VECTOR ( 'NONE', #35827, 1000.000000000000000 ) ;
#41715 = CARTESIAN_POINT ( 'NONE',  ( -21.59909385759798894, -8.105421454601382081, 49.25000573077640098 ) ) ;
#41716 = CARTESIAN_POINT ( 'NONE',  ( -18.41501299910237677, -20.23286350246260312, 53.88362224778186516 ) ) ;
#41717 = EDGE_LOOP ( 'NONE', ( #44441, #4690, #14848, #8913 ) ) ;
#41718 = CARTESIAN_POINT ( 'NONE',  ( -16.95423314674965098, -22.24437505095468026, 72.31543220464045874 ) ) ;
#41719 = CARTESIAN_POINT ( 'NONE',  ( -17.26457240846633923, -7.760713630915982542, 70.50507891880883449 ) ) ;
#41720 = CARTESIAN_POINT ( 'NONE',  ( -18.33614212499659502, -22.20322161997698629, 68.92240557158177694 ) ) ;
#41721 = VERTEX_POINT ( 'NONE', #46591 ) ;
#41722 = CARTESIAN_POINT ( 'NONE',  ( -16.44909385650551670, -8.104110260919579645, 48.81699501597546487 ) ) ;
#41723 = CYLINDRICAL_SURFACE ( 'NONE', #46831, 1.249999999999998668 ) ;
#41724 = FACE_OUTER_BOUND ( 'NONE', #32678, .T. ) ;
#41725 = CARTESIAN_POINT ( 'NONE',  ( -16.01003035779492834, -7.894338788008341545, 70.75422978485266867 ) ) ;
#41726 = DIRECTION ( 'NONE',  ( 0.3109111061729913916, 0.9504389954427825415, 3.354176643444177759E-08 ) ) ;
#41727 = EDGE_LOOP ( 'NONE', ( #42638, #19841, #40192, #16798, #39629 ) ) ;
#41728 = VERTEX_POINT ( 'NONE', #35956 ) ;
#41729 = CARTESIAN_POINT ( 'NONE',  ( -16.42409385650551812, -6.426201560718813433, 50.50509628382439331 ) ) ;
#41730 = EDGE_CURVE ( 'NONE', #1862, #21555, #28592, .T. ) ;
#41731 = ADVANCED_FACE ( 'NONE', ( #10116 ), #5465, .T. ) ;
#41732 = FACE_OUTER_BOUND ( 'NONE', #21325, .T. ) ;
#41733 = AXIS2_PLACEMENT_3D ( 'NONE', #3227, #25880, #39515 ) ;
#41734 = CARTESIAN_POINT ( 'NONE',  ( -10.52991701743181174, -16.02177613136639067, 67.97767831076122036 ) ) ;
#41735 = CARTESIAN_POINT ( 'NONE',  ( -18.96529421678551230, -7.929577530235508043, 66.90631605115711977 ) ) ;
#41736 = CARTESIAN_POINT ( 'NONE',  ( -14.23034385650551492, -9.794322478646142471, 51.19202720610083901 ) ) ;
#41737 = AXIS2_PLACEMENT_3D ( 'NONE', #35123, #27261, #34882 ) ;
#41738 = EDGE_CURVE ( 'NONE', #733, #48469, #39430, .T. ) ;
#41739 = PRODUCT_DEFINITION_SHAPE ( 'NONE', 'NONE',  #9649 ) ;
#41740 = EDGE_CURVE ( 'NONE', #43099, #7039, #10808, .T. ) ;
#41741 = CARTESIAN_POINT ( 'NONE',  ( -13.75179125342063458, -11.87837916245159953, 49.52966884056655772 ) ) ;
#41742 = DIRECTION ( 'NONE',  ( -6.023555224489876859E-06, 1.003033500230846996E-05, -0.9999999999315546395 ) ) ;
#41743 = ADVANCED_FACE ( 'NONE', ( #9155 ), #1998, .T. ) ;
#41744 = FACE_OUTER_BOUND ( 'NONE', #29807, .T. ) ;
#41745 = AXIS2_PLACEMENT_3D ( 'NONE', #44772, #14194, #3140 ) ;
#41746 = CARTESIAN_POINT ( 'NONE',  ( -24.30048669258562200, -16.36410883687464946, 59.42332431756338451 ) ) ;
#41747 = ORIENTED_EDGE ( 'NONE', *, *, #3947, .T. ) ;
#41748 = DIRECTION ( 'NONE',  ( 0.000000000000000000, 1.000000000000000000, -0.000000000000000000 ) ) ;
#41749 = VERTEX_POINT ( 'NONE', #20484 ) ;
#41750 = CARTESIAN_POINT ( 'NONE',  ( -22.17046091269999764, -9.065891900838490614, 59.83515915777798710 ) ) ;
#41751 = CARTESIAN_POINT ( 'NONE',  ( -13.65684165595416921, -8.849801312179289781, 56.98439896120441261 ) ) ;
#41752 = CARTESIAN_POINT ( 'NONE',  ( -12.53241260230162624, -9.190070326428815051, 74.42584683763180919 ) ) ;
#41753 = LINE ( 'NONE', #31144, #255 ) ;
#41754 = EDGE_CURVE ( 'NONE', #20983, #42591, #6790, .T. ) ;
#41755 = VECTOR ( 'NONE', #11167, 1000.000000000000000 ) ;
#41756 = ORIENTED_EDGE ( 'NONE', *, *, #18650, .T. ) ;
#41757 = DIRECTION ( 'NONE',  ( -3.071710424422018668E-17, 6.404604876783312462E-16, 1.000000000000000000 ) ) ;
#41758 = LINE ( 'NONE', #4329, #31299 ) ;
#41759 =( BOUNDED_CURVE ( )  B_SPLINE_CURVE ( 3, ( #29220, #2860, #28500, #17633 ),
 .UNSPECIFIED., .F., .F. ) 
 B_SPLINE_CURVE_WITH_KNOTS ( ( 4, 4 ),
 ( 0.4074455897393630122, 0.5000000000000000000 ),
 .UNSPECIFIED. ) 
 CURVE ( )  GEOMETRIC_REPRESENTATION_ITEM ( )  RATIONAL_B_SPLINE_CURVE ( ( 0.6983129098260898449, 0.7760317562606893205, 0.8765941196519910772, 0.9999999999999903411 ) ) 
 REPRESENTATION_ITEM ( '' )  );
#41760 = DIRECTION ( 'NONE',  ( -0.6973657521612036669, 0.7167154300785205656, -1.015100525525034718E-08 ) ) ;
#41761 = CARTESIAN_POINT ( 'NONE',  ( -24.48057421083657914, -17.19850309837678637, 72.98312409556710634 ) ) ;
#41762 = VERTEX_POINT ( 'NONE', #13061 ) ;
#41763 = CARTESIAN_POINT ( 'NONE',  ( -10.55442330881768775, -17.69226200592865794, 68.27438864859273338 ) ) ;
#41764 = CARTESIAN_POINT ( 'NONE',  ( -10.97586111044497947, -17.65935802862028936, 71.56718190231987364 ) ) ;
#41765 = PLANE ( 'NONE',  #20766 ) ;
#41766 = FACE_BOUND ( 'NONE', #33677, .T. ) ;
#41767 = ITEM_DEFINED_TRANSFORMATION ( 'NONE', 'NONE', #41624,  #29031 ) ;
#41768 = ORIENTED_EDGE ( 'NONE', *, *, #35181, .F. ) ;
#41769 = CIRCLE ( 'NONE', #15798, 1.999999999999999556 ) ;
#41770 = CARTESIAN_POINT ( 'NONE',  ( -21.18000274887674905, -20.77541536365158592, 69.05450184741354747 ) ) ;
#41771 = CARTESIAN_POINT ( 'NONE',  ( -14.36784385541283982, -9.357632978295985282, 49.97845033065656395 ) ) ;
#41772 = CYLINDRICAL_SURFACE ( 'NONE', #39170, 1.999999999999994893 ) ;
#41773 = CARTESIAN_POINT ( 'NONE',  ( -21.61813247623101830, -8.651786778886961571, 73.71633474065167491 ) ) ;
#41774 = ORIENTED_EDGE ( 'NONE', *, *, #43521, .T. ) ;
#41775 = ORIENTED_EDGE ( 'NONE', *, *, #11533, .F. ) ;
#41776 = DIRECTION ( 'NONE',  ( -0.2122660683108583690, 0.9772119095896469876, -7.504255179299140299E-08 ) ) ;
#41777 = CARTESIAN_POINT ( 'NONE',  ( -22.96794543296044466, -10.53327132317364168, 63.30015916732239845 ) ) ;
#41778 = DIRECTION ( 'NONE',  ( -0.9660698163281070672, -0.2582810677919976095, 5.363434502754640132E-08 ) ) ;
#41779 = ORIENTED_EDGE ( 'NONE', *, *, #11699, .T. ) ;
#41780 = VECTOR ( 'NONE', #32050, 1000.000000000000114 ) ;
#41781 = CARTESIAN_POINT ( 'NONE',  ( -21.95523322170430092, -8.895446802377390938, 66.77654591769551473 ) ) ;
#41782 = ORIENTED_EDGE ( 'NONE', *, *, #14808, .T. ) ;
#41783 = ORIENTED_EDGE ( 'NONE', *, *, #30783, .T. ) ;
#41784 = ORIENTED_EDGE ( 'NONE', *, *, #37268, .F. ) ;
#41785 = CARTESIAN_POINT ( 'NONE',  ( -6.424093855413055110, -6.859206544744110623, 45.99999999999998579 ) ) ;
#41786 = CARTESIAN_POINT ( 'NONE',  ( -23.30963478160716562, -18.69084381296369557, 69.30844128244088154 ) ) ;
#41787 = VECTOR ( 'NONE', #21272, 1000.000000000000000 ) ;
#41788 = CARTESIAN_POINT ( 'NONE',  ( -21.18842005097459591, -20.71103373205295028, 69.05450136001277883 ) ) ;
#41789 = CARTESIAN_POINT ( 'NONE',  ( -23.46741973463711872, -19.16603908095663655, 62.53902270128352825 ) ) ;
#41790 = EDGE_CURVE ( 'NONE', #41056, #44086, #19632, .T. ) ;
#41791 = CARTESIAN_POINT ( 'NONE',  ( -12.41310947992116098, -19.76871611099698001, 61.68206578716802113 ) ) ;
#41792 = CARTESIAN_POINT ( 'NONE',  ( -6.424093855413058662, -6.359206544744109735, 52.99999999999998579 ) ) ;
#41793 = CARTESIAN_POINT ( 'NONE',  ( -22.56207008003183745, -19.63703213565221262, 72.92928497383269359 ) ) ;
#41794 = ORIENTED_EDGE ( 'NONE', *, *, #23257, .T. ) ;
#41795 = EDGE_LOOP ( 'NONE', ( #14839, #44717 ) ) ;
#41796 = CARTESIAN_POINT ( 'NONE',  ( -12.26752988409003642, -16.72227946798956921, 54.07175714974876968 ) ) ;
#41797 = ADVANCED_FACE ( 'NONE', ( #24893 ), #43934, .T. ) ;
#41798 = CIRCLE ( 'NONE', #15001, 0.1000000000000000056 ) ;
#41799 = CARTESIAN_POINT ( 'NONE',  ( -10.36816553299425792, -14.63937932467125691, 64.54370954096965818 ) ) ;
#41800 = LINE ( 'NONE', #8081, #4801 ) ;
#41801 = CARTESIAN_POINT ( 'NONE',  ( -23.30963478160716562, -18.69084381296369912, 69.30844128244088154 ) ) ;
#41802 = ORIENTED_EDGE ( 'NONE', *, *, #8824, .T. ) ;
#41803 = CARTESIAN_POINT ( 'NONE',  ( -16.11159385650551457, -6.922745924619793101, 51.69366785382590024 ) ) ;
#41805 = ORIENTED_EDGE ( 'NONE', *, *, #36464, .F. ) ;
#41804 = EDGE_CURVE ( 'NONE', #9176, #45877, #6108, .T. ) ;
#41806 = VECTOR ( 'NONE', #6781, 1000.000000000000114 ) ;
#41807 = CARTESIAN_POINT ( 'NONE',  ( -16.05912236108952129, -21.67647341356571999, 58.47512757527289295 ) ) ;
#41808 = CARTESIAN_POINT ( 'NONE',  ( -12.32278866559117780, -19.67576434477648917, 61.41150688479135766 ) ) ;
#41809 = EDGE_CURVE ( 'NONE', #22777, #45931, #36663, .T. ) ;
#41810 = AXIS2_PLACEMENT_3D ( 'NONE', #27548, #11810, #18945 ) ;
#41811 = CARTESIAN_POINT ( 'NONE',  ( -15.17058439935471092, -21.43790227555238559, 68.64763166194532573 ) ) ;
#41812 = EDGE_CURVE ( 'NONE', #5311, #44029, #48563, .T. ) ;
#41813 =( BOUNDED_CURVE ( )  B_SPLINE_CURVE ( 3, ( #8027, #7775, #1095, #4315 ),
 .UNSPECIFIED., .F., .F. ) 
 B_SPLINE_CURVE_WITH_KNOTS ( ( 4, 4 ),
 ( 0.000000000000000000, 0.4074455897393656212 ),
 .UNSPECIFIED. ) 
 CURVE ( )  GEOMETRIC_REPRESENTATION_ITEM ( )  RATIONAL_B_SPLINE_CURVE ( ( 1.000000000000000000, 0.4567392136813327452, 0.3561768502900305999, 0.6983129098260936196 ) ) 
 REPRESENTATION_ITEM ( '' )  );
#41814 = ORIENTED_EDGE ( 'NONE', *, *, #24280, .F. ) ;
#41815 = CYLINDRICAL_SURFACE ( 'NONE', #30587, 5.249999999999998224 ) ;
#41816 = CARTESIAN_POINT ( 'NONE',  ( -10.66703363856100317, -12.79807828486586629, 64.26836111018113229 ) ) ;
#41817 = CARTESIAN_POINT ( 'NONE',  ( -22.81479297205375190, -19.95148388737573697, 72.74376929014212578 ) ) ;
#41818 = ORIENTED_EDGE ( 'NONE', *, *, #3191, .T. ) ;
#41819 = AXIS2_PLACEMENT_3D ( 'NONE', #15860, #26721, #19079 ) ;
#41820 = CARTESIAN_POINT ( 'NONE',  ( -10.61708496520324552, -12.96040230030987850, 71.30008833185628703 ) ) ;
#41821 = DIRECTION ( 'NONE',  ( 9.632611942272803284E-07, -3.816342176806251797E-07, -0.9999999999994633182 ) ) ;
#41822 = CARTESIAN_POINT ( 'NONE',  ( 22.62590614458706639, 1.890747609047893185, 50.53028072113869484 ) ) ;
#41823 = ORIENTED_EDGE ( 'NONE', *, *, #46096, .T. ) ;
#41824 = CARTESIAN_POINT ( 'NONE',  ( -22.72409385759798894, -9.359200813967568422, 50.49621490985803263 ) ) ;
#41825 =( BOUNDED_CURVE ( )  B_SPLINE_CURVE ( 3, ( #29338, #2980, #25634, #48284 ),
 .UNSPECIFIED., .F., .F. ) 
 B_SPLINE_CURVE_WITH_KNOTS ( ( 4, 4 ),
 ( 0.5000000000000000000, 0.9074455897393705062 ),
 .UNSPECIFIED. ) 
 CURVE ( )  GEOMETRIC_REPRESENTATION_ITEM ( )  RATIONAL_B_SPLINE_CURVE ( ( 1.000000000000006883, 0.4567392136813273606, 0.3561768502900237721, 0.6983129098261032786 ) ) 
 REPRESENTATION_ITEM ( '' )  );
#41826 = ORIENTED_EDGE ( 'NONE', *, *, #43935, .F. ) ;
#41827 = CARTESIAN_POINT ( 'NONE',  ( -10.48742572850251520, -13.50628733207679666, 71.36395466173868840 ) ) ;
#41828 = FACE_OUTER_BOUND ( 'NONE', #6897, .T. ) ;
#41829 = ORIENTED_EDGE ( 'NONE', *, *, #39131, .T. ) ;
#41830 = DIRECTION ( 'NONE',  ( -3.071710424422018668E-17, 6.404604876783312462E-16, 1.000000000000000000 ) ) ;
#41831 = LINE ( 'NONE', #42064, #37321 ) ;
#41832 = VECTOR ( 'NONE', #22684, 1000.000000000000000 ) ;
#41833 = DIRECTION ( 'NONE',  ( 3.071710424422018668E-17, -6.404604876783312462E-16, -1.000000000000000000 ) ) ;
#41834 = VERTEX_POINT ( 'NONE', #14490 ) ;
#41835 = CARTESIAN_POINT ( 'NONE',  ( -17.87628565292757088, -21.84483846147477237, 61.88095697920203264 ) ) ;
#41836 = PLANE ( 'NONE',  #20457 ) ;
#41837 = CARTESIAN_POINT ( 'NONE',  ( -11.42391642618174785, -11.20395052909733735, 57.40006283751519334 ) ) ;
#41838 = ORIENTED_EDGE ( 'NONE', *, *, #405, .F. ) ;
#41839 = CARTESIAN_POINT ( 'NONE',  ( -22.68646480449111635, -20.08284195570847430, 69.35913425646373298 ) ) ;
#41840 = CARTESIAN_POINT ( 'NONE',  ( -21.78913961794832588, -8.771810275399618106, 70.24637145832762997 ) ) ;
#41841 = AXIS2_PLACEMENT_3D ( 'NONE', #20610, #35604, #16882 ) ;
#41842 = ORIENTED_EDGE ( 'NONE', *, *, #11665, .F. ) ;
#41843 = VERTEX_POINT ( 'NONE', #3201 ) ;
#41844 = CARTESIAN_POINT ( 'NONE',  ( -21.77108044372514684, -13.02615771018284541, 49.52966884056655772 ) ) ;
#41845 = CARTESIAN_POINT ( 'NONE',  ( -10.48742572850251520, -13.50628733207679666, 71.36395466173868840 ) ) ;
#41846 = CARTESIAN_POINT ( 'NONE',  ( -10.78031428196279329, -11.32923628920978310, 53.49999999999994316 ) ) ;
#41847 = CARTESIAN_POINT ( 'NONE',  ( -20.72409385650551883, -6.426201560718812544, 50.50509628382439331 ) ) ;
#41848 = CARTESIAN_POINT ( 'NONE',  ( -20.38078961538757028, -7.970959937923086436, 70.50746246719650401 ) ) ;
#41849 = EDGE_CURVE ( 'NONE', #24654, #25105, #3663, .T. ) ;
#41850 = CARTESIAN_POINT ( 'NONE',  ( -12.10905746339987132, -9.588700880036457264, 57.28209702652397795 ) ) ;
#41851 = CARTESIAN_POINT ( 'NONE',  ( -17.59331746331979929, -7.761237803891376963, 63.55057029381061540 ) ) ;
#41852 = CARTESIAN_POINT ( 'NONE',  ( -9.975186738464962843, -14.94398050308648784, 74.97495774971199012 ) ) ;
#41853 = EDGE_LOOP ( 'NONE', ( #15460, #37984, #12802, #26069 ) ) ;
#41854 = DIRECTION ( 'NONE',  ( -0.9577883914167873991, -0.2682351919075509628, 0.1033986416233889233 ) ) ;
#41855 = CARTESIAN_POINT ( 'NONE',  ( -24.53780051168580911, -12.59584816521350348, 69.95738404390658616 ) ) ;
#41856 = CARTESIAN_POINT ( 'NONE',  ( -14.87949561415316424, -21.38794988972642841, 65.40596695917321313 ) ) ;
#41857 = EDGE_LOOP ( 'NONE', ( #17234, #13391, #9912, #4140 ) ) ;
#41858 = ORIENTED_EDGE ( 'NONE', *, *, #6993, .T. ) ;
#41859 = DIRECTION ( 'NONE',  ( -1.000000000000000000, 0.000000000000000000, 0.000000000000000000 ) ) ;
#41860 = CARTESIAN_POINT ( 'NONE',  ( -45.67409385541305511, -15.81020654474410847, 61.49999999999999289 ) ) ;
#41861 = EDGE_CURVE ( 'NONE', #11264, #27788, #37463, .T. ) ;
#41862 = CARTESIAN_POINT ( 'NONE',  ( -13.33790141638613314, -21.03862562311502060, 61.71635090507787424 ) ) ;
#41863 = CARTESIAN_POINT ( 'NONE',  ( -10.17814040529963826, -13.07751228953917533, 71.40839792250820039 ) ) ;
#41864 = ADVANCED_FACE ( 'NONE', ( #3693 ), #17959, .T. ) ;
#41865 = ORIENTED_EDGE ( 'NONE', *, *, #26076, .F. ) ;
#41866 = CARTESIAN_POINT ( 'NONE',  ( -10.52991701743181174, -16.02177613136639067, 67.97767831076122036 ) ) ;
#41867 =( BOUNDED_CURVE ( )  B_SPLINE_CURVE ( 3, ( #32881, #13680, #32655, #31935 ),
 .UNSPECIFIED., .F., .F. ) 
 B_SPLINE_CURVE_WITH_KNOTS ( ( 4, 4 ),
 ( 0.5000000000000000000, 0.9074455897393652881 ),
 .UNSPECIFIED. ) 
 CURVE ( )  GEOMETRIC_REPRESENTATION_ITEM ( )  RATIONAL_B_SPLINE_CURVE ( ( 1.000000000000018430, 0.4567392136813394066, 0.3561768502900201638, 0.6983129098260804080 ) ) 
 REPRESENTATION_ITEM ( '' )  );
#41868 = EDGE_CURVE ( 'NONE', #31985, #31794, #12013, .T. ) ;
#41869 = CARTESIAN_POINT ( 'NONE',  ( -19.89283007060495123, -10.81159512726058836, 52.02966884056656482 ) ) ;
#41870 = VERTEX_POINT ( 'NONE', #29546 ) ;
#41871 = CARTESIAN_POINT ( 'NONE',  ( -10.90187802848681109, -12.12302927398623353, 74.55840406006809928 ) ) ;
#41872 = ADVANCED_FACE ( 'NONE', ( #2713 ), #25378, .T. ) ;
#41873 = B_SPLINE_CURVE_WITH_KNOTS ( 'NONE', 1,
 ( #1021, #30102 ),
 .UNSPECIFIED., .F., .F.,
 ( 2, 2 ),
 ( 0.000000000000000000, 1.000000000000000000 ),
 .UNSPECIFIED. ) ;
#41874 = CARTESIAN_POINT ( 'NONE',  ( -14.37051197998799523, -8.445983692038035784, 74.34387349308116200 ) ) ;
#41875 = ORIENTED_EDGE ( 'NONE', *, *, #32677, .T. ) ;
#41877 = EDGE_CURVE ( 'NONE', #31526, #5342, #29307, .T. ) ;
#41876 = CARTESIAN_POINT ( 'NONE',  ( -17.39761409878557785, -7.809256622337199971, 67.02039592144427615 ) ) ;
#41878 = ORIENTED_EDGE ( 'NONE', *, *, #36980, .T. ) ;
#41879 = FACE_OUTER_BOUND ( 'NONE', #22112, .T. ) ;
#41880 = CARTESIAN_POINT ( 'NONE',  ( -20.49047903802489756, -8.516432955688220119, 63.61121494929229669 ) ) ;
#41881 = ORIENTED_EDGE ( 'NONE', *, *, #23888, .T. ) ;
#41882 = CARTESIAN_POINT ( 'NONE',  ( -13.54792730259346456, -8.920061342218058797, 57.25495614889487683 ) ) ;
#41883 = FACE_OUTER_BOUND ( 'NONE', #16393, .T. ) ;
#41884 = CARTESIAN_POINT ( 'NONE',  ( -18.78659385650551528, -9.302874398569244363, 51.68646062012417985 ) ) ;
#41885 = CARTESIAN_POINT ( 'NONE',  ( -21.40280876628366968, -21.10781420246748041, 69.25438953298345268 ) ) ;
#41886 = CARTESIAN_POINT ( 'NONE',  ( -11.32522400900782067, -11.27219014254736074, 60.96413645226084554 ) ) ;
#41887 = CARTESIAN_POINT ( 'NONE',  ( -15.92409385541305333, -14.80920654474410547, 48.99999999999997868 ) ) ;
#41888 = ORIENTED_EDGE ( 'NONE', *, *, #13703, .F. ) ;
#41889 = CARTESIAN_POINT ( 'NONE',  ( -16.67409385541329669, -6.859212275519744217, 50.50378509014024075 ) ) ;
#41890 = CARTESIAN_POINT ( 'NONE',  ( -23.44980260057078070, -18.46889688393208573, 72.76368236443251192 ) ) ;
#41891 = CARTESIAN_POINT ( 'NONE',  ( -24.45577199812615632, -12.20047074031916168, 54.27966884056650088 ) ) ;
#41892 = CARTESIAN_POINT ( 'NONE',  ( -24.18825283819140992, -13.00726010212983574, 63.05937419120780163 ) ) ;
#41893 = ORIENTED_EDGE ( 'NONE', *, *, #20662, .T. ) ;
#41894 = VERTEX_POINT ( 'NONE', #11084 ) ;
#41895 = LINE ( 'NONE', #8172, #23581 ) ;
#41896 = CARTESIAN_POINT ( 'NONE',  ( -14.53996353315453405, -7.939311612974331744, 60.43341030124493329 ) ) ;
#41897 = ORIENTED_EDGE ( 'NONE', *, *, #22694, .T. ) ;
#41898 = CARTESIAN_POINT ( 'NONE',  ( -15.34465393633500696, -21.54586957516256263, 68.86120835375241711 ) ) ;
#41899 = CARTESIAN_POINT ( 'NONE',  ( -21.93659385759799108, -8.995762431863214559, 51.38120296130585274 ) ) ;
#41900 = LINE ( 'NONE', #19244, #27385 ) ;
#41901 = ADVANCED_FACE ( 'NONE', ( #44344 ), #25855, .T. ) ;
#41902 = CARTESIAN_POINT ( 'NONE',  ( -14.35241195940507808, -8.021096776717739019, 67.44630344931481147 ) ) ;
#41903 = CARTESIAN_POINT ( 'NONE',  ( -24.28619334359350290, -16.42731978468327014, 59.13804568661029037 ) ) ;
#41904 = CARTESIAN_POINT ( 'NONE',  ( -16.39155704513022016, -21.78318439201321866, 61.75568132354042916 ) ) ;
#41905 = VERTEX_POINT ( 'NONE', #9 ) ;
#41906 = CARTESIAN_POINT ( 'NONE',  ( -20.59270190486383356, -18.27842527154038521, 49.52966884056656482 ) ) ;
#41907 = CARTESIAN_POINT ( 'NONE',  ( -14.44842434502374573, -8.417926551829491899, 67.25975083404114230 ) ) ;
#41908 = CARTESIAN_POINT ( 'NONE',  ( -10.51276550655336273, -13.39960300793130621, 71.41648339266447465 ) ) ;
#41909 = CYLINDRICAL_SURFACE ( 'NONE', #20898, 4.686499999999997002 ) ;
#41910 = CARTESIAN_POINT ( 'NONE',  ( -19.98813031515369332, -21.37641424997302053, 72.70478737316020101 ) ) ;
#41911 = FACE_BOUND ( 'NONE', #38767, .T. ) ;
#41912 = ADVANCED_FACE ( 'NONE', ( #48251 ), #6898, .T. ) ;
#41913 = ORIENTED_EDGE ( 'NONE', *, *, #4931, .F. ) ;
#41914 = ORIENTED_EDGE ( 'NONE', *, *, #37911, .F. ) ;
#41915 =( NAMED_UNIT ( * ) PLANE_ANGLE_UNIT ( ) SI_UNIT ( $, .RADIAN. ) );
#41916 = ORIENTED_EDGE ( 'NONE', *, *, #2306, .F. ) ;
#41917 = CARTESIAN_POINT ( 'NONE',  ( -11.56806251476610115, -18.73522173559940995, 65.03234934376791898 ) ) ;
#41918 = CARTESIAN_POINT ( 'NONE',  ( -10.02107422201081732, -13.96720754792729480, 57.56169656168945181 ) ) ;
#41919 = B_SPLINE_CURVE_WITH_KNOTS ( 'NONE', 3,
 ( #41615, #15239, #11086, #37656, #34448, #37909, #30305, #41862, #14732, #22174 ),
 .UNSPECIFIED., .F., .F.,
 ( 4, 2, 2, 2, 4 ),
 ( 0.1272669073658578009, 0.2522669073463363332, 0.3772669073268148932, 0.5022669073072933976, 0.6272669072877719021 ),
 .UNSPECIFIED. ) ;
#41920 = EDGE_CURVE ( 'NONE', #30823, #32996, #16701, .T. ) ;
#41921 = CARTESIAN_POINT ( 'NONE',  ( -13.41559485503361948, -8.529420403834853559, 57.08472365561223683 ) ) ;
#41922 = CARTESIAN_POINT ( 'NONE',  ( -16.16379449968008331, -22.15191876840708929, 58.47080954035841671 ) ) ;
#41923 = AXIS2_PLACEMENT_3D ( 'NONE', #5789, #5552, #2075 ) ;
#41924 = ORIENTED_EDGE ( 'NONE', *, *, #28481, .F. ) ;
#41925 = EDGE_CURVE ( 'NONE', #15450, #18903, #21914, .T. ) ;
#41926 = FACE_OUTER_BOUND ( 'NONE', #30923, .T. ) ;
#41927 = EDGE_CURVE ( 'NONE', #40396, #1942, #15729, .T. ) ;
#41928 = CARTESIAN_POINT ( 'NONE',  ( -17.61671342162341958, -7.361684265168443098, 63.65082775983518815 ) ) ;
#41929 = VERTEX_POINT ( 'NONE', #42343 ) ;
#41930 = DIRECTION ( 'NONE',  ( -3.071710424422018668E-17, 6.404604876783312462E-16, 1.000000000000000000 ) ) ;
#41931 = CARTESIAN_POINT ( 'NONE',  ( -15.38465892218781050, -7.643789270862604290, 74.22985656858331538 ) ) ;
#41932 = VERTEX_POINT ( 'NONE', #41613 ) ;
#41933 = CARTESIAN_POINT ( 'NONE',  ( -22.92560359444879836, -19.23055950467793096, 62.49839992038752712 ) ) ;
#41934 = CARTESIAN_POINT ( 'NONE',  ( -22.49057859776916857, -20.27125474133809391, 65.89760026996282249 ) ) ;
#41935 = CARTESIAN_POINT ( 'NONE',  ( -18.30534385541304232, -7.595227055684743434, 51.75156210489596020 ) ) ;
#41936 = ORIENTED_EDGE ( 'NONE', *, *, #47454, .T. ) ;
#41937 = CARTESIAN_POINT ( 'NONE',  ( -24.47217469393258327, -14.64471774706559515, 62.86296487297660462 ) ) ;
#41938 = CARTESIAN_POINT ( 'NONE',  ( -36.42409385541304800, -8.109206544743658540, 50.50000000000030553 ) ) ;
#41939 =( BOUNDED_SURFACE ( )  B_SPLINE_SURFACE ( 3, 1, ( 
 ( #3978, #42314 ),
 ( #30989, #43033 ),
 ( #35395, #9311 ),
 ( #24329, #9072 ),
 ( #42797, #38851 ),
 ( #1673, #24581 ),
 ( #24086, #39088 ) ),
 .UNSPECIFIED., .T., .F., .F. ) 
 B_SPLINE_SURFACE_WITH_KNOTS ( ( 4, 3, 4 ),
 ( 2, 2 ),
 ( 0.000000000000000000, 0.5000000000000000000, 1.000000000000000000 ),
 ( 0.000000000000000000, 1.000000000000000000 ),
 .UNSPECIFIED. ) 
 GEOMETRIC_REPRESENTATION_ITEM ( )  RATIONAL_B_SPLINE_SURFACE ( (
 ( 1.000000000000000000, 1.000000000000000000),
 ( 0.3333333333333335369, 0.3333333333333330373),
 ( 0.3333333333333335369, 0.3333333333333330373),
 ( 1.000000000000000000, 1.000000000000000000),
 ( 0.3333333333333333703, 0.3333333333333333703),
 ( 0.3333333333333333703, 0.3333333333333333703),
 ( 1.000000000000000000, 1.000000000000000000) ) ) 
 REPRESENTATION_ITEM ( '' )  SURFACE ( )  );
#41940 = EDGE_CURVE ( 'NONE', #2243, #21441, #32585, .T. ) ;
#41941 = CARTESIAN_POINT ( 'NONE',  ( -14.52849927865251267, -21.67364703532615877, 58.30584490887105886 ) ) ;
#41942 = FACE_OUTER_BOUND ( 'NONE', #17286, .T. ) ;
#41943 = ORIENTED_EDGE ( 'NONE', *, *, #35666, .F. ) ;
#41944 = LINE ( 'NONE', #8220, #14799 ) ;
#41945 = CARTESIAN_POINT ( 'NONE',  ( -16.06904265174829405, -7.890656434512189676, 63.82011029958098192 ) ) ;
#41946 = EDGE_CURVE ( 'NONE', #44255, #3166, #39654, .T. ) ;
#41947 = DIRECTION ( 'NONE',  ( -6.816999857788696862E-06, -9.113320819891793432E-06, -0.9999999999352379154 ) ) ;
#41948 = FACE_OUTER_BOUND ( 'NONE', #47964, .T. ) ;
#41949 = DIRECTION ( 'NONE',  ( 0.9687793358424821033, -0.2479245821708677133, 0.000000000000000000 ) ) ;
#41950 = EDGE_CURVE ( 'NONE', #23509, #13312, #7893, .T. ) ;
#41951 = EDGE_CURVE ( 'NONE', #29468, #4941, #38639, .T. ) ;
#41952 = CARTESIAN_POINT ( 'NONE',  ( -18.86784385650552309, -6.428312510596451368, 51.20221977374900035 ) ) ;
#41953 = ORIENTED_EDGE ( 'NONE', *, *, #5297, .F. ) ;
#41954 = FACE_BOUND ( 'NONE', #48670, .T. ) ;
#41955 = CARTESIAN_POINT ( 'NONE',  ( -11.03619655160677304, -10.97525948075760560, 60.80168914678925063 ) ) ;
#41956 = ORIENTED_EDGE ( 'NONE', *, *, #9154, .T. ) ;
#41957 = CARTESIAN_POINT ( 'NONE',  ( -23.23616409499838653, -18.79948708312782557, 65.82389430043846801 ) ) ;
#41958 = CARTESIAN_POINT ( 'NONE',  ( -12.79553473267226771, -20.06053405000708878, 68.52760710243867948 ) ) ;
#41959 = DIRECTION ( 'NONE',  ( 1.000000000000000000, -4.164305804376849172E-17, 1.614929280266638808E-16 ) ) ;
#41960 =( BOUNDED_SURFACE ( )  B_SPLINE_SURFACE ( 3, 1, ( 
 ( #32733, #2697 ),
 ( #33438, #48479 ),
 ( #47757, #6403 ),
 ( #11069, #10347 ),
 ( #21433, #40854 ),
 ( #30039, #44814 ),
 ( #37138, #14471 ) ),
 .UNSPECIFIED., .T., .F., .F. ) 
 B_SPLINE_SURFACE_WITH_KNOTS ( ( 4, 3, 4 ),
 ( 2, 2 ),
 ( 0.000000000000000000, 0.5000000000000000000, 1.000000000000000000 ),
 ( 0.000000000000000000, 1.000000000000000000 ),
 .UNSPECIFIED. ) 
 GEOMETRIC_REPRESENTATION_ITEM ( )  RATIONAL_B_SPLINE_SURFACE ( (
 ( 1.000000000000000000, 1.000000000000000000),
 ( 0.3333333333333335369, 0.3333333333333330373),
 ( 0.3333333333333335369, 0.3333333333333330373),
 ( 1.000000000000000000, 1.000000000000000000),
 ( 0.3333333333333333703, 0.3333333333333333703),
 ( 0.3333333333333333703, 0.3333333333333333703),
 ( 1.000000000000000000, 1.000000000000000000) ) ) 
 REPRESENTATION_ITEM ( '' )  SURFACE ( )  );
#41961 = ORIENTED_EDGE ( 'NONE', *, *, #15106, .F. ) ;
#41962 =( BOUNDED_CURVE ( )  B_SPLINE_CURVE ( 3, ( #2302, #5771, #20778, #17310 ),
 .UNSPECIFIED., .F., .F. ) 
 B_SPLINE_CURVE_WITH_KNOTS ( ( 4, 4 ),
 ( 0.9074455897393700621, 1.000000000000000000 ),
 .UNSPECIFIED. ) 
 CURVE ( )  GEOMETRIC_REPRESENTATION_ITEM ( )  RATIONAL_B_SPLINE_CURVE ( ( 0.6983129098261124934, 0.7760317562607149666, 0.8765941196520108392, 1.000000000000000000 ) ) 
 REPRESENTATION_ITEM ( '' )  );
#41963 = CARTESIAN_POINT ( 'NONE',  ( -14.78754745127378456, -8.270772244812135909, 60.61996282000563241 ) ) ;
#41964 = CARTESIAN_POINT ( 'NONE',  ( -24.42401755266412522, -14.76532053153747448, 59.52834928196978126 ) ) ;
#41965 = CARTESIAN_POINT ( 'NONE',  ( -24.02253934063158880, -11.35034036425029136, 66.61552819682387394 ) ) ;
#41966 = B_SPLINE_CURVE_WITH_KNOTS ( 'NONE', 1,
 ( #31860, #17787 ),
 .UNSPECIFIED., .F., .F.,
 ( 2, 2 ),
 ( 0.000000000000000000, 1.000000000000000000 ),
 .UNSPECIFIED. ) ;
#41967 = VERTEX_POINT ( 'NONE', #15479 ) ;
#41968 = AXIS2_PLACEMENT_3D ( 'NONE', #1282, #8700, #23728 ) ;
#41969 = CARTESIAN_POINT ( 'NONE',  ( -43.06159385541306506, -14.90920654474410512, 57.89999999999999147 ) ) ;
#41970 = DIRECTION ( 'NONE',  ( 0.000000000000000000, 0.000000000000000000, -1.000000000000000000 ) ) ;
#41971 = CARTESIAN_POINT ( 'NONE',  ( -10.00731251637046881, -14.10555026099538978, 61.10316585833331260 ) ) ;
#41972 = DIRECTION ( 'NONE',  ( -0.9986807914369958405, 0.05134858142905002198, -1.286972153835537669E-09 ) ) ;
#41973 = CARTESIAN_POINT ( 'NONE',  ( -23.16941533403626607, -18.80811654971253688, 62.46292810888792957 ) ) ;
#41974 =( BOUNDED_CURVE ( )  B_SPLINE_CURVE ( 3, ( #7912, #34218, #505, #15748 ),
 .UNSPECIFIED., .F., .F. ) 
 B_SPLINE_CURVE_WITH_KNOTS ( ( 4, 4 ),
 ( 0.000000000000000000, 0.4074455897393670645 ),
 .UNSPECIFIED. ) 
 CURVE ( )  GEOMETRIC_REPRESENTATION_ITEM ( )  RATIONAL_B_SPLINE_CURVE ( ( 1.000000000000000000, 0.4567392136813321346, 0.3561768502900303779, 0.6983129098260947298 ) ) 
 REPRESENTATION_ITEM ( '' )  );
#41975 = ORIENTED_EDGE ( 'NONE', *, *, #45089, .T. ) ;
#41976 = ORIENTED_EDGE ( 'NONE', *, *, #31358, .T. ) ;
#41977 = CARTESIAN_POINT ( 'NONE',  ( -22.41159385541304161, -8.990409506049200417, 49.61344411288074951 ) ) ;
#41978 = ADVANCED_FACE ( 'NONE', ( #18959 ), #261, .T. ) ;
#41979 = CARTESIAN_POINT ( 'NONE',  ( -21.06702863216100496, -20.84540773593990792, 65.86981821684420879 ) ) ;
#41980 = CARTESIAN_POINT ( 'NONE',  ( -20.38154718419116662, -8.406214666052791884, 70.66588945595221105 ) ) ;
#41981 = CARTESIAN_POINT ( 'NONE',  ( -17.42409385541299471, -14.80920654474435594, 52.02966884056656482 ) ) ;
#41982 = CARTESIAN_POINT ( 'NONE',  ( -17.84905175390062837, -22.24782703323402444, 58.51898120184483076 ) ) ;
#41983 = CARTESIAN_POINT ( 'NONE',  ( -20.54394416162392289, -8.483752705004535599, 59.72636470710568091 ) ) ;
#41984 = EDGE_CURVE ( 'NONE', #31166, #45033, #25668, .T. ) ;
#41985 = CARTESIAN_POINT ( 'NONE',  ( -9.976559278833523337, -14.59036342035520306, 67.97144843379662404 ) ) ;
#41986 = CARTESIAN_POINT ( 'NONE',  ( -24.78881009142557090, -15.93819564886128148, 66.17669525438618905 ) ) ;
#41987 = VERTEX_POINT ( 'NONE', #30789 ) ;
#41988 = CARTESIAN_POINT ( 'NONE',  ( -24.05420634179087358, -17.20676946999824608, 69.69867738674849988 ) ) ;
#41989 = AXIS2_PLACEMENT_3D ( 'NONE', #40368, #17936, #47753 ) ;
#41990 = ORIENTED_EDGE ( 'NONE', *, *, #32703, .F. ) ;
#41991 = CARTESIAN_POINT ( 'NONE',  ( -22.22371030936713510, -9.111184089457765367, 59.90666523727240644 ) ) ;
#41992 = DIRECTION ( 'NONE',  ( -0.9848822020395749943, 0.1732254256905498002, 7.367703375004543066E-08 ) ) ;
#41993 = DIRECTION ( 'NONE',  ( -3.549360974554993999E-17, 6.371834667797928663E-18, 1.000000000000000000 ) ) ;
#41994 = AXIS2_PLACEMENT_3D ( 'NONE', #13148, #28195, #9245 ) ;
#41995 = EDGE_LOOP ( 'NONE', ( #4456, #29290 ) ) ;
#41996 = CARTESIAN_POINT ( 'NONE',  ( -10.69985271022639317, -16.93744915505940085, 61.57231810286263141 ) ) ;
#41997 = CARTESIAN_POINT ( 'NONE',  ( -14.60479643987598841, -7.913168514039711887, 60.50491717424539218 ) ) ;
#41998 = CARTESIAN_POINT ( 'NONE',  ( -14.74690658000796439, -21.27702444416618732, 58.16617884968206198 ) ) ;
#41999 = CARTESIAN_POINT ( 'NONE',  ( -24.49036105318029755, -17.16975618249231061, 73.00523289078640232 ) ) ;
#42000 = ORIENTED_EDGE ( 'NONE', *, *, #36181, .T. ) ;
#42001 = CARTESIAN_POINT ( 'NONE',  ( -45.92409385541306222, -14.80920654474410902, 73.00000000000001421 ) ) ;
#42002 = CARTESIAN_POINT ( 'NONE',  ( -17.78619188034219079, -22.25052443322864448, 58.52740643916145302 ) ) ;
#42003 = CARTESIAN_POINT ( 'NONE',  ( -17.42409385541299471, -14.80920654474434883, 62.02966884056656482 ) ) ;
#42004 = FACE_BOUND ( 'NONE', #11051, .T. ) ;
#42005 = PRODUCT_CONTEXT ( 'NONE', #4536, 'mechanical' ) ;
#42006 = ADVANCED_FACE ( 'NONE', ( #1203 ), #34937, .T. ) ;
#42007 = EDGE_CURVE ( 'NONE', #27678, #22721, #45806, .T. ) ;
#42008 = LINE ( 'NONE', #38283, #32886 ) ;
#42009 = CARTESIAN_POINT ( 'NONE',  ( -19.11145865927415954, -7.964113456900453691, 63.43089235103782642 ) ) ;
#42010 = DIRECTION ( 'NONE',  ( -0.000000000000000000, -1.000000000000000000, -0.000000000000000000 ) ) ;
#42011 = FACE_OUTER_BOUND ( 'NONE', #32833, .T. ) ;
#42012 = EDGE_LOOP ( 'NONE', ( #17977, #28004, #35402, #28048, #38075 ) ) ;
#42013 = CARTESIAN_POINT ( 'NONE',  ( -12.08002995027803372, -10.28786569443740717, 67.49896886176594535 ) ) ;
#42014 = ORIENTED_EDGE ( 'NONE', *, *, #1912, .T. ) ;
#42015 = CARTESIAN_POINT ( 'NONE',  ( -11.45751978572037011, -19.27057081285444085, 71.87181161472111057 ) ) ;
#42016 = CARTESIAN_POINT ( 'NONE',  ( -22.96794631393402142, -10.53327243508824473, 63.14356316969981009 ) ) ;
#42017 = ORIENTED_EDGE ( 'NONE', *, *, #37351, .F. ) ;
#42018 = ADVANCED_FACE ( 'NONE', ( #4671 ), #15974, .T. ) ;
#42019 = ADVANCED_FACE ( 'NONE', ( #12058 ), #34702, .T. ) ;
#42020 = CARTESIAN_POINT ( 'NONE',  ( -12.74662852849665207, -9.010439419175657605, 70.97208472523765010 ) ) ;
#42021 = ORIENTED_EDGE ( 'NONE', *, *, #13321, .F. ) ;
#42022 = ORIENTED_EDGE ( 'NONE', *, *, #41319, .F. ) ;
#42023 = ORIENTED_EDGE ( 'NONE', *, *, #47009, .T. ) ;
#42024 = DIRECTION ( 'NONE',  ( -1.224646799147353207E-16, -1.000000000000000000, 1.912410701131276611E-32 ) ) ;
#42025 = DIRECTION ( 'NONE',  ( 0.8394943004421987487, -0.3114503813636534946, 0.4452504682462423702 ) ) ;
#42026 = CARTESIAN_POINT ( 'NONE',  ( -24.16171209271585596, -12.91020206353950250, 66.60246698658390585 ) ) ;
#42027 = CARTESIAN_POINT ( 'NONE',  ( -11.81148223110008821, -9.909859460634582007, 64.18947707955818771 ) ) ;
#42028 = CARTESIAN_POINT ( 'NONE',  ( -46.29409385541305966, -14.20920654474410760, 71.05212771298751306 ) ) ;
#42029 = ORIENTED_EDGE ( 'NONE', *, *, #12473, .F. ) ;
#42030 = ORIENTED_EDGE ( 'NONE', *, *, #26174, .T. ) ;
#42031 = VECTOR ( 'NONE', #4293, 1000.000000000000114 ) ;
#42032 = CARTESIAN_POINT ( 'NONE',  ( -19.50843993236927432, -21.96177808838975665, 62.11008241541560437 ) ) ;
#42033 = ADVANCED_FACE ( 'NONE', ( #23640 ), #8364, .F. ) ;
#42034 = VECTOR ( 'NONE', #32791, 1000.000000000000114 ) ;
#42035 = CARTESIAN_POINT ( 'NONE',  ( -10.40687472791218049, -14.09964931664121579, 64.80292589203708076 ) ) ;
#42036 = DIRECTION ( 'NONE',  ( -0.9687793358424819923, 0.2479245821708680464, 0.000000000000000000 ) ) ;
#42037 = CARTESIAN_POINT ( 'NONE',  ( -19.67335841558337961, -21.43805762741428111, 65.75020853001484511 ) ) ;
#42038 = ORIENTED_EDGE ( 'NONE', *, *, #16823, .T. ) ;
#42039 = CARTESIAN_POINT ( 'NONE',  ( -14.19909385650551847, -8.114302828567740988, 52.18300498402516041 ) ) ;
#42040 = ORIENTED_EDGE ( 'NONE', *, *, #45982, .F. ) ;
#42041 = CARTESIAN_POINT ( 'NONE',  ( -21.57995947450667984, -9.113990939708573435, 70.14604673427196246 ) ) ;
#42042 = DIRECTION ( 'NONE',  ( 2.181982678098338148E-16, 0.000000000000000000, -1.000000000000000000 ) ) ;
#42043 = DIRECTION ( 'NONE',  ( -2.866981220435666553E-17, 1.000000000000000000, 1.190614954331866791E-16 ) ) ;
#42044 =( BOUNDED_CURVE ( )  B_SPLINE_CURVE ( 3, ( #12641, #47361, #31843, #43170 ),
 .UNSPECIFIED., .F., .F. ) 
 B_SPLINE_CURVE_WITH_KNOTS ( ( 4, 4 ),
 ( 0.000000000000000000, 0.4074455897393667314 ),
 .UNSPECIFIED. ) 
 CURVE ( )  GEOMETRIC_REPRESENTATION_ITEM ( )  RATIONAL_B_SPLINE_CURVE ( ( 1.000000000000000000, 0.4567392136813263059, 0.3561768502900282130, 0.6983129098261057210 ) ) 
 REPRESENTATION_ITEM ( '' )  );
#42045 = B_SPLINE_CURVE_WITH_KNOTS ( 'NONE', 3,
 ( #28122, #1057, #45884, #27880, #12139, #23959, #38471, #4755, #16054, #15819 ),
 .UNSPECIFIED., .F., .F.,
 ( 4, 2, 2, 2, 4 ),
 ( 0.000000000000000000, 0.2500000000000000000, 0.5000000000000000000, 0.7500000000000000000, 1.000000000000000000 ),
 .UNSPECIFIED. ) ;
#42046 = EDGE_LOOP ( 'NONE', ( #24051, #25859 ) ) ;
#42047 = DIRECTION ( 'NONE',  ( -0.2196488028684550897, -0.9755790093059856227, 7.835600157697874713E-08 ) ) ;
#42048 = B_SPLINE_CURVE_WITH_KNOTS ( 'NONE', 1,
 ( #19687, #45077 ),
 .UNSPECIFIED., .F., .F.,
 ( 2, 2 ),
 ( 0.000000000000000000, 1.000000000000000000 ),
 .UNSPECIFIED. ) ;
#42049 = CARTESIAN_POINT ( 'NONE',  ( -11.83425018566923370, -19.11833757169930692, 68.37256453262955347 ) ) ;
#42050 = CARTESIAN_POINT ( 'NONE',  ( -12.55788482626217650, -9.703832430577184809, 57.50424130074089391 ) ) ;
#42051 = VERTEX_POINT ( 'NONE', #7649 ) ;
#42052 = LINE ( 'NONE', #31206, #1373 ) ;
#42053 = CARTESIAN_POINT ( 'NONE',  ( -17.19167086870822203, -7.760035283349824731, 66.90551000485606892 ) ) ;
#42054 = CARTESIAN_POINT ( 'NONE',  ( -6.424093855413055110, -6.859206544744110623, 47.99999999999998579 ) ) ;
#42055 = VERTEX_POINT ( 'NONE', #16209 ) ;
#42056 = CARTESIAN_POINT ( 'NONE',  ( -10.00747133761319141, -14.10395761772617362, 60.96175355949325336 ) ) ;
#42057 = ORIENTED_EDGE ( 'NONE', *, *, #19176, .T. ) ;
#42058 = CIRCLE ( 'NONE', #28698, 1.900000000000000133 ) ;
#42059 = CARTESIAN_POINT ( 'NONE',  ( -23.45029294355628480, -11.15024590387849557, 73.66193277021260144 ) ) ;
#42060 = CARTESIAN_POINT ( 'NONE',  ( -22.02664077354800654, -9.468686367811812943, 59.72730992479275614 ) ) ;
#42061 = VERTEX_POINT ( 'NONE', #31251 ) ;
#42062 = EDGE_CURVE ( 'NONE', #38050, #48382, #23326, .T. ) ;
#42063 = CARTESIAN_POINT ( 'NONE',  ( -16.32745258320347759, -21.77369344365219561, 61.77040269689842944 ) ) ;
#42064 = CARTESIAN_POINT ( 'NONE',  ( -50.42609385541305755, -14.90920654474413887, 60.91764705882351905 ) ) ;
#42065 = CIRCLE ( 'NONE', #26343, 4.686499999999998778 ) ;
#42066 = DIRECTION ( 'NONE',  ( 4.115385489419892128E-17, 0.9999954153791273948, 0.003028072113818697231 ) ) ;
#42067 = VERTEX_POINT ( 'NONE', #46995 ) ;
#42068 = CARTESIAN_POINT ( 'NONE',  ( -22.12470610600313137, -9.029191726191170275, 63.36966517759014295 ) ) ;
#42069 = UNCERTAINTY_MEASURE_WITH_UNIT (LENGTH_MEASURE( 1.000000000000000082E-05 ), #14481, 'distance_accuracy_value', 'NONE');
#42070 = DIRECTION ( 'NONE',  ( 0.9789991564298999860, 0.2038642972899921690, -4.410747590293462207E-08 ) ) ;
#42071 = CARTESIAN_POINT ( 'NONE',  ( -10.95381465013825206, -17.48043978162002077, 68.39721944380028162 ) ) ;
#42072 = VERTEX_POINT ( 'NONE', #39850 ) ;
#42073 = DIRECTION ( 'NONE',  ( -3.071710424422018668E-17, 6.404604876783312462E-16, 1.000000000000000000 ) ) ;
#42074 = EDGE_CURVE ( 'NONE', #3341, #47047, #34316, .T. ) ;
#42075 = CARTESIAN_POINT ( 'NONE',  ( -23.32804039107871574, -19.35299860258280447, 59.08399415320680959 ) ) ;
#42076 = VERTEX_POINT ( 'NONE', #13493 ) ;
#42077 = ORIENTED_EDGE ( 'NONE', *, *, #43252, .F. ) ;
#42078 = ADVANCED_FACE ( 'NONE', ( #28538 ), #47247, .T. ) ;
#42079 = CARTESIAN_POINT ( 'NONE',  ( -24.84680101036319400, -14.17012173819833798, 69.81308644732062874 ) ) ;
#42080 = CARTESIAN_POINT ( 'NONE',  ( -16.06904075904983031, -7.890656793283918446, 63.97011029956861705 ) ) ;
#42081 = DIRECTION ( 'NONE',  ( 0.000000000000000000, 1.000000000000000000, 5.551115123125785858E-15 ) ) ;
#42082 = CARTESIAN_POINT ( 'NONE',  ( -22.18659385650551741, -9.302874398569244363, 51.68646062012417985 ) ) ;
#42083 = EDGE_CURVE ( 'NONE', #12097, #13748, #13869, .T. ) ;
#42084 = CARTESIAN_POINT ( 'NONE',  ( -24.82750207115152463, -13.97654542584719373, 73.30766806548945169 ) ) ;
#42085 = LINE ( 'NONE', #32215, #13350 ) ;
#42086 = CARTESIAN_POINT ( 'NONE',  ( -10.76785811675247118, -12.48515291162924434, 57.61385273545094066 ) ) ;
#42087 = CARTESIAN_POINT ( 'NONE',  ( -10.56255612388957665, -16.44405857821975658, 71.65570096763067909 ) ) ;
#42088 = ORIENTED_EDGE ( 'NONE', *, *, #39607, .F. ) ;
#42089 = ORIENTED_EDGE ( 'NONE', *, *, #19746, .T. ) ;
#42090 = CARTESIAN_POINT ( 'NONE',  ( -13.88293403466071396, -20.90532716339074781, 68.60625136993937190 ) ) ;
#42091 = EDGE_CURVE ( 'NONE', #13885, #4171, #45513, .T. ) ;
#42092 = DIRECTION ( 'NONE',  ( -3.071710424422018668E-17, 6.404604876783312462E-16, 1.000000000000000000 ) ) ;
#42093 = CARTESIAN_POINT ( 'NONE',  ( -20.88270717056239789, -21.40782548341276481, 58.82970473467946704 ) ) ;
#42094 = B_SPLINE_CURVE_WITH_KNOTS ( 'NONE', 1,
 ( #43572, #9835 ),
 .UNSPECIFIED., .F., .F.,
 ( 2, 2 ),
 ( 0.000000000000000000, 1.000000000000000000 ),
 .UNSPECIFIED. ) ;
#42095 =( BOUNDED_CURVE ( )  B_SPLINE_CURVE ( 3, ( #5749, #28626, #17528, #13817 ),
 .UNSPECIFIED., .F., .F. ) 
 B_SPLINE_CURVE_WITH_KNOTS ( ( 4, 4 ),
 ( 0.9074455897393666204, 1.000000000000000000 ),
 .UNSPECIFIED. ) 
 CURVE ( )  GEOMETRIC_REPRESENTATION_ITEM ( )  RATIONAL_B_SPLINE_CURVE ( ( 0.6983129098261068313, 0.7760317562607100816, 0.8765941196520078416, 1.000000000000000000 ) ) 
 REPRESENTATION_ITEM ( '' )  );
#42096 = ORIENTED_EDGE ( 'NONE', *, *, #15656, .F. ) ;
#42097 = VECTOR ( 'NONE', #28693, 1000.000000000000000 ) ;
#42098 = ORIENTED_EDGE ( 'NONE', *, *, #41390, .T. ) ;
#42099 = DIRECTION ( 'NONE',  ( 0.9999889394985579383, 0.004703284017506803583, -7.734398264755851970E-09 ) ) ;
#42100 = VECTOR ( 'NONE', #14769, 1000.000000000000227 ) ;
#42101 = CARTESIAN_POINT ( 'NONE',  ( -23.78676244964941233, -10.93361294341921131, 73.54688584860882372 ) ) ;
#42102 = DIRECTION ( 'NONE',  ( 0.4599824152910791941, 0.8879280250239793837, 2.250728352126283350E-08 ) ) ;
#42103 = CARTESIAN_POINT ( 'NONE',  ( -9.424093855413055110, -25.10920654474410441, 54.99999999999997868 ) ) ;
#42104 = ORIENTED_EDGE ( 'NONE', *, *, #10977, .F. ) ;
#42105 =( BOUNDED_CURVE ( )  B_SPLINE_CURVE ( 3, ( #3100, #18108, #48164, #14395 ),
 .UNSPECIFIED., .F., .F. ) 
 B_SPLINE_CURVE_WITH_KNOTS ( ( 4, 4 ),
 ( 0.9074455897393750581, 1.000000000000000000 ),
 .UNSPECIFIED. ) 
 CURVE ( )  GEOMETRIC_REPRESENTATION_ITEM ( )  RATIONAL_B_SPLINE_CURVE ( ( 0.6983129098261150469, 0.7760317562607171871, 0.8765941196520121714, 1.000000000000000000 ) ) 
 REPRESENTATION_ITEM ( '' )  );
#42106 = FACE_OUTER_BOUND ( 'NONE', #26557, .T. ) ;
#42107 = CARTESIAN_POINT ( 'NONE',  ( -24.80746943141735983, -15.80390768895026987, 69.57661537956182940 ) ) ;
#42108 = ORIENTED_EDGE ( 'NONE', *, *, #41738, .T. ) ;
#42109 = CARTESIAN_POINT ( 'NONE',  ( -12.93275540070710505, -20.17844446062794717, 71.87941766543936239 ) ) ;
#42110 = CARTESIAN_POINT ( 'NONE',  ( -22.20320178312271153, -19.92390373660361291, 65.70421731406698029 ) ) ;
#42111 = EDGE_CURVE ( 'NONE', #36681, #30955, #9341, .T. ) ;
#42112 = ORIENTED_EDGE ( 'NONE', *, *, #12516, .F. ) ;
#42113 = CARTESIAN_POINT ( 'NONE',  ( -24.72409385541305582, -14.90920654474414775, 61.02352941176469869 ) ) ;
#42114 = VERTEX_POINT ( 'NONE', #20166 ) ;
#42115 = CARTESIAN_POINT ( 'NONE',  ( -17.26457240846633923, -7.760713630915982542, 70.50507891880883449 ) ) ;
#42116 = CARTESIAN_POINT ( 'NONE',  ( -21.97169192525862869, -15.94174089086207147, 49.52966884056655772 ) ) ;
#42117 = ORIENTED_EDGE ( 'NONE', *, *, #40824, .F. ) ;
#42118 = CARTESIAN_POINT ( 'NONE',  ( -13.35685073114381716, -8.567315923767541364, 57.01321801328607108 ) ) ;
#42119 = EDGE_CURVE ( 'NONE', #34596, #30663, #43836, .T. ) ;
#42120 = DIRECTION ( 'NONE',  ( -3.071710424422018668E-17, 6.404604876783312462E-16, 1.000000000000000000 ) ) ;
#42121 = CARTESIAN_POINT ( 'NONE',  ( -18.33659385650551243, -6.915538690918075382, 49.31353937987644542 ) ) ;
#42122 = CARTESIAN_POINT ( 'NONE',  ( -10.33431758219403207, -12.52035302217920254, 60.98348881056122650 ) ) ;
#42123 = CARTESIAN_POINT ( 'NONE',  ( -19.10460565471617755, -7.550450307296652674, 63.54433857513910056 ) ) ;
#42124 = B_SPLINE_CURVE_WITH_KNOTS ( 'NONE', 1,
 ( #12910, #24258 ),
 .UNSPECIFIED., .F., .F.,
 ( 2, 2 ),
 ( 0.000000000000000000, 1.000000000000000000 ),
 .UNSPECIFIED. ) ;
#42125 = CARTESIAN_POINT ( 'NONE',  ( -15.22312280068192081, -21.51522583983519255, 61.79167741754957177 ) ) ;
#42126 = ORIENTED_EDGE ( 'NONE', *, *, #12398, .T. ) ;
#42127 = FACE_BOUND ( 'NONE', #31807, .T. ) ;
#42128 = CARTESIAN_POINT ( 'NONE',  ( -13.06884191565359643, -20.85448943349606665, 58.23305466536662323 ) ) ;
#42129 = VECTOR ( 'NONE', #2769, 1000.000000000000000 ) ;
#42130 = DIRECTION ( 'NONE',  ( -3.071710424422018668E-17, 6.404604876783312462E-16, 1.000000000000000000 ) ) ;
#42131 = DIRECTION ( 'NONE',  ( 0.000000000000000000, 0.000000000000000000, -1.000000000000000000 ) ) ;
#42132 = CARTESIAN_POINT ( 'NONE',  ( -24.77723895724858494, -16.00713575449774595, 66.24820309305337673 ) ) ;
#42133 = ORIENTED_EDGE ( 'NONE', *, *, #3673, .F. ) ;
#42134 = EDGE_LOOP ( 'NONE', ( #34407, #26379, #31897, #45026 ) ) ;
#42135 = EDGE_CURVE ( 'NONE', #27147, #7125, #43759, .T. ) ;
#42136 = CARTESIAN_POINT ( 'NONE',  ( -14.25677688785123109, -8.066017148268395331, 67.40975083916667643 ) ) ;
#42137 = CARTESIAN_POINT ( 'NONE',  ( -24.29232294273250758, -16.16103065725259214, 62.59328677063434299 ) ) ;
#42138 = ORIENTED_EDGE ( 'NONE', *, *, #33351, .F. ) ;
#42139 = CARTESIAN_POINT ( 'NONE',  ( -10.00117635412376593, -15.44487469174752903, 57.68297500625912733 ) ) ;
#42140 = CARTESIAN_POINT ( 'NONE',  ( -15.81515823392193631, -7.534963144122849066, 67.24733145614881380 ) ) ;
#42141 = CARTESIAN_POINT ( 'NONE',  ( -20.69909385759799036, -8.105421454601382081, 49.25000573077640098 ) ) ;
#42142 = EDGE_CURVE ( 'NONE', #28374, #40286, #42826, .T. ) ;
#42143 = CARTESIAN_POINT ( 'NONE',  ( -21.89130958583942288, -9.354787850460871468, 63.20625856529903075 ) ) ;
#42144 = CARTESIAN_POINT ( 'NONE',  ( -14.36817892824948650, -8.455618309860652104, 67.54503025475185041 ) ) ;
#42145 = CARTESIAN_POINT ( 'NONE',  ( -12.74138925215518015, -14.62063335304397249, 52.02966884056656482 ) ) ;
#42146 = CARTESIAN_POINT ( 'NONE',  ( -16.36796100389485176, -21.77969089362421684, 61.75568160946304630 ) ) ;
#42147 = ORIENTED_EDGE ( 'NONE', *, *, #6369, .T. ) ;
#42148 = PRODUCT_DEFINITION_SHAPE ( 'NONE', 'NONE',  #48735 ) ;
#42149 = EDGE_CURVE ( 'NONE', #45248, #14239, #31496, .T. ) ;
#42150 = DIRECTION ( 'NONE',  ( -3.071710424422018668E-17, 6.404604876783312462E-16, 1.000000000000000000 ) ) ;
#42151 = LINE ( 'NONE', #38188, #13236 ) ;
#42152 = CARTESIAN_POINT ( 'NONE',  ( -11.01197672498281044, -17.74032467813711733, 71.85246142747087106 ) ) ;
#42153 = PLANE ( 'NONE',  #38953 ) ;
#42154 = CARTESIAN_POINT ( 'NONE',  ( -17.44318359119074913, -7.759083889314800864, 67.02599349837787202 ) ) ;
#42155 = ADVANCED_FACE ( 'NONE', ( #39369 ), #121, .T. ) ;
#42156 = CARTESIAN_POINT ( 'NONE',  ( -19.70639753248355319, -21.90109403227812379, 65.57990909513159750 ) ) ;
#42157 = ORIENTED_EDGE ( 'NONE', *, *, #46764, .T. ) ;
#42158 = ORIENTED_EDGE ( 'NONE', *, *, #30237, .F. ) ;
#42159 = CARTESIAN_POINT ( 'NONE',  ( -22.24284385650551954, -8.811426318492348031, 52.18089403414751359 ) ) ;
#42160 = ORIENTED_EDGE ( 'NONE', *, *, #31851, .F. ) ;
#42161 = CARTESIAN_POINT ( 'NONE',  ( -11.21783104652298846, -18.93062367394879431, 64.93202350587574756 ) ) ;
#42162 = CARTESIAN_POINT ( 'NONE',  ( -10.02995829593802668, -13.89786868041111667, 57.63320316755233819 ) ) ;
#42163 = EDGE_LOOP ( 'NONE', ( #35348, #41442 ) ) ;
#42164 = B_SPLINE_CURVE_WITH_KNOTS ( 'NONE', 3,
 ( #39879, #2691, #7322, #25350, #43594, #6153, #22322, #3606, #3867, #41523 ),
 .UNSPECIFIED., .F., .F.,
 ( 4, 2, 2, 2, 4 ),
 ( 0.1272669073658169447, 0.2522669073463095213, 0.3772669073268021256, 0.5022669073072946189, 0.6272669072877872232 ),
 .UNSPECIFIED. ) ;
#42165 = CARTESIAN_POINT ( 'NONE',  ( -10.43726483381679415, -14.35454136775383382, 68.04727144194282573 ) ) ;
#42166 = AXIS2_PLACEMENT_3D ( 'NONE', #19656, #22880, #19162 ) ;
#42167 = CARTESIAN_POINT ( 'NONE',  ( -15.84754116039521676, -7.934039430420517292, 63.87830746700826268 ) ) ;
#42168 = DIRECTION ( 'NONE',  ( -5.731567514496413899E-31, -1.020425574103664789E-16, -1.000000000000000000 ) ) ;
#42169 = EDGE_LOOP ( 'NONE', ( #41581, #12613 ) ) ;
#42170 = CARTESIAN_POINT ( 'NONE',  ( -23.83080496556880945, -17.75212211224490133, 59.28906343887996400 ) ) ;
#42171 = CARTESIAN_POINT ( 'NONE',  ( -23.86921235852081580, -8.358587496134095574, 54.49999999999995026 ) ) ;
#42172 = ORIENTED_EDGE ( 'NONE', *, *, #23876, .F. ) ;
#42173 = DIRECTION ( 'NONE',  ( 1.000000000000000000, 0.000000000000000000, 0.000000000000000000 ) ) ;
#42174 = ADVANCED_FACE ( 'NONE', ( #27560 ), #9592, .F. ) ;
#42175 = CARTESIAN_POINT ( 'NONE',  ( -23.76644255318129595, -11.73037447993928239, 62.95778050648025470 ) ) ;
#42176 = ORIENTED_EDGE ( 'NONE', *, *, #16330, .T. ) ;
#42177 = CARTESIAN_POINT ( 'NONE',  ( -11.10300703817161327, -10.86615712478015539, 57.39398594787093089 ) ) ;
#42178 = CARTESIAN_POINT ( 'NONE',  ( -22.47920019561985328, -20.28188657713170073, 65.88234471252430069 ) ) ;
#42179 = CARTESIAN_POINT ( 'NONE',  ( -15.53265176333180619, -21.60105060138385014, 72.33103357390284316 ) ) ;
#42180 = VERTEX_POINT ( 'NONE', #17180 ) ;
#42181 = CARTESIAN_POINT ( 'NONE',  ( -10.66703313327717417, -12.79807994555918782, 64.56836111017611302 ) ) ;
#42182 = DIRECTION ( 'NONE',  ( 0.000000000000000000, 1.000000000000000000, -0.000000000000000000 ) ) ;
#42183 = B_SPLINE_CURVE_WITH_KNOTS ( 'NONE', 1,
 ( #42086, #16688 ),
 .UNSPECIFIED., .F., .F.,
 ( 2, 2 ),
 ( 0.000000000000000000, 1.000000000000000000 ),
 .UNSPECIFIED. ) ;
#42184 = CARTESIAN_POINT ( 'NONE',  ( -15.25351580106674376, -21.52054300433004386, 72.13755606438517987 ) ) ;
#42185 = CARTESIAN_POINT ( 'NONE',  ( -21.24554520941113367, -21.20453976546471608, 65.76949229983627276 ) ) ;
#42186 = CARTESIAN_POINT ( 'NONE',  ( -14.79922817013080483, -7.836842635312091687, 57.03495431467663224 ) ) ;
#42187 = DIRECTION ( 'NONE',  ( -0.1922068328301544116, -0.9813544382196450755, 7.804899501296266931E-08 ) ) ;
#42188 = CARTESIAN_POINT ( 'NONE',  ( -22.75539019595754908, -10.19575032747719412, 66.82710158566565894 ) ) ;
#42189 = CARTESIAN_POINT ( 'NONE',  ( -20.88397215374023119, -20.89444276828103142, 62.40006029053370895 ) ) ;
#42190 = DIRECTION ( 'NONE',  ( -1.000000000000000000, -1.669677910507523057E-21, -6.493791346278465266E-22 ) ) ;
#42191 = CARTESIAN_POINT ( 'NONE',  ( -17.18034385650551954, -6.424090610841176385, 49.80797279389978627 ) ) ;
#42192 = ORIENTED_EDGE ( 'NONE', *, *, #227, .T. ) ;
#42193 = EDGE_CURVE ( 'NONE', #1317, #20133, #18436, .T. ) ;
#42194 = DIRECTION ( 'NONE',  ( 0.1675476790616295675, -0.9858639740050658684, 1.222863418168464292E-17 ) ) ;
#42195 = CARTESIAN_POINT ( 'NONE',  ( -10.47120130798260185, -17.48512196787819661, 64.73401085767241625 ) ) ;
#42196 = VERTEX_POINT ( 'NONE', #29493 ) ;
#42197 = CARTESIAN_POINT ( 'NONE',  ( -15.77151528785019430, -19.20744933288474954, 49.52966884056656482 ) ) ;
#42198 = CARTESIAN_POINT ( 'NONE',  ( -12.82020749880560651, -17.33244462614775827, 49.52966884056655772 ) ) ;
#42199 = CARTESIAN_POINT ( 'NONE',  ( -45.42186609336205549, -13.24559821555319239, 70.87000000000000455 ) ) ;
#42200 = ORIENTED_EDGE ( 'NONE', *, *, #46838, .T. ) ;
#42201 = CARTESIAN_POINT ( 'NONE',  ( -18.46885980906216318, -22.18634193242058572, 68.92859349268570668 ) ) ;
#42202 = CIRCLE ( 'NONE', #42166, 1.250000000000001110 ) ;
#42203 = DIRECTION ( 'NONE',  ( 0.5327540375067998379, 0.8462701315302333382, 7.203825861310634525E-08 ) ) ;
#42204 = VECTOR ( 'NONE', #38140, 1000.000000000000000 ) ;
#42205 = EDGE_CURVE ( 'NONE', #7167, #25404, #2841, .T. ) ;
#42206 = CARTESIAN_POINT ( 'NONE',  ( -10.08886380456056742, -16.11191617737164705, 68.07744192415786699 ) ) ;
#42207 = ORIENTED_EDGE ( 'NONE', *, *, #24826, .T. ) ;
#42208 = CARTESIAN_POINT ( 'NONE',  ( -15.62222905942471840, -7.993050613273783966, 70.89517703929612935 ) ) ;
#42209 = EDGE_CURVE ( 'NONE', #37645, #48120, #21860, .T. ) ;
#42210 = CARTESIAN_POINT ( 'NONE',  ( -12.86542566280920319, -8.916737054783007821, 67.47919149430154562 ) ) ;
#42211 = CARTESIAN_POINT ( 'NONE',  ( -10.37560970945560967, -14.44337087574636769, 61.07388280500082800 ) ) ;
#42212 = CARTESIAN_POINT ( 'NONE',  ( 8.575906144586951996, 11.89145878086734065, 50.31056258843197782 ) ) ;
#42213 = CARTESIAN_POINT ( 'NONE',  ( -13.92409385541305511, -10.60920654474410618, 81.49999999999998579 ) ) ;
#42214 = ORIENTED_EDGE ( 'NONE', *, *, #21074, .F. ) ;
#42215 = ORIENTED_EDGE ( 'NONE', *, *, #30180, .F. ) ;
#42216 = CARTESIAN_POINT ( 'NONE',  ( -23.36784385541304232, -9.357632978295830739, 49.97845033065684106 ) ) ;
#42217 = CARTESIAN_POINT ( 'NONE',  ( -14.07539642552819359, -8.605278304397881328, 74.19954655214911554 ) ) ;
#42218 = CARTESIAN_POINT ( 'NONE',  ( -23.34080049944153856, -11.06854047984963962, 73.55296409646045674 ) ) ;
#42219 = DIRECTION ( 'NONE',  ( -0.1738928961406289164, 0.9847645711904029486, 7.871847295470929299E-08 ) ) ;
#42220 = EDGE_CURVE ( 'NONE', #34559, #44694, #4863, .T. ) ;
#42221 = EDGE_CURVE ( 'NONE', #43276, #31666, #23798, .T. ) ;
#42222 = B_SPLINE_CURVE_WITH_KNOTS ( 'NONE', 1,
 ( #33409, #19830 ),
 .UNSPECIFIED., .F., .F.,
 ( 2, 2 ),
 ( 0.000000000000000000, 1.000000000000000000 ),
 .UNSPECIFIED. ) ;
#42223 = CARTESIAN_POINT ( 'NONE',  ( -17.39128687056474121, -21.86710222072322907, 58.54986106076864161 ) ) ;
#42224 = ADVANCED_FACE ( 'NONE', ( #26054 ), #18153, .T. ) ;
#42225 = CARTESIAN_POINT ( 'NONE',  ( -20.88289085685542545, -8.210692395643533814, 59.88479313977884289 ) ) ;
#42226 = DIRECTION ( 'NONE',  ( -4.115385489419834812E-17, -0.9999954153791275058, -0.003028072113822189229 ) ) ;
#42227 = CARTESIAN_POINT ( 'NONE',  ( -11.60526899143904345, -18.79015832504765626, 68.23161775275829655 ) ) ;
#42228 =( BOUNDED_CURVE ( )  B_SPLINE_CURVE ( 3, ( #43533, #44498, #39818, #32898 ),
 .UNSPECIFIED., .F., .F. ) 
 B_SPLINE_CURVE_WITH_KNOTS ( ( 4, 4 ),
 ( 0.4074455897393627901, 0.5000000000000000000 ),
 .UNSPECIFIED. ) 
 CURVE ( )  GEOMETRIC_REPRESENTATION_ITEM ( )  RATIONAL_B_SPLINE_CURVE ( ( 0.6983129098260937306, 0.7760317562606900976, 0.8765941196519897449, 0.9999999999999861222 ) ) 
 REPRESENTATION_ITEM ( '' )  );
#42229 = ORIENTED_EDGE ( 'NONE', *, *, #39961, .F. ) ;
#42230 = CARTESIAN_POINT ( 'NONE',  ( -24.41687585628244506, -14.48898472626409273, 66.18292730085975961 ) ) ;
#42231 = DIRECTION ( 'NONE',  ( 0.4182840851231335866, -0.9083162577718748576, 8.112345261759808545E-09 ) ) ;
#42232 = AXIS2_PLACEMENT_3D ( 'NONE', #35876, #40546, #6097 ) ;
#42233 = VECTOR ( 'NONE', #11892, 1000.000000000000000 ) ;
#42234 = ORIENTED_EDGE ( 'NONE', *, *, #35518, .T. ) ;
#42235 = CARTESIAN_POINT ( 'NONE',  ( -13.30482829320324534, -21.01685844473519182, 61.62372190405099559 ) ) ;
#42236 = CARTESIAN_POINT ( 'NONE',  ( -9.974527725170556636, -14.89026794202819204, 74.99790105621293890 ) ) ;
#42237 = ORIENTED_EDGE ( 'NONE', *, *, #41004, .F. ) ;
#42238 = CARTESIAN_POINT ( 'NONE',  ( -18.13127753087942295, -22.22561600718755770, 65.53870465771630904 ) ) ;
#42239 = VERTEX_POINT ( 'NONE', #7101 ) ;
#42240 = B_SPLINE_CURVE_WITH_KNOTS ( 'NONE', 1,
 ( #35839, #2124 ),
 .UNSPECIFIED., .F., .F.,
 ( 2, 2 ),
 ( 0.000000000000000000, 1.000000000000000000 ),
 .UNSPECIFIED. ) ;
#42241 = CARTESIAN_POINT ( 'NONE',  ( -10.00824906877580567, -15.52305002423542390, 57.68980053291110721 ) ) ;
#42242 = AXIS2_PLACEMENT_3D ( 'NONE', #46665, #12677, #12912 ) ;
#42243 = CARTESIAN_POINT ( 'NONE',  ( -15.11795752579537400, -21.47139868945932051, 65.40596679997382523 ) ) ;
#42244 = CARTESIAN_POINT ( 'NONE',  ( -15.11195812866605692, -21.41632606413040918, 65.10596681519622564 ) ) ;
#42245 = VERTEX_POINT ( 'NONE', #29009 ) ;
#42246 = CARTESIAN_POINT ( 'NONE',  ( -21.57940561823839332, -9.104090476609597360, 63.34720799502051847 ) ) ;
#42247 = FACE_OUTER_BOUND ( 'NONE', #11066, .T. ) ;
#42248 =( BOUNDED_CURVE ( )  B_SPLINE_CURVE ( 3, ( #41327, #27282, #4633, #18923 ),
 .UNSPECIFIED., .F., .F. ) 
 B_SPLINE_CURVE_WITH_KNOTS ( ( 4, 4 ),
 ( 0.4074455897269660953, 0.5000000000000000000 ),
 .UNSPECIFIED. ) 
 CURVE ( )  GEOMETRIC_REPRESENTATION_ITEM ( )  RATIONAL_B_SPLINE_CURVE ( ( 0.6983129097948570507, 0.7760317562337696318, 0.8765941196354886111, 1.000000000000025535 ) ) 
 REPRESENTATION_ITEM ( '' )  );
#42249 = CARTESIAN_POINT ( 'NONE',  ( -13.50190746284422794, -17.39609839546894676, 49.52966884056655772 ) ) ;
#42250 = DIRECTION ( 'NONE',  ( -3.071710424422018668E-17, 6.404604876783312462E-16, 1.000000000000000000 ) ) ;
#42251 = APPLICATION_PROTOCOL_DEFINITION ( 'draft international standard', 'automotive_design', 1998, #6119 ) ;
#42252 = CARTESIAN_POINT ( 'NONE',  ( -11.44438386955935272, -18.44830926459003351, 57.91600554991716621 ) ) ;
#42253 = DIRECTION ( 'NONE',  ( 0.9687793358424802159, -0.2479245821708745412, 0.000000000000000000 ) ) ;
#42254 = FACE_OUTER_BOUND ( 'NONE', #17938, .T. ) ;
#42255 = ORIENTED_EDGE ( 'NONE', *, *, #3169, .F. ) ;
#42256 = CARTESIAN_POINT ( 'NONE',  ( -24.35389707626741185, -16.10709931453380861, 62.87856533165624029 ) ) ;
#42257 = ORIENTED_EDGE ( 'NONE', *, *, #35715, .F. ) ;
#42258 = CARTESIAN_POINT ( 'NONE',  ( -11.49911252271374273, -19.32675654123934095, 71.80030491464860631 ) ) ;
#42259 = CARTESIAN_POINT ( 'NONE',  ( -16.71219879347879100, -22.22520166962337740, 68.81065243885818461 ) ) ;
#42260 = VERTEX_POINT ( 'NONE', #7351 ) ;
#42261 = B_SPLINE_CURVE_WITH_KNOTS ( 'NONE', 1,
 ( #21359, #44256 ),
 .UNSPECIFIED., .F., .F.,
 ( 2, 2 ),
 ( 0.000000000000000000, 1.000000000000000000 ),
 .UNSPECIFIED. ) ;
#42262 = DIRECTION ( 'NONE',  ( 1.927470528863119542E-16, 0.000000000000000000, -1.000000000000000000 ) ) ;
#42263 =( BOUNDED_CURVE ( )  B_SPLINE_CURVE ( 3, ( #47080, #17263, #47331, #16779 ),
 .UNSPECIFIED., .F., .F. ) 
 B_SPLINE_CURVE_WITH_KNOTS ( ( 4, 4 ),
 ( 0.4074455897393777226, 0.5000000000000000000 ),
 .UNSPECIFIED. ) 
 CURVE ( )  GEOMETRIC_REPRESENTATION_ITEM ( )  RATIONAL_B_SPLINE_CURVE ( ( 0.6983129098261363632, 0.7760317562607240705, 0.8765941196520085077, 0.9999999999999816813 ) ) 
 REPRESENTATION_ITEM ( '' )  );
#42264 = ADVANCED_FACE ( 'NONE', ( #22349 ), #6844, .T. ) ;
#42265 = ORIENTED_EDGE ( 'NONE', *, *, #37906, .F. ) ;
#42266 = VERTEX_POINT ( 'NONE', #3148 ) ;
#42267 = EDGE_LOOP ( 'NONE', ( #32309, #15559, #42096, #42014 ) ) ;
#42268 = CARTESIAN_POINT ( 'NONE',  ( -10.03035355355731006, -15.72374577095404824, 61.22284339518546403 ) ) ;
#42269 = CARTESIAN_POINT ( 'NONE',  ( -18.50931870666621037, -21.77518001355031529, 72.28510940651260341 ) ) ;
#42270 = DIRECTION ( 'NONE',  ( 0.9687793358424819923, -0.2479245821708680464, 0.000000000000000000 ) ) ;
#42271 = CARTESIAN_POINT ( 'NONE',  ( -21.30258078786002329, -8.981766571127032250, 73.90128699495393505 ) ) ;
#42272 = CARTESIAN_POINT ( 'NONE',  ( -10.25351306168449383, -12.78524163461458762, 64.38180785400611228 ) ) ;
#42273 = CARTESIAN_POINT ( 'NONE',  ( -12.49693318139922482, -20.39741725237024284, 71.94620299007212338 ) ) ;
#42274 = VECTOR ( 'NONE', #48705, 1000.000000000000000 ) ;
#42275 = VERTEX_POINT ( 'NONE', #2664 ) ;
#42276 = ORIENTED_EDGE ( 'NONE', *, *, #11093, .F. ) ;
#42277 = DIRECTION ( 'NONE',  ( 3.413470714839332458E-33, -1.190614954331866791E-16, 1.000000000000000000 ) ) ;
#42278 = CARTESIAN_POINT ( 'NONE',  ( -19.80301260837064703, -21.44571507605098404, 69.23482476707422961 ) ) ;
#42279 = DIRECTION ( 'NONE',  ( 5.329554274754248866E-07, 1.313503380136696700E-06, 0.9999999999989952482 ) ) ;
#42280 = VECTOR ( 'NONE', #45053, 1000.000000000000000 ) ;
#42281 = CARTESIAN_POINT ( 'NONE',  ( -14.86627107493491984, -7.811969877679347363, 56.96504568426624360 ) ) ;
#42282 = EDGE_LOOP ( 'NONE', ( #39271, #8777, #2096, #21997, #25453 ) ) ;
#42283 = CARTESIAN_POINT ( 'NONE',  ( -13.18659385650551918, -9.302874398569244363, 51.68646062012417985 ) ) ;
#42284 = EDGE_CURVE ( 'NONE', #27092, #46437, #22039, .T. ) ;
#42285 = EDGE_LOOP ( 'NONE', ( #23895, #39359, #33462, #20493, #5957 ) ) ;
#42286 = EDGE_CURVE ( 'NONE', #3865, #34178, #45139, .T. ) ;
#42287 = ADVANCED_FACE ( 'NONE', ( #18638 ), #20229, .T. ) ;
#42288 = CARTESIAN_POINT ( 'NONE',  ( -21.52726260838264949, -9.076274878514672295, 70.13132538915753855 ) ) ;
#42289 = CARTESIAN_POINT ( 'NONE',  ( -17.32045713178291280, -7.809913985087237442, 67.03542077588672043 ) ) ;
#42290 = VERTEX_POINT ( 'NONE', #45029 ) ;
#42291 = CARTESIAN_POINT ( 'NONE',  ( -20.89284385541298761, -8.630756214087167422, 51.74842643355258076 ) ) ;
#42292 = CARTESIAN_POINT ( 'NONE',  ( -10.76216126260078987, -17.12512740823429525, 65.04228012599854480 ) ) ;
#42293 = CARTESIAN_POINT ( 'NONE',  ( -12.64905295888074299, -9.611711778639854487, 57.23368232919959553 ) ) ;
#42294 = APPLICATION_CONTEXT ( 'automotive_design' ) ;
#42295 = ORIENTED_EDGE ( 'NONE', *, *, #14715, .F. ) ;
#42296 = AXIS2_PLACEMENT_3D ( 'NONE', #10850, #47564, #13796 ) ;
#42297 = CARTESIAN_POINT ( 'NONE',  ( -15.97587070454731517, -21.71254611733878193, 58.37765857771692879 ) ) ;
#42298 = DIRECTION ( 'NONE',  ( 0.000000000000000000, 0.9999954153791273948, 0.003028072113819836077 ) ) ;
#42299 = VERTEX_POINT ( 'NONE', #38577 ) ;
#42300 = DIRECTION ( 'NONE',  ( 3.413470714839332458E-33, -1.190614954331866791E-16, 1.000000000000000000 ) ) ;
#42301 = CIRCLE ( 'NONE', #48581, 4.686499999999998778 ) ;
#42302 = CIRCLE ( 'NONE', #32855, 1.700000000000001954 ) ;
#42303 = EDGE_LOOP ( 'NONE', ( #34750, #38291, #34689, #2199, #44985 ) ) ;
#42304 = CARTESIAN_POINT ( 'NONE',  ( -14.99706723701585354, -21.85287888328288375, 65.29092001793476641 ) ) ;
#42305 = DIRECTION ( 'NONE',  ( -3.071710424422018668E-17, 6.404604876783312462E-16, 1.000000000000000000 ) ) ;
#42306 = ORIENTED_EDGE ( 'NONE', *, *, #13351, .F. ) ;
#42307 = CARTESIAN_POINT ( 'NONE',  ( -33.52409385541305653, -8.109206544744111511, 49.44999999999998863 ) ) ;
#42309 = ADVANCED_FACE ( 'NONE', ( #30965 ), #22596, .T. ) ;
#42308 = CARTESIAN_POINT ( 'NONE',  ( -23.84761965343929901, -12.02338239010575194, 59.59308729769960422 ) ) ;
#42310 = CARTESIAN_POINT ( 'NONE',  ( -21.99019323879806365, -13.75373571565882713, 49.52966884056655772 ) ) ;
#42311 = ORIENTED_EDGE ( 'NONE', *, *, #20396, .F. ) ;
#42312 = CARTESIAN_POINT ( 'NONE',  ( -10.84896266223257122, -17.37486770053218521, 71.71150890757306229 ) ) ;
#42313 = AXIS2_PLACEMENT_3D ( 'NONE', #26059, #15683, #45034 ) ;
#42314 = CARTESIAN_POINT ( 'NONE',  ( -20.88270717056239789, -21.40782548341276481, 58.82970473467946704 ) ) ;
#42315 = CARTESIAN_POINT ( 'NONE',  ( -10.92393577332946641, -17.40806695695071227, 68.38105336835567982 ) ) ;
#42316 = ORIENTED_EDGE ( 'NONE', *, *, #32095, .T. ) ;
#42317 = DIRECTION ( 'NONE',  ( 1.000000000000000000, -4.164305804376849172E-17, 1.614929280266638808E-16 ) ) ;
#42318 = AXIS2_PLACEMENT_3D ( 'NONE', #41397, #6700, #29102 ) ;
#42319 = B_SPLINE_CURVE_WITH_KNOTS ( 'NONE', 3,
 ( #32477, #35905, #24370, #6127, #13731, #17677, #17915, #40343, #32240, #6374 ),
 .UNSPECIFIED., .F., .F.,
 ( 4, 2, 2, 2, 4 ),
 ( 0.000000000000000000, 0.2500000000000000000, 0.5000000000000000000, 0.7500000000000000000, 1.000000000000000000 ),
 .UNSPECIFIED. ) ;
#42320 = DIRECTION ( 'NONE',  ( 0.000000000000000000, -0.000000000000000000, -1.000000000000000000 ) ) ;
#42321 = ORIENTED_EDGE ( 'NONE', *, *, #24056, .T. ) ;
#42322 = ORIENTED_EDGE ( 'NONE', *, *, #39671, .T. ) ;
#42323 = CARTESIAN_POINT ( 'NONE',  ( -10.49015519723160850, -15.76906674594861002, 61.11077061167396351 ) ) ;
#42324 = CARTESIAN_POINT ( 'NONE',  ( -10.16786014542261007, -13.12079378898483384, 71.25182636653194379 ) ) ;
#42325 = EDGE_CURVE ( 'NONE', #41967, #7285, #20817, .T. ) ;
#42326 = DIRECTION ( 'NONE',  ( -1.000000000000000000, 4.164305804376849172E-17, -1.614929280266638808E-16 ) ) ;
#42327 = CARTESIAN_POINT ( 'NONE',  ( -20.38659385650551670, -9.302874398569244363, 51.68646062012417985 ) ) ;
#42328 = CARTESIAN_POINT ( 'NONE',  ( -12.34455782425648351, -9.992743752570305560, 57.19821645454700842 ) ) ;
#42329 = CARTESIAN_POINT ( 'NONE',  ( -23.65624121974494543, -11.51332442490695129, 66.42214514605623776 ) ) ;
#42330 = DIRECTION ( 'NONE',  ( -0.9687793358424819923, 0.2479245821708680464, 0.000000000000000000 ) ) ;
#42331 = CARTESIAN_POINT ( 'NONE',  ( -23.77562434277295367, -17.86939608417919345, 59.01850491586762359 ) ) ;
#42332 = ORIENTED_EDGE ( 'NONE', *, *, #37615, .F. ) ;
#42333 = ORIENTED_EDGE ( 'NONE', *, *, #30788, .T. ) ;
#42334 = CARTESIAN_POINT ( 'NONE',  ( -11.46310342473229049, -11.03940158154180651, 61.09374645412970750 ) ) ;
#42335 = CARTESIAN_POINT ( 'NONE',  ( -50.42609385541305755, -14.80920654474413745, 60.01764705882352047 ) ) ;
#42336 =( BOUNDED_CURVE ( )  B_SPLINE_CURVE ( 3, ( #9226, #23769, #24250, #39256 ),
 .UNSPECIFIED., .F., .F. ) 
 B_SPLINE_CURVE_WITH_KNOTS ( ( 4, 4 ),
 ( 0.9074455897393661763, 1.000000000000000000 ),
 .UNSPECIFIED. ) 
 CURVE ( )  GEOMETRIC_REPRESENTATION_ITEM ( )  RATIONAL_B_SPLINE_CURVE ( ( 0.6983129098260806300, 0.7760317562606875441, 0.8765941196519939638, 1.000000000000000000 ) ) 
 REPRESENTATION_ITEM ( '' )  );
#42337 = CARTESIAN_POINT ( 'NONE',  ( -18.79049830835916524, -7.892586073225762000, 70.38540174208183942 ) ) ;
#42338 = AXIS2_PLACEMENT_3D ( 'NONE', #40483, #40728, #22266 ) ;
#42339 = VECTOR ( 'NONE', #43520, 1000.000000000000000 ) ;
#42340 = VERTEX_POINT ( 'NONE', #45757 ) ;
#42341 = EDGE_LOOP ( 'NONE', ( #22168, #5692, #28661, #35457, #5643 ) ) ;
#42342 = EDGE_CURVE ( 'NONE', #33146, #31985, #851, .T. ) ;
#42343 = CARTESIAN_POINT ( 'NONE',  ( -28.42409385541305511, -6.859206544744110623, 45.99999999999998579 ) ) ;
#42344 = DIRECTION ( 'NONE',  ( -3.071710424422018668E-17, 6.404604876783312462E-16, 1.000000000000000000 ) ) ;
#42345 = DIRECTION ( 'NONE',  ( -3.298726454030011118E-06, 1.683524824177191357E-06, 0.9999999999931419303 ) ) ;
#42346 = CARTESIAN_POINT ( 'NONE',  ( -15.82259855879412846, -7.533287975791289171, 67.25511890406325222 ) ) ;
#42347 = CIRCLE ( 'NONE', #35261, 0.5000000000000004441 ) ;
#42348 = VERTEX_POINT ( 'NONE', #8087 ) ;
#42349 = CARTESIAN_POINT ( 'NONE',  ( -24.45714095472541771, -14.31630891555218987, 69.66747352629326429 ) ) ;
#42350 = EDGE_CURVE ( 'NONE', #24257, #3170, #29993, .T. ) ;
#42351 = ADVANCED_FACE ( 'NONE', ( #18904 ), #7593, .T. ) ;
#42352 = CARTESIAN_POINT ( 'NONE',  ( -24.41553149706675896, -15.71832598455623398, 69.81835354388927328 ) ) ;
#42353 = ORIENTED_EDGE ( 'NONE', *, *, #18957, .F. ) ;
#42354 = EDGE_CURVE ( 'NONE', #34358, #14163, #41386, .T. ) ;
#42355 = CARTESIAN_POINT ( 'NONE',  ( -24.31477923169101629, -16.30090137217950996, 59.40860294853779777 ) ) ;
#42356 = EDGE_CURVE ( 'NONE', #34511, #34680, #46982, .T. ) ;
#42357 = CARTESIAN_POINT ( 'NONE',  ( -24.22219984651093583, -16.48362222048029579, 59.19502791767319394 ) ) ;
#42358 = EDGE_LOOP ( 'NONE', ( #8284, #26977 ) ) ;
#42359 = CARTESIAN_POINT ( 'NONE',  ( -20.37524731190853799, -7.968593674222963053, 70.35826172290288127 ) ) ;
#42360 = ORIENTED_EDGE ( 'NONE', *, *, #45086, .T. ) ;
#42361 = CYLINDRICAL_SURFACE ( 'NONE', #12282, 0.1500000000000061562 ) ;
#42362 = CARTESIAN_POINT ( 'NONE',  ( -17.42409385541299471, -14.80920654474435771, 49.52966884056655772 ) ) ;
#42363 = ORIENTED_EDGE ( 'NONE', *, *, #44150, .T. ) ;
#42364 = CARTESIAN_POINT ( 'NONE',  ( -24.29299122354570883, -17.69571185755203757, 62.58705726155704951 ) ) ;
#42365 = FACE_OUTER_BOUND ( 'NONE', #19237, .T. ) ;
#42366 = EDGE_CURVE ( 'NONE', #12617, #18903, #48473, .T. ) ;
#42367 = CARTESIAN_POINT ( 'NONE',  ( -17.83034385650552167, -9.794322478646142471, 51.19202720610083190 ) ) ;
#42368 = AXIS2_PLACEMENT_3D ( 'NONE', #3467, #40414, #29090 ) ;
#42369 = CARTESIAN_POINT ( 'NONE',  ( -15.47894645291934523, -21.58867816219044755, 68.46104220717563749 ) ) ;
#42370 = AXIS2_PLACEMENT_3D ( 'NONE', #20709, #47049, #17236 ) ;
#42371 = FACE_OUTER_BOUND ( 'NONE', #21121, .T. ) ;
#42372 = CARTESIAN_POINT ( 'NONE',  ( -14.86587017669673649, -21.80700303724089295, 61.74945191855038473 ) ) ;
#42373 = ORIENTED_EDGE ( 'NONE', *, *, #25985, .T. ) ;
#42374 = DIRECTION ( 'NONE',  ( -5.731567514496413899E-31, -1.020425574103664789E-16, -1.000000000000000000 ) ) ;
#42375 = VECTOR ( 'NONE', #37688, 1000.000000000000114 ) ;
#42376 = CIRCLE ( 'NONE', #41602, 6.899999999999999467 ) ;
#42377 = CARTESIAN_POINT ( 'NONE',  ( -11.89466307818281798, -10.43082414681992276, 74.85374085024349711 ) ) ;
#42378 = DIRECTION ( 'NONE',  ( 0.000000000000000000, 0.007114381193220285608, -0.9999746924698833528 ) ) ;
#42379 = CARTESIAN_POINT ( 'NONE',  ( -20.49479342634786505, -8.021289690749126677, 66.94137462304620101 ) ) ;
#42380 = CYLINDRICAL_SURFACE ( 'NONE', #5929, 0.1500000000000010769 ) ;
#42381 = ORIENTED_EDGE ( 'NONE', *, *, #43261, .T. ) ;
#42382 = EDGE_LOOP ( 'NONE', ( #46141, #8605, #28804, #14612 ) ) ;
#42383 = CARTESIAN_POINT ( 'NONE',  ( -15.43182990062313564, -8.046249867383863830, 74.36513541778452918 ) ) ;
#42384 = CARTESIAN_POINT ( 'NONE',  ( -14.60628068055246942, -7.912570010659592867, 60.36350377317607752 ) ) ;
#42385 = VERTEX_POINT ( 'NONE', #37592 ) ;
#42386 = CARTESIAN_POINT ( 'NONE',  ( -22.38767768884900988, -19.81996202295057330, 65.58933089874275879 ) ) ;
#42387 = CARTESIAN_POINT ( 'NONE',  ( -23.98503169607928953, -17.39005800936845603, 66.22885190747201989 ) ) ;
#42388 = CIRCLE ( 'NONE', #10141, 1.249999999999999556 ) ;
#42389 = CARTESIAN_POINT ( 'NONE',  ( -21.24651499925844078, -18.40803921647045982, 49.52966884056656482 ) ) ;
#42390 = CARTESIAN_POINT ( 'NONE',  ( -17.33515886584969223, -7.808492153737893737, 70.56206024376236030 ) ) ;
#42391 =( BOUNDED_CURVE ( )  B_SPLINE_CURVE ( 3, ( #20993, #13339, #5503, #21485 ),
 .UNSPECIFIED., .F., .F. ) 
 B_SPLINE_CURVE_WITH_KNOTS ( ( 4, 4 ),
 ( 4.712388980384689674, 4.982321776218093135 ),
 .UNSPECIFIED. ) 
 CURVE ( )  GEOMETRIC_REPRESENTATION_ITEM ( )  RATIONAL_B_SPLINE_CURVE ( ( 1.000000000000000000, 0.9939372354399834686, 0.9939372354399834686, 1.000000000000000000 ) ) 
 REPRESENTATION_ITEM ( '' )  );
#42392 = CARTESIAN_POINT ( 'NONE',  ( -17.09591293804728807, -10.13421140726271297, 52.02966884056656482 ) ) ;
#42393 = CARTESIAN_POINT ( 'NONE',  ( -23.55000801791835485, -19.04907288299056489, 65.93115295761097627 ) ) ;
#42394 = CARTESIAN_POINT ( 'NONE',  ( -16.89979169948162863, -10.14008855580012636, 49.52966884056655772 ) ) ;
#42395 = ORIENTED_EDGE ( 'NONE', *, *, #27682, .T. ) ;
#42396 = CARTESIAN_POINT ( 'NONE',  ( -10.02191625022346955, -15.65273779443635327, 61.15293638507743168 ) ) ;
#42397 = CARTESIAN_POINT ( 'NONE',  ( -19.23866243364646422, -21.62168334911581269, 58.52507384657483414 ) ) ;
#42398 = CARTESIAN_POINT ( 'NONE',  ( -23.95290610889346539, -17.47904830382568875, 69.50519765973122333 ) ) ;
#42399 = CARTESIAN_POINT ( 'NONE',  ( -19.18086540149941399, -19.15397765319887569, 49.52966884056656482 ) ) ;
#42400 = FACE_OUTER_BOUND ( 'NONE', #901, .T. ) ;
#42401 = B_SPLINE_CURVE_WITH_KNOTS ( 'NONE', 3,
 ( #25594, #48009, #10103, #21438, #25126, #40144, #10818, #32738, #33204, #40859 ),
 .UNSPECIFIED., .F., .F.,
 ( 4, 2, 2, 2, 4 ),
 ( 0.000000000000000000, 0.2500000000000000000, 0.5000000000000000000, 0.7500000000000000000, 1.000000000000000000 ),
 .UNSPECIFIED. ) ;
#42402 = EDGE_CURVE ( 'NONE', #26226, #4075, #8690, .T. ) ;
#42403 =( BOUNDED_CURVE ( )  B_SPLINE_CURVE ( 3, ( #9224, #39006, #2307, #27923 ),
 .UNSPECIFIED., .F., .F. ) 
 B_SPLINE_CURVE_WITH_KNOTS ( ( 4, 4 ),
 ( 0.000000000000000000, 0.4074455897393611248 ),
 .UNSPECIFIED. ) 
 CURVE ( )  GEOMETRIC_REPRESENTATION_ITEM ( )  RATIONAL_B_SPLINE_CURVE ( ( 1.000000000000000000, 0.4567392136813394066, 0.3561768502900330979, 0.6983129098260809631 ) ) 
 REPRESENTATION_ITEM ( '' )  );
#42404 = ORIENTED_EDGE ( 'NONE', *, *, #1526, .F. ) ;
#42405 = VERTEX_POINT ( 'NONE', #11512 ) ;
#42406 = CARTESIAN_POINT ( 'NONE',  ( -22.52409385650551954, -6.426201560718812544, 50.50509628382439331 ) ) ;
#42407 = VERTEX_POINT ( 'NONE', #4144 ) ;
#42408 = EDGE_CURVE ( 'NONE', #26785, #25255, #34152, .T. ) ;
#42409 = CARTESIAN_POINT ( 'NONE',  ( -11.97744758732939019, -9.726227503278199293, 60.75906873251374662 ) ) ;
#42410 = VECTOR ( 'NONE', #21157, 1000.000000000000000 ) ;
#42411 = CARTESIAN_POINT ( 'NONE',  ( -21.80947398209100285, -9.353160252369512762, 63.49153755919518005 ) ) ;
#42412 =( GEOMETRIC_REPRESENTATION_CONTEXT ( 3 ) GLOBAL_UNCERTAINTY_ASSIGNED_CONTEXT ( ( #43531 ) ) GLOBAL_UNIT_ASSIGNED_CONTEXT ( ( #30536, #33961, #23145 ) ) REPRESENTATION_CONTEXT ( 'NONE', 'WORKASPACE' ) );
#42413 = ORIENTED_EDGE ( 'NONE', *, *, #9077, .T. ) ;
#42414 = CIRCLE ( 'NONE', #43188, 2.000000000000001332 ) ;
#42415 = CARTESIAN_POINT ( 'NONE',  ( -10.43414264852987117, -14.42617553249795392, 68.14183543910880303 ) ) ;
#42416 = CARTESIAN_POINT ( 'NONE',  ( -18.53202070066404517, -7.846807721809618386, 73.84064401782792686 ) ) ;
#42417 = ORIENTED_EDGE ( 'NONE', *, *, #23639, .F. ) ;
#42418 = EDGE_CURVE ( 'NONE', #33406, #27678, #5147, .T. ) ;
#42419 = CARTESIAN_POINT ( 'NONE',  ( -23.89931086185965370, -17.60652826309538099, 59.21198374917257468 ) ) ;
#42420 = AXIS2_PLACEMENT_3D ( 'NONE', #45105, #17987, #10622 ) ;
#42421 = CARTESIAN_POINT ( 'NONE',  ( -23.18182585610446722, -10.73448348362502536, 59.90203689567525913 ) ) ;
#42422 = EDGE_CURVE ( 'NONE', #36361, #40825, #23096, .T. ) ;
#42423 = VERTEX_POINT ( 'NONE', #19633 ) ;
#42424 = CARTESIAN_POINT ( 'NONE',  ( -19.86401518824997225, -21.42384811948916834, 69.22010401872219632 ) ) ;
#42425 = CARTESIAN_POINT ( 'NONE',  ( -17.54757171063225485, -7.760139436107405864, 63.84497264672818773 ) ) ;
#42426 = ORIENTED_EDGE ( 'NONE', *, *, #25727, .F. ) ;
#42427 = B_SPLINE_CURVE_WITH_KNOTS ( 'NONE', 3,
 ( #22251, #6749, #37490, #37242, #6989, #18539, #37007, #44669, #29893, #40471 ),
 .UNSPECIFIED., .F., .F.,
 ( 4, 2, 2, 2, 4 ),
 ( 0.000000000000000000, 0.2500000000000000000, 0.5000000000000000000, 0.7500000000000000000, 1.000000000000000000 ),
 .UNSPECIFIED. ) ;
#42428 = CARTESIAN_POINT ( 'NONE',  ( -24.47559319016939483, -14.50700548578266513, 59.39867536442299212 ) ) ;
#42429 = CARTESIAN_POINT ( 'NONE',  ( -23.35776552503721959, -18.61638513218611735, 69.59371953224538743 ) ) ;
#42430 = EDGE_LOOP ( 'NONE', ( #21511, #28729 ) ) ;
#42431 = CARTESIAN_POINT ( 'NONE',  ( -19.90648311238531676, -10.83415612659009319, 49.52966884056655772 ) ) ;
#42432 = CARTESIAN_POINT ( 'NONE',  ( -19.64830701089596232, -21.50306318240866332, 61.99503448598593280 ) ) ;
#42433 = ADVANCED_FACE ( 'NONE', ( #46937 ), #20359, .T. ) ;
#42434 = CARTESIAN_POINT ( 'NONE',  ( 18.82590614458706924, 1.890747609047893185, 50.53028072113869484 ) ) ;
#42435 = FACE_OUTER_BOUND ( 'NONE', #23656, .T. ) ;
#42436 = CARTESIAN_POINT ( 'NONE',  ( -42.41968209070717677, -14.80920654474410547, 63.03529411764704804 ) ) ;
#42437 = CARTESIAN_POINT ( 'NONE',  ( -16.02724774380223849, -7.491242405164911133, 63.78515641179975404 ) ) ;
#42438 = DIRECTION ( 'NONE',  ( -0.9441784275685842776, 0.3294345108122634369, 1.993146885055995131E-08 ) ) ;
#42439 = DIRECTION ( 'NONE',  ( 0.9687793358424821033, -0.2479245821708680464, 0.000000000000000000 ) ) ;
#42440 = DIRECTION ( 'NONE',  ( -3.071710424422018668E-17, 6.404604876783312462E-16, 1.000000000000000000 ) ) ;
#42441 = CARTESIAN_POINT ( 'NONE',  ( -16.61784385650551954, -9.790100578890868377, 49.79778022625163203 ) ) ;
#42442 = PRODUCT_DEFINITION ( 'UNKNOWN', '', #8597, #12978 ) ;
#42443 = ORIENTED_EDGE ( 'NONE', *, *, #41113, .T. ) ;
#42444 = AXIS2_PLACEMENT_3D ( 'NONE', #17447, #36621, #28543 ) ;
#42445 = CARTESIAN_POINT ( 'NONE',  ( -15.79771479060332240, -19.20445095063907104, 49.52966884056656482 ) ) ;
#42446 = ORIENTED_EDGE ( 'NONE', *, *, #31951, .T. ) ;
#42447 = CYLINDRICAL_SURFACE ( 'NONE', #4068, 1.999999999999999112 ) ;
#42448 = DIRECTION ( 'NONE',  ( 0.000000000000000000, -1.000000000000000000, 0.000000000000000000 ) ) ;
#42449 = CARTESIAN_POINT ( 'NONE',  ( -46.47622156840087371, -14.20920654474410760, 70.13000000000000966 ) ) ;
#42450 = CARTESIAN_POINT ( 'NONE',  ( -24.32886716615087153, -16.23426984194678724, 62.60800820172418923 ) ) ;
#42451 = ORIENTED_EDGE ( 'NONE', *, *, #45204, .F. ) ;
#42452 = CARTESIAN_POINT ( 'NONE',  ( -24.80446278886646283, -15.82547754058744083, 69.63283851078359987 ) ) ;
#42453 = CIRCLE ( 'NONE', #22801, 1.000000000000000888 ) ;
#42454 = CARTESIAN_POINT ( 'NONE',  ( -24.42312040261578687, -14.69246961071934798, 59.35186350302572578 ) ) ;
#42455 = CARTESIAN_POINT ( 'NONE',  ( -24.03326526335923319, -11.37062187434330873, 66.56181149773966865 ) ) ;
#42456 = VERTEX_POINT ( 'NONE', #12950 ) ;
#42457 = CARTESIAN_POINT ( 'NONE',  ( -23.87620549320321572, -17.65941701095796645, 66.03537195726408981 ) ) ;
#42458 = VECTOR ( 'NONE', #6402, 1000.000000000000000 ) ;
#42459 = CARTESIAN_POINT ( 'NONE',  ( -12.74909871793134997, -15.13738746211001462, 49.52966884056655772 ) ) ;
#42460 = CARTESIAN_POINT ( 'NONE',  ( -12.43058792219793141, -16.43013174195301218, 52.02966884056656482 ) ) ;
#42461 = EDGE_CURVE ( 'NONE', #28350, #32762, #31197, .T. ) ;
#42462 = CARTESIAN_POINT ( 'NONE',  ( -24.86426575691346486, -14.42665972991787271, 66.33292729196470816 ) ) ;
#42463 = CYLINDRICAL_SURFACE ( 'NONE', #3172, 2.000000000000000000 ) ;
#42464 = ORIENTED_EDGE ( 'NONE', *, *, #23257, .F. ) ;
#42465 = ORIENTED_EDGE ( 'NONE', *, *, #48385, .T. ) ;
#42466 = CARTESIAN_POINT ( 'NONE',  ( -21.06159385541304374, -7.228003583438117552, 51.38655588711986155 ) ) ;
#42467 = LINE ( 'NONE', #35301, #38996 ) ;
#42468 = CARTESIAN_POINT ( 'NONE',  ( -15.69205246790211561, -7.972184624072811587, 74.49474465824219749 ) ) ;
#42469 = FACE_OUTER_BOUND ( 'NONE', #40840, .T. ) ;
#42470 = CARTESIAN_POINT ( 'NONE',  ( -20.38775279631941473, -8.467419115199003699, 66.78104087472024730 ) ) ;
#42471 = EDGE_CURVE ( 'NONE', #27235, #21456, #31978, .T. ) ;
#42472 = VECTOR ( 'NONE', #22419, 1000.000000000000000 ) ;
#42473 = DIRECTION ( 'NONE',  ( -1.000000000000000000, 0.000000000000000000, 0.000000000000000000 ) ) ;
#42474 = VECTOR ( 'NONE', #24507, 1000.000000000000000 ) ;
#42475 = EDGE_CURVE ( 'NONE', #41987, #31278, #19383, .T. ) ;
#42476 = ORIENTED_EDGE ( 'NONE', *, *, #35855, .F. ) ;
#42477 = CARTESIAN_POINT ( 'NONE',  ( -22.39908541082256832, -19.73366760896285399, 69.45952680249732225 ) ) ;
#42478 = VECTOR ( 'NONE', #600, 1000.000000000000000 ) ;
#42479 = CARTESIAN_POINT ( 'NONE',  ( -33.42409385541304800, -9.359200813967566646, 50.49621490985803263 ) ) ;
#42480 = ORIENTED_EDGE ( 'NONE', *, *, #37978, .F. ) ;
#42481 = EDGE_CURVE ( 'NONE', #48003, #22219, #10184, .T. ) ;
#42482 = CARTESIAN_POINT ( 'NONE',  ( -21.94242186726961208, -9.397052521110282441, 60.00699132926281010 ) ) ;
#42483 = DIRECTION ( 'NONE',  ( -0.9687793358424796608, 0.2479245821708770392, 7.674369900078814127E-17 ) ) ;
#42484 = ORIENTED_EDGE ( 'NONE', *, *, #37500, .T. ) ;
#42485 = FACE_OUTER_BOUND ( 'NONE', #29965, .T. ) ;
#42486 = B_SPLINE_CURVE_WITH_KNOTS ( 'NONE', 1,
 ( #33533, #37233 ),
 .UNSPECIFIED., .F., .F.,
 ( 2, 2 ),
 ( 0.000000000000000000, 1.000000000000000000 ),
 .UNSPECIFIED. ) ;
#42487 = CARTESIAN_POINT ( 'NONE',  ( -19.63034385759798894, -6.857644439848014528, 49.98602051094138687 ) ) ;
#42488 = VECTOR ( 'NONE', #43673, 1000.000000000000000 ) ;
#42489 = EDGE_CURVE ( 'NONE', #3333, #21578, #38823, .T. ) ;
#42490 = LINE ( 'NONE', #12914, #21909 ) ;
#42491 = CARTESIAN_POINT ( 'NONE',  ( -12.14425506381237341, -10.13739722748950634, 64.32914326607961186 ) ) ;
#42492 = EDGE_LOOP ( 'NONE', ( #39567, #20107, #12025, #37396, #32432 ) ) ;
#42493 = CARTESIAN_POINT ( 'NONE',  ( -10.33531725737393181, -17.10115422170377641, 57.87255955594724810 ) ) ;
#42494 = CARTESIAN_POINT ( 'NONE',  ( -11.55573786329523855, -10.21941616939416342, 71.15388509157428132 ) ) ;
#42495 = DIRECTION ( 'NONE',  ( -3.071710424422018668E-17, 6.404604876783312462E-16, 1.000000000000000000 ) ) ;
#42496 = FACE_BOUND ( 'NONE', #4159, .T. ) ;
#42497 = SHAPE_DEFINITION_REPRESENTATION ( #41739, #11272 ) ;
#42498 = CARTESIAN_POINT ( 'NONE',  ( -11.40678069298109953, -18.38590894181533031, 58.09249207256556247 ) ) ;
#42499 = CARTESIAN_POINT ( 'NONE',  ( -15.88656107989463706, -7.980151544674868980, 67.14007279409138107 ) ) ;
#42500 = CARTESIAN_POINT ( 'NONE',  ( -43.17409385541305511, -14.80920654474410547, 56.99999999999998579 ) ) ;
#42501 = ORIENTED_EDGE ( 'NONE', *, *, #41673, .T. ) ;
#42502 = CARTESIAN_POINT ( 'NONE',  ( -17.42409385541300892, -14.80920654474439502, 75.49999999999994316 ) ) ;
#42503 = ORIENTED_EDGE ( 'NONE', *, *, #2656, .F. ) ;
#42504 = CARTESIAN_POINT ( 'NONE',  ( -20.09319558404390449, -21.76479983661718265, 72.52761822131290614 ) ) ;
#42505 = CARTESIAN_POINT ( 'NONE',  ( -13.26878207226084783, -9.173970493528688763, 67.49015956650667647 ) ) ;
#42506 = EDGE_CURVE ( 'NONE', #2636, #35967, #1879, .T. ) ;
#42507 = B_SPLINE_CURVE_WITH_KNOTS ( 'NONE', 1,
 ( #3233, #19231 ),
 .UNSPECIFIED., .F., .F.,
 ( 2, 2 ),
 ( 0.000000000000000000, 1.000000000000000000 ),
 .UNSPECIFIED. ) ;
#42508 = ORIENTED_EDGE ( 'NONE', *, *, #240, .T. ) ;
#42509 = CARTESIAN_POINT ( 'NONE',  ( -20.10030204730919223, -21.76202525863913451, 72.51983304728076973 ) ) ;
#42510 = ADVANCED_FACE ( 'NONE', ( #35603 ), #31921, .T. ) ;
#42511 = CARTESIAN_POINT ( 'NONE',  ( -13.27770465421436619, -9.107456272842560097, 64.20946529204060482 ) ) ;
#42512 = VERTEX_POINT ( 'NONE', #35838 ) ;
#42513 = VERTEX_POINT ( 'NONE', #42771 ) ;
#42514 = VERTEX_POINT ( 'NONE', #31682 ) ;
#42515 = LINE ( 'NONE', #24284, #2906 ) ;
#42516 =( NAMED_UNIT ( * ) PLANE_ANGLE_UNIT ( ) SI_UNIT ( $, .RADIAN. ) );
#42517 = CARTESIAN_POINT ( 'NONE',  ( -45.92409385541306222, -14.90920654474410867, 69.25000000000000000 ) ) ;
#42518 = EDGE_CURVE ( 'NONE', #26697, #25255, #44370, .T. ) ;
#42519 = CARTESIAN_POINT ( 'NONE',  ( -17.36015840614627592, -7.359395087992972151, 67.20535029649403214 ) ) ;
#42520 = CARTESIAN_POINT ( 'NONE',  ( -10.27345486655506868, -12.71824029969684844, 64.45331411623358520 ) ) ;
#42521 = CARTESIAN_POINT ( 'NONE',  ( -16.34431749418946822, -22.18055063995905130, 61.95556900725736682 ) ) ;
#42522 = VECTOR ( 'NONE', #42709, 1000.000000000000114 ) ;
#42523 = ORIENTED_EDGE ( 'NONE', *, *, #15545, .F. ) ;
#42524 = ORIENTED_EDGE ( 'NONE', *, *, #27908, .F. ) ;
#42525 = CARTESIAN_POINT ( 'NONE',  ( -15.48261606618132546, -10.53062973237824096, 49.52966884056655772 ) ) ;
#42526 = CARTESIAN_POINT ( 'NONE',  ( -11.47484201153877237, -11.01958276889226518, 60.97886048380778590 ) ) ;
#42527 = B_SPLINE_CURVE_WITH_KNOTS ( 'NONE', 1,
 ( #5642, #20651 ),
 .UNSPECIFIED., .F., .F.,
 ( 2, 2 ),
 ( 0.000000000000000000, 1.000000000000000000 ),
 .UNSPECIFIED. ) ;
#42528 = CARTESIAN_POINT ( 'NONE',  ( -17.42409385541305511, -14.80920654474411080, 47.99999999999997868 ) ) ;
#42529 = VECTOR ( 'NONE', #664, 1000.000000000000114 ) ;
#42530 = CARTESIAN_POINT ( 'NONE',  ( -19.72840181597629439, -21.41912346864951999, 65.53774255715215702 ) ) ;
#42531 = VERTEX_POINT ( 'NONE', #43001 ) ;
#42532 =( BOUNDED_CURVE ( )  B_SPLINE_CURVE ( 3, ( #4279, #26686, #5012, #45404 ),
 .UNSPECIFIED., .F., .F. ) 
 B_SPLINE_CURVE_WITH_KNOTS ( ( 4, 4 ),
 ( 0.5000000000000000000, 0.9074455897393640669 ),
 .UNSPECIFIED. ) 
 CURVE ( )  GEOMETRIC_REPRESENTATION_ITEM ( )  RATIONAL_B_SPLINE_CURVE ( ( 0.9999999999999942268, 0.4567392136813319681, 0.3561768502900342082, 0.6983129098260947298 ) ) 
 REPRESENTATION_ITEM ( '' )  );
#42533 = CARTESIAN_POINT ( 'NONE',  ( -13.69284385650552061, -7.406986770994973490, 48.81910596585309747 ) ) ;
#42534 = EDGE_LOOP ( 'NONE', ( #20045, #17211, #34919, #41361 ) ) ;
#42535 = DIRECTION ( 'NONE',  ( -5.468526094916624094E-08, -8.832527036150760808E-06, 0.9999999999609917589 ) ) ;
#42536 = CARTESIAN_POINT ( 'NONE',  ( -16.06050865347321732, -9.480920197610746669, 53.49999999999995026 ) ) ;
#42537 = CARTESIAN_POINT ( 'NONE',  ( -12.43502688619039453, -19.72161029367247309, 65.05601852582830702 ) ) ;
#42538 = ORIENTED_EDGE ( 'NONE', *, *, #14022, .T. ) ;
#42539 = DIRECTION ( 'NONE',  ( -0.6380325334150322991, 0.7700094066334487453, 0.000000000000000000 ) ) ;
#42540 =( BOUNDED_SURFACE ( )  B_SPLINE_SURFACE ( 3, 1, ( 
 ( #42651, #46335 ),
 ( #12589, #2228 ),
 ( #39900, #43372 ),
 ( #13056, #12829 ),
 ( #28087, #35704 ),
 ( #35472, #31550 ),
 ( #47306, #39659 ) ),
 .UNSPECIFIED., .T., .F., .F. ) 
 B_SPLINE_SURFACE_WITH_KNOTS ( ( 4, 3, 4 ),
 ( 2, 2 ),
 ( 0.000000000000000000, 0.5000000000000000000, 1.000000000000000000 ),
 ( 0.000000000000000000, 1.000000000000000000 ),
 .UNSPECIFIED. ) 
 GEOMETRIC_REPRESENTATION_ITEM ( )  RATIONAL_B_SPLINE_SURFACE ( (
 ( 1.000000000000000000, 1.000000000000000000),
 ( 0.3333333333333335369, 0.3333333333333330373),
 ( 0.3333333333333335369, 0.3333333333333330373),
 ( 1.000000000000000000, 1.000000000000000000),
 ( 0.3333333333333333703, 0.3333333333333333703),
 ( 0.3333333333333333703, 0.3333333333333333703),
 ( 1.000000000000000000, 1.000000000000000000) ) ) 
 REPRESENTATION_ITEM ( '' )  SURFACE ( )  );
#42541 = EDGE_CURVE ( 'NONE', #40656, #10333, #46706, .T. ) ;
#42542 = VECTOR ( 'NONE', #17896, 1000.000000000000000 ) ;
#42543 = CARTESIAN_POINT ( 'NONE',  ( -10.40174226954351866, -17.29724918936392442, 61.34238429002267878 ) ) ;
#42544 = CARTESIAN_POINT ( 'NONE',  ( -10.85841931818429629, -17.37798394237199062, 64.91267318220633342 ) ) ;
#42545 = CARTESIAN_POINT ( 'NONE',  ( -13.00141362859484673, -9.318806420380903788, 70.85485155228010967 ) ) ;
#42546 = EDGE_CURVE ( 'NONE', #20698, #38947, #2062, .T. ) ;
#42547 = AXIS2_PLACEMENT_3D ( 'NONE', #16619, #20330, #34605 ) ;
#42548 = ORIENTED_EDGE ( 'NONE', *, *, #27944, .F. ) ;
#42549 = LINE ( 'NONE', #4623, #32036 ) ;
#42550 = CARTESIAN_POINT ( 'NONE',  ( -24.82391033454606699, -15.67355493173947956, 73.12586871779123499 ) ) ;
#42551 = CARTESIAN_POINT ( 'NONE',  ( -23.41977899678227004, -11.19648470850049904, 73.36193302072521760 ) ) ;
#42552 = ORIENTED_EDGE ( 'NONE', *, *, #23410, .F. ) ;
#42553 = CARTESIAN_POINT ( 'NONE',  ( -10.00037608677762258, -14.17511115329010707, 61.03165943758897782 ) ) ;
#42554 = CIRCLE ( 'NONE', #41737, 2.000000000000001776 ) ;
#42555 =( BOUNDED_SURFACE ( )  B_SPLINE_SURFACE ( 3, 1, ( 
 ( #38899, #20186 ),
 ( #35197, #16480 ),
 ( #31516, #12793 ),
 ( #27814, #24133 ),
 ( #7799, #14889 ),
 ( #33867, #7308 ),
 ( #22816, #26492 ) ),
 .UNSPECIFIED., .T., .F., .F. ) 
 B_SPLINE_SURFACE_WITH_KNOTS ( ( 4, 3, 4 ),
 ( 2, 2 ),
 ( 0.000000000000000000, 0.5000000000000000000, 1.000000000000000000 ),
 ( 0.000000000000000000, 1.000000000000000000 ),
 .UNSPECIFIED. ) 
 GEOMETRIC_REPRESENTATION_ITEM ( )  RATIONAL_B_SPLINE_SURFACE ( (
 ( 1.000000000000000000, 1.000000000000000000),
 ( 0.3333333333333335369, 0.3333333333333330373),
 ( 0.3333333333333335369, 0.3333333333333330373),
 ( 1.000000000000000000, 1.000000000000000000),
 ( 0.3333333333333333703, 0.3333333333333333703),
 ( 0.3333333333333333703, 0.3333333333333333703),
 ( 1.000000000000000000, 1.000000000000000000) ) ) 
 REPRESENTATION_ITEM ( '' )  SURFACE ( )  );
#42556 = ORIENTED_EDGE ( 'NONE', *, *, #9282, .F. ) ;
#42557 = CARTESIAN_POINT ( 'NONE',  ( -23.43898735819080059, -11.13148316174488528, 73.65633489482847551 ) ) ;
#42558 = PRODUCT ( 'Speed Governor Worm Gear Train', 'Speed Governor Worm Gear Train', '', ( #26982 ) ) ;
#42559 = CARTESIAN_POINT ( 'NONE',  ( -21.99178500617274779, -9.439039195359631762, 59.72171213140594404 ) ) ;
#42560 = ORIENTED_EDGE ( 'NONE', *, *, #28952, .F. ) ;
#42561 = CARTESIAN_POINT ( 'NONE',  ( -16.72330486927764426, -21.83230113783351101, 61.91134987066439521 ) ) ;
#42562 = FACE_OUTER_BOUND ( 'NONE', #37173, .T. ) ;
#42563 = PLANE ( 'NONE',  #39911 ) ;
#42564 = LINE ( 'NONE', #31945, #1493 ) ;
#42565 = ORIENTED_EDGE ( 'NONE', *, *, #31932, .T. ) ;
#42566 = CARTESIAN_POINT ( 'NONE',  ( -23.77562434277295367, -17.86939608417919345, 59.01850491586762359 ) ) ;
#42567 = AXIS2_PLACEMENT_3D ( 'NONE', #543, #38193, #4475 ) ;
#42568 = DIRECTION ( 'NONE',  ( -0.8402231219892289937, 0.5322911103758086737, 0.1033986416233890204 ) ) ;
#42569 = CARTESIAN_POINT ( 'NONE',  ( -17.84735443592641602, -7.371153788697909270, 60.19565345827741965 ) ) ;
#42571 = ADVANCED_FACE ( 'NONE', ( #19062 ), #11928, .T. ) ;
#42570 = FACE_OUTER_BOUND ( 'NONE', #21756, .T. ) ;
#42572 = ORIENTED_EDGE ( 'NONE', *, *, #20848, .F. ) ;
#42573 = CARTESIAN_POINT ( 'NONE',  ( -10.37600963001940713, -14.53000751884195374, 64.59623758275894545 ) ) ;
#42574 = ADVANCED_FACE ( 'NONE', ( #38498 ), #3265, .T. ) ;
#42575 = LINE ( 'NONE', #42803, #43220 ) ;
#42576 = EDGE_CURVE ( 'NONE', #25499, #20428, #19546, .T. ) ;
#42577 = ADVANCED_FACE ( 'NONE', ( #16076 ), #45186, .F. ) ;
#42578 = EDGE_CURVE ( 'NONE', #33105, #19220, #31608, .T. ) ;
#42580 = ORIENTED_EDGE ( 'NONE', *, *, #7105, .T. ) ;
#42579 = VECTOR ( 'NONE', #26007, 1000.000000000000227 ) ;
#42581 = ORIENTED_EDGE ( 'NONE', *, *, #1273, .F. ) ;
#42582 = CARTESIAN_POINT ( 'NONE',  ( -19.34161870936485883, -22.00820632818791012, 58.67507381970625602 ) ) ;
#42583 = CARTESIAN_POINT ( 'NONE',  ( -13.12790236870489302, -8.721809449924828428, 64.09601920791236296 ) ) ;
#42584 = CARTESIAN_POINT ( 'NONE',  ( -16.36862302632751209, -10.24310716135927812, 49.52966884056655772 ) ) ;
#42585 = CARTESIAN_POINT ( 'NONE',  ( -21.84909385650551528, -8.104110260919577868, 48.81699501597546487 ) ) ;
#42586 = CARTESIAN_POINT ( 'NONE',  ( -24.45714095472541771, -14.31630891555219165, 69.66747352629326429 ) ) ;
#42587 = FACE_OUTER_BOUND ( 'NONE', #33778, .T. ) ;
#42588 = CARTESIAN_POINT ( 'NONE',  ( -23.28150713458464338, -18.64225386619112257, 69.59372035755308161 ) ) ;
#42589 = LINE ( 'NONE', #8851, #8013 ) ;
#42590 = ORIENTED_EDGE ( 'NONE', *, *, #17498, .F. ) ;
#42591 = VERTEX_POINT ( 'NONE', #15345 ) ;
#42593 = CARTESIAN_POINT ( 'NONE',  ( -22.80481760130283675, -10.24931098477615166, 70.42667203218238114 ) ) ;
#42592 = AXIS2_PLACEMENT_3D ( 'NONE', #31252, #15730, #45807 ) ;
#42594 = AXIS2_PLACEMENT_3D ( 'NONE', #8460, #42691, #12390 ) ;
#42595 = CARTESIAN_POINT ( 'NONE',  ( -23.68216640822461372, -11.66929755891756670, 66.61141575710782092 ) ) ;
#42596 = DIRECTION ( 'NONE',  ( -3.071710424422018668E-17, 6.404604876783312462E-16, 1.000000000000000000 ) ) ;
#42597 = CARTESIAN_POINT ( 'NONE',  ( -12.50766613833179974, -19.86205114983803810, 64.86674886870797252 ) ) ;
#42598 = VECTOR ( 'NONE', #37728, 1000.000000000000114 ) ;
#42599 = ORIENTED_EDGE ( 'NONE', *, *, #29935, .T. ) ;
#42600 = EDGE_CURVE ( 'NONE', #47353, #17705, #15182, .T. ) ;
#42601 = CARTESIAN_POINT ( 'NONE',  ( -17.42409385541306222, -17.30920654474411080, 82.49999999999998579 ) ) ;
#42602 = CARTESIAN_POINT ( 'NONE',  ( -21.68499379980493913, -9.192514338196572155, 66.96149992326067490 ) ) ;
#42603 = CARTESIAN_POINT ( 'NONE',  ( -36.42409385541304800, -8.109206544743658540, 50.50000000000030553 ) ) ;
#42604 = CARTESIAN_POINT ( 'NONE',  ( -24.16424020987968646, -16.88652737071335252, 72.76847378359866525 ) ) ;
#42605 = AXIS2_PLACEMENT_3D ( 'NONE', #43195, #35057, #35303 ) ;
#42606 = ORIENTED_EDGE ( 'NONE', *, *, #30513, .T. ) ;
#42607 = CARTESIAN_POINT ( 'NONE',  ( -24.84240844029834250, -14.11474841844398043, 69.76619977786306492 ) ) ;
#42608 = B_SPLINE_CURVE_WITH_KNOTS ( 'NONE', 3,
 ( #14733, #15482, #26346, #48497, #3697, #29805, #41863, #34449, #739, #15733 ),
 .UNSPECIFIED., .F., .F.,
 ( 4, 2, 2, 2, 4 ),
 ( 0.1272669073657639871, 0.2522669073462675549, 0.3772669073267711504, 0.5022669073072747459, 0.6272669072877783414 ),
 .UNSPECIFIED. ) ;
#42609 = ORIENTED_EDGE ( 'NONE', *, *, #47583, .T. ) ;
#42610 = CARTESIAN_POINT ( 'NONE',  ( -50.42409385541305511, -14.80920654474410725, 74.99999999999998579 ) ) ;
#42611 = CARTESIAN_POINT ( 'NONE',  ( -22.10541318350566442, -20.01527617504624601, 65.77591942924708235 ) ) ;
#42612 = ORIENTED_EDGE ( 'NONE', *, *, #9134, .F. ) ;
#42613 = FACE_OUTER_BOUND ( 'NONE', #48218, .T. ) ;
#42614 = ORIENTED_EDGE ( 'NONE', *, *, #5015, .F. ) ;
#42615 = CARTESIAN_POINT ( 'NONE',  ( -50.42609385541305755, -14.90920654474415841, 62.02941176470587692 ) ) ;
#42617 = CARTESIAN_POINT ( 'NONE',  ( -10.42411290126982060, -14.77598683159526161, 71.34285171099139689 ) ) ;
#42616 = CIRCLE ( 'NONE', #12723, 5.249999999999998224 ) ;
#42618 = ORIENTED_EDGE ( 'NONE', *, *, #41120, .T. ) ;
#42619 = CARTESIAN_POINT ( 'NONE',  ( -19.41474841345058522, -21.52018966427049307, 62.29503644830997189 ) ) ;
#42620 = CARTESIAN_POINT ( 'NONE',  ( -14.35043204381087101, -18.34698626059704551, 49.52966884056656482 ) ) ;
#42621 = CARTESIAN_POINT ( 'NONE',  ( -16.48034385650551670, -6.424090610841176385, 49.80797279389978627 ) ) ;
#42622 = AXIS2_PLACEMENT_3D ( 'NONE', #32097, #29124, #13115 ) ;
#42623 = CARTESIAN_POINT ( 'NONE',  ( -23.19916440516392697, -19.59445054535707698, 53.49999999999994316 ) ) ;
#42624 = CARTESIAN_POINT ( 'NONE',  ( -24.07098297129566333, -12.61366397057463118, 73.54225587970537958 ) ) ;
#42625 = CARTESIAN_POINT ( 'NONE',  ( -22.25094433143537387, -9.134348456342106459, 59.87171212369386097 ) ) ;
#42626 = ORIENTED_EDGE ( 'NONE', *, *, #28090, .F. ) ;
#42627 = CYLINDRICAL_SURFACE ( 'NONE', #12911, 0.1500000000000073774 ) ;
#42628 = DIRECTION ( 'NONE',  ( 0.000000000000000000, 0.000000000000000000, 1.000000000000000000 ) ) ;
#42629 = CARTESIAN_POINT ( 'NONE',  ( -11.63496427220788121, -10.77921706672702129, 74.43884596448377522 ) ) ;
#42630 = CARTESIAN_POINT ( 'NONE',  ( 18.62590614458706995, 1.890747609047893185, 50.53028072113869484 ) ) ;
#42631 = CARTESIAN_POINT ( 'NONE',  ( -24.44055745662519641, -14.11932379769929113, 73.13743607903229815 ) ) ;
#42632 = ADVANCED_FACE ( 'NONE', ( #4778 ), #30163, .T. ) ;
#42633 = ADVANCED_FACE ( 'NONE', ( #34806 ), #25270, .T. ) ;
#42634 = ORIENTED_EDGE ( 'NONE', *, *, #21730, .F. ) ;
#42635 = EDGE_LOOP ( 'NONE', ( #22311, #20423, #14209, #12584 ) ) ;
#42636 = CARTESIAN_POINT ( 'NONE',  ( -10.42334091404133645, -15.64104667191196540, 61.33789045260129313 ) ) ;
#42637 = CARTESIAN_POINT ( 'NONE',  ( -17.92193097897699872, -21.84160713959417421, 62.17535923543129428 ) ) ;
#42638 = ORIENTED_EDGE ( 'NONE', *, *, #48466, .F. ) ;
#42639 = CARTESIAN_POINT ( 'NONE',  ( -15.54840433177174397, -8.005034934413657766, 67.29574103338339341 ) ) ;
#42640 = CYLINDRICAL_SURFACE ( 'NONE', #30303, 0.1500000000000026590 ) ;
#42641 = CARTESIAN_POINT ( 'NONE',  ( -10.29167786474582869, -12.65701390312483809, 64.37561959354262342 ) ) ;
#42642 = CARTESIAN_POINT ( 'NONE',  ( -13.43773910423563400, -20.62433115109003268, 58.33177939114180788 ) ) ;
#42643 = CARTESIAN_POINT ( 'NONE',  ( -42.67115267894247665, -14.90920654474414775, 61.02352941176469869 ) ) ;
#42644 = DIRECTION ( 'NONE',  ( -0.000000000000000000, -1.000000000000000000, -0.000000000000000000 ) ) ;
#42645 = VERTEX_POINT ( 'NONE', #46867 ) ;
#42646 = ADVANCED_FACE ( 'NONE', ( #35533 ), #39960, .T. ) ;
#42647 = ADVANCED_FACE ( 'NONE', ( #5514 ), #47109, .T. ) ;
#42648 = B_SPLINE_CURVE_WITH_KNOTS ( 'NONE', 1,
 ( #45012, #11257 ),
 .UNSPECIFIED., .F., .F.,
 ( 2, 2 ),
 ( 0.000000000000000000, 1.000000000000000000 ),
 .UNSPECIFIED. ) ;
#42649 = CARTESIAN_POINT ( 'NONE',  ( -17.58219478024370730, -20.05682544264154288, 49.52966884056656482 ) ) ;
#42650 = LINE ( 'NONE', #1991, #7484 ) ;
#42651 = CARTESIAN_POINT ( 'NONE',  ( -12.76547314785493192, -9.517330534081262172, 74.60450883341005124 ) ) ;
#42652 = CARTESIAN_POINT ( 'NONE',  ( -21.43549133165072362, -9.072522135161841916, 70.41667131949601810 ) ) ;
#42653 = ORIENTED_EDGE ( 'NONE', *, *, #7099, .T. ) ;
#42654 = ORIENTED_EDGE ( 'NONE', *, *, #47634, .F. ) ;
#42655 = CARTESIAN_POINT ( 'NONE',  ( -21.79284385650551314, -7.406986770994973490, 48.81910596585309747 ) ) ;
#42656 = ORIENTED_EDGE ( 'NONE', *, *, #33718, .T. ) ;
#42657 = EDGE_CURVE ( 'NONE', #10249, #2125, #28052, .T. ) ;
#42658 = CARTESIAN_POINT ( 'NONE',  ( -11.96606040034933471, -9.738391814011444936, 60.75192256564785254 ) ) ;
#42659 = CARTESIAN_POINT ( 'NONE',  ( -24.10581758648508099, -12.72203489083164740, 70.07242970654482406 ) ) ;
#42660 = ORIENTED_EDGE ( 'NONE', *, *, #1013, .T. ) ;
#42661 = CARTESIAN_POINT ( 'NONE',  ( -20.92409385541305511, -10.10920654474410618, 80.49999999999998579 ) ) ;
#42662 = CARTESIAN_POINT ( 'NONE',  ( -22.69190674372240935, -10.11825871574920654, 73.78161098756908132 ) ) ;
#42663 = ORIENTED_EDGE ( 'NONE', *, *, #4722, .F. ) ;
#42664 = CARTESIAN_POINT ( 'NONE',  ( -10.64068610965668960, -17.88985431858020547, 71.72751587850088129 ) ) ;
#42665 = CARTESIAN_POINT ( 'NONE',  ( -23.78474288321120511, -17.73496378845812771, 62.54531179860746448 ) ) ;
#42666 = B_SPLINE_CURVE_WITH_KNOTS ( 'NONE', 1,
 ( #2261, #6202 ),
 .UNSPECIFIED., .F., .F.,
 ( 2, 2 ),
 ( 0.000000000000000000, 1.000000000000000000 ),
 .UNSPECIFIED. ) ;
#42667 = VERTEX_POINT ( 'NONE', #9450 ) ;
#42668 = CARTESIAN_POINT ( 'NONE',  ( -19.90433039125390025, -21.83431899736824988, 69.04987161812600505 ) ) ;
#42669 = CARTESIAN_POINT ( 'NONE',  ( -10.60399421354195404, -13.23188019733764520, 71.50828540008092205 ) ) ;
#42670 = ORIENTED_EDGE ( 'NONE', *, *, #22164, .F. ) ;
#42671 = FACE_OUTER_BOUND ( 'NONE', #36167, .T. ) ;
#42672 = CARTESIAN_POINT ( 'NONE',  ( -18.14263071100308977, -21.82253481906295178, 65.64532146769309406 ) ) ;
#42673 = ORIENTED_EDGE ( 'NONE', *, *, #12330, .T. ) ;
#42674 = CARTESIAN_POINT ( 'NONE',  ( -17.84735443592641602, -7.371153788697909270, 60.19565345827741965 ) ) ;
#42675 = CARTESIAN_POINT ( 'NONE',  ( -14.66790711817407278, -21.29843871104708342, 58.18089935161520287 ) ) ;
#42676 =( BOUNDED_CURVE ( )  B_SPLINE_CURVE ( 3, ( #32197, #32894, #36825, #47689 ),
 .UNSPECIFIED., .F., .F. ) 
 B_SPLINE_CURVE_WITH_KNOTS ( ( 4, 4 ),
 ( 0.4074455897393675086, 0.5000000000000000000 ),
 .UNSPECIFIED. ) 
 CURVE ( )  GEOMETRIC_REPRESENTATION_ITEM ( )  RATIONAL_B_SPLINE_CURVE ( ( 0.6983129098261046108, 0.7760317562607000896, 0.8765941196519961842, 0.9999999999999872324 ) ) 
 REPRESENTATION_ITEM ( '' )  );
#42677 = CARTESIAN_POINT ( 'NONE',  ( -14.58539460706017543, -21.69719740599226654, 58.36606672081529013 ) ) ;
#42678 = CARTESIAN_POINT ( 'NONE',  ( -24.17899278864585355, -11.66673636667039027, 59.66731167108189737 ) ) ;
#42679 = CARTESIAN_POINT ( 'NONE',  ( -24.36818545036879868, -13.92577592638252604, 73.34944830282202588 ) ) ;
#42680 = ORIENTED_EDGE ( 'NONE', *, *, #4920, .F. ) ;
#42681 = CARTESIAN_POINT ( 'NONE',  ( -22.37985709289073455, -19.82347726015160205, 69.17417989525732480 ) ) ;
#42682 = DIRECTION ( 'NONE',  ( -0.000000000000000000, -1.000000000000000000, 0.000000000000000000 ) ) ;
#42683 = CARTESIAN_POINT ( 'NONE',  ( -46.92409385541305511, -14.80920654474410547, 61.49999999999999289 ) ) ;
#42684 = CARTESIAN_POINT ( 'NONE',  ( -24.46812100523181144, -14.51191712007779699, 66.19764790277996269 ) ) ;
#42685 = CARTESIAN_POINT ( 'NONE',  ( -16.67409385650551812, -9.792211528768504536, 50.49490371617623197 ) ) ;
#42686 = EDGE_CURVE ( 'NONE', #7144, #13624, #43672, .T. ) ;
#42687 = ORIENTED_EDGE ( 'NONE', *, *, #36374, .T. ) ;
#42688 = DIRECTION ( 'NONE',  ( 0.000000000000000000, 0.000000000000000000, 1.000000000000000000 ) ) ;
#42689 = CARTESIAN_POINT ( 'NONE',  ( -12.23220189640646538, -19.57856266540686718, 58.07682373937821296 ) ) ;
#42690 = VERTEX_POINT ( 'NONE', #43175 ) ;
#42691 = DIRECTION ( 'NONE',  ( -3.071710424422018668E-17, 6.404604876783312462E-16, 1.000000000000000000 ) ) ;
#42692 = CARTESIAN_POINT ( 'NONE',  ( -14.95029678367283665, -21.83651174838278664, 65.20622428847848084 ) ) ;
#42693 = CARTESIAN_POINT ( 'NONE',  ( -21.06713455244400635, -20.85430592508659586, 72.66879606033384675 ) ) ;
#42694 = PLANE ( 'NONE',  #21903 ) ;
#42695 = CARTESIAN_POINT ( 'NONE',  ( -16.99688961111671404, -22.24707068558670642, 72.28730467040716690 ) ) ;
#42696 = VERTEX_POINT ( 'NONE', #28403 ) ;
#42697 = DIRECTION ( 'NONE',  ( 1.000000000000000000, -4.164305804376849172E-17, 1.614929280266638808E-16 ) ) ;
#42698 =( BOUNDED_CURVE ( )  B_SPLINE_CURVE ( 3, ( #35049, #16575, #20042, #27675 ),
 .UNSPECIFIED., .F., .F. ) 
 B_SPLINE_CURVE_WITH_KNOTS ( ( 4, 4 ),
 ( 4.712388980384689674, 4.921828490624009511 ),
 .UNSPECIFIED. ) 
 CURVE ( )  GEOMETRIC_REPRESENTATION_ITEM ( )  RATIONAL_B_SPLINE_CURVE ( ( 1.000000000000000000, 0.9963479302455154896, 0.9963479302455154896, 1.000000000000000000 ) ) 
 REPRESENTATION_ITEM ( '' )  );
#42699 = FACE_OUTER_BOUND ( 'NONE', #27501, .T. ) ;
#42700 = ADVANCED_FACE ( 'NONE', ( #42699 ), #20531, .T. ) ;
#42701 = CARTESIAN_POINT ( 'NONE',  ( -11.96194199484143539, -9.742791280557115741, 60.60272182217008208 ) ) ;
#42702 = B_SPLINE_CURVE_WITH_KNOTS ( 'NONE', 3,
 ( #30015, #11294, #21878, #10796, #25815, #29024, #18172, #14222, #3914, #3406 ),
 .UNSPECIFIED., .F., .F.,
 ( 4, 2, 2, 2, 4 ),
 ( 0.1272669073658190264, 0.2522669073463195133, 0.3772669073268200002, 0.5022669073073204871, 0.6272669072878209739 ),
 .UNSPECIFIED. ) ;
#42703 = VERTEX_POINT ( 'NONE', #16317 ) ;
#42704 = LINE ( 'NONE', #5030, #25871 ) ;
#42705 = EDGE_CURVE ( 'NONE', #23794, #18637, #9925, .T. ) ;
#42706 = EDGE_CURVE ( 'NONE', #25610, #41313, #30318, .T. ) ;
#42707 = CARTESIAN_POINT ( 'NONE',  ( -23.97043363090852353, -12.17094895590152426, 59.62668449103946955 ) ) ;
#42708 = CARTESIAN_POINT ( 'NONE',  ( -33.52409385541305653, -6.359206544744109735, 49.44999999999998863 ) ) ;
#42709 = DIRECTION ( 'NONE',  ( 0.05202058437830280740, -0.9986460127597464043, 1.657953767687799580E-08 ) ) ;
#42710 = CARTESIAN_POINT ( 'NONE',  ( -45.85858821786030859, -14.20920654474410760, 71.05212771298751306 ) ) ;
#42711 = ORIENTED_EDGE ( 'NONE', *, *, #14804, .F. ) ;
#42712 = ORIENTED_EDGE ( 'NONE', *, *, #3759, .F. ) ;
#42713 = CARTESIAN_POINT ( 'NONE',  ( -20.33034385541304800, -6.857644439848013640, 49.98602051094139398 ) ) ;
#42714 = CARTESIAN_POINT ( 'NONE',  ( -16.93941734680482725, -7.775588144984237005, 74.24546186738449194 ) ) ;
#42715 = AXIS2_PLACEMENT_3D ( 'NONE', #15613, #11950, #41742 ) ;
#42716 = CARTESIAN_POINT ( 'NONE',  ( -17.76701911439868198, -7.767511358351252504, 60.38060761803046006 ) ) ;
#42717 = CARTESIAN_POINT ( 'NONE',  ( -22.91217743940941176, -10.46398633218385399, 59.71089353488221718 ) ) ;
#42718 = CARTESIAN_POINT ( 'NONE',  ( -13.90804716676048258, -20.86209139562971160, 68.45625137333186672 ) ) ;
#42719 = ORIENTED_EDGE ( 'NONE', *, *, #47198, .T. ) ;
#42720 = CARTESIAN_POINT ( 'NONE',  ( -18.69700338743018264, -7.871300468185871146, 66.90071501288184663 ) ) ;
#42721 = CARTESIAN_POINT ( 'NONE',  ( -24.10335570753463230, -17.07466383872621307, 69.29851186845237976 ) ) ;
#42722 = ORIENTED_EDGE ( 'NONE', *, *, #26807, .T. ) ;
#42723 = CARTESIAN_POINT ( 'NONE',  ( -23.71561414012218094, -17.99693426085591952, 59.41867086777731544 ) ) ;
#42724 = DIRECTION ( 'NONE',  ( 2.866981220435666553E-17, -1.000000000000000000, -1.190614954331866791E-16 ) ) ;
#42725 = VERTEX_POINT ( 'NONE', #24943 ) ;
#42726 = CARTESIAN_POINT ( 'NONE',  ( -13.36456289509512096, -21.05617294863179723, 61.69363177936434539 ) ) ;
#42727 = CARTESIAN_POINT ( 'NONE',  ( -10.40245588357037043, -14.17414831712846990, 61.20349182037644198 ) ) ;
#42728 = ORIENTED_EDGE ( 'NONE', *, *, #649, .T. ) ;
#42729 = CARTESIAN_POINT ( 'NONE',  ( -12.00971705810820467, -9.691755786776280246, 60.67422651510300113 ) ) ;
#42730 = CYLINDRICAL_SURFACE ( 'NONE', #38316, 2.000000000000001332 ) ;
#42731 = EDGE_CURVE ( 'NONE', #13213, #19324, #13352, .T. ) ;
#42732 = CARTESIAN_POINT ( 'NONE',  ( -15.09544305450467938, -21.46351983957133669, 65.40596681500470311 ) ) ;
#42733 = CARTESIAN_POINT ( 'NONE',  ( -22.57359528252793623, -19.55088050636924990, 72.71688684016393722 ) ) ;
#42734 = VERTEX_POINT ( 'NONE', #43429 ) ;
#42735 = CARTESIAN_POINT ( 'NONE',  ( -17.82409385541306079, -14.80920654474411080, 75.49999999999998579 ) ) ;
#42736 = CARTESIAN_POINT ( 'NONE',  ( -20.83870870799843900, -21.43061845379169839, 58.74500915750943619 ) ) ;
#42737 = CARTESIAN_POINT ( 'NONE',  ( -16.60134452727454146, -19.99433755013348701, 50.77966884056656482 ) ) ;
#42738 = CARTESIAN_POINT ( 'NONE',  ( -11.17855889551124982, -18.87086522978130532, 64.86211687253867808 ) ) ;
#42739 = CARTESIAN_POINT ( 'NONE',  ( -17.75227477277866939, -19.48420168222600068, 49.52966884056656482 ) ) ;
#42740 = CARTESIAN_POINT ( 'NONE',  ( -17.06206538396918404, -7.760525543569854356, 67.17606901500077754 ) ) ;
#42741 = AXIS2_PLACEMENT_3D ( 'NONE', #2855, #22310, #17862 ) ;
#42742 = CARTESIAN_POINT ( 'NONE',  ( -50.42509385541305988, -8.109206544744111511, 50.49999999999998579 ) ) ;
#42743 = VERTEX_POINT ( 'NONE', #46389 ) ;
#42744 = CARTESIAN_POINT ( 'NONE',  ( -10.67379822573247949, -12.95623351948692381, 64.37722118855614895 ) ) ;
#42745 = ORIENTED_EDGE ( 'NONE', *, *, #10036, .F. ) ;
#42746 = CARTESIAN_POINT ( 'NONE',  ( -11.15046514442954972, -11.70398196082027376, 67.69152635070139468 ) ) ;
#42747 = CARTESIAN_POINT ( 'NONE',  ( -22.90877211956182435, -10.45951156430351503, 63.07186031186947872 ) ) ;
#42748 = ORIENTED_EDGE ( 'NONE', *, *, #38654, .F. ) ;
#42749 = CARTESIAN_POINT ( 'NONE',  ( -20.52762626839951210, -8.534807245883811788, 63.61121513079540080 ) ) ;
#42750 = FACE_BOUND ( 'NONE', #6674, .T. ) ;
#42751 = EDGE_LOOP ( 'NONE', ( #26124, #21570, #42322, #34700, #24674 ) ) ;
#42752 = ORIENTED_EDGE ( 'NONE', *, *, #37163, .T. ) ;
#42753 = VERTEX_POINT ( 'NONE', #16568 ) ;
#42754 = EDGE_CURVE ( 'NONE', #41701, #45322, #31998, .T. ) ;
#42755 = CARTESIAN_POINT ( 'NONE',  ( -10.38377074815290868, -15.30802594933397920, 61.18222038349547631 ) ) ;
#42756 = EDGE_CURVE ( 'NONE', #2663, #6207, #14873, .T. ) ;
#42757 = CARTESIAN_POINT ( 'NONE',  ( -16.36784385759798965, -9.357632978295836068, 49.97845033065684106 ) ) ;
#42758 = CARTESIAN_POINT ( 'NONE',  ( -22.81815734205171964, -10.26415160585916020, 70.10358578328691692 ) ) ;
#42759 = CARTESIAN_POINT ( 'NONE',  ( -22.48114071483173149, -19.64927648862363796, 72.94400547034429394 ) ) ;
#42760 = LINE ( 'NONE', #9030, #834 ) ;
#42761 = EDGE_LOOP ( 'NONE', ( #34174, #3289, #14748, #43770 ) ) ;
#42762 = ORIENTED_EDGE ( 'NONE', *, *, #48552, .F. ) ;
#42763 = EDGE_CURVE ( 'NONE', #32365, #733, #37497, .T. ) ;
#42764 = CARTESIAN_POINT ( 'NONE',  ( -23.06159385650551386, -9.295667164867525756, 49.30633214617472504 ) ) ;
#42765 = CARTESIAN_POINT ( 'NONE',  ( -21.59804090337381410, -20.98026344205569771, 72.70941702861115630 ) ) ;
#42766 = CARTESIAN_POINT ( 'NONE',  ( -24.87406538417882729, -14.83278061336772069, 59.44289023857400167 ) ) ;
#42767 = DIRECTION ( 'NONE',  ( -6.059369603295153624E-06, 3.309764060044371102E-06, 0.9999999999761648439 ) ) ;
#42768 = EDGE_CURVE ( 'NONE', #38822, #40490, #38263, .T. ) ;
#42769 = CARTESIAN_POINT ( 'NONE',  ( -22.04909385650551457, -8.104110260919577868, 48.81699501597546487 ) ) ;
#42770 = ORIENTED_EDGE ( 'NONE', *, *, #33839, .T. ) ;
#42771 = CARTESIAN_POINT ( 'NONE',  ( -22.67171275331017810, -14.65110561991362559, 49.52966884056655772 ) ) ;
#42772 = DIRECTION ( 'NONE',  ( -1.000000000000000000, -0.000000000000000000, -0.000000000000000000 ) ) ;
#42773 = VECTOR ( 'NONE', #22817, 1000.000000000000000 ) ;
#42774 = CARTESIAN_POINT ( 'NONE',  ( -41.28806444364835215, -14.80920654474426357, 72.08823529411763786 ) ) ;
#42775 = ORIENTED_EDGE ( 'NONE', *, *, #13124, .F. ) ;
#42776 = CARTESIAN_POINT ( 'NONE',  ( -12.68532267716109985, -9.060482739934947460, 71.03420753023118550 ) ) ;
#42777 = FACE_OUTER_BOUND ( 'NONE', #17997, .T. ) ;
#42778 = B_SPLINE_CURVE_WITH_KNOTS ( 'NONE', 1,
 ( #4085, #22532 ),
 .UNSPECIFIED., .F., .F.,
 ( 2, 2 ),
 ( 0.000000000000000000, 1.000000000000000000 ),
 .UNSPECIFIED. ) ;
#42779 = CARTESIAN_POINT ( 'NONE',  ( -22.06352374043166265, -8.980015506435984562, 63.37649162950052784 ) ) ;
#42780 = CARTESIAN_POINT ( 'NONE',  ( -14.40111994560675690, -7.999901138345907547, 63.95012236324505750 ) ) ;
#42781 = VERTEX_POINT ( 'NONE', #39231 ) ;
#42782 = CARTESIAN_POINT ( 'NONE',  ( -23.41977742916776251, -11.19648202114625235, 73.66193302070908544 ) ) ;
#42783 = EDGE_CURVE ( 'NONE', #46985, #8086, #28809, .T. ) ;
#42784 = CARTESIAN_POINT ( 'NONE',  ( -12.39907312731801525, -20.30942516702692657, 68.44319146479406868 ) ) ;
#42785 = ORIENTED_EDGE ( 'NONE', *, *, #2373, .T. ) ;
#42786 = CARTESIAN_POINT ( 'NONE',  ( -24.72409385541305582, -14.80920654474428488, 74.99999999999998579 ) ) ;
#42787 = ORIENTED_EDGE ( 'NONE', *, *, #6461, .T. ) ;
#42788 = CARTESIAN_POINT ( 'NONE',  ( -9.974824918456654643, -14.70410907813601220, 71.42759073425887095 ) ) ;
#42789 = CARTESIAN_POINT ( 'NONE',  ( -9.975093131592752016, -14.93635113986534257, 74.98274190467411415 ) ) ;
#42790 = EDGE_LOOP ( 'NONE', ( #23469, #27312, #2311, #22772, #26633 ) ) ;
#42791 = CARTESIAN_POINT ( 'NONE',  ( -24.72409385541305582, -14.80920654474428488, 74.09999999999998010 ) ) ;
#42792 = CARTESIAN_POINT ( 'NONE',  ( -19.97164353606484255, -21.81018995992316079, 69.11977899231902711 ) ) ;
#42793 = CARTESIAN_POINT ( 'NONE',  ( -14.21162209046732805, -8.087226629722726656, 67.39828596402958283 ) ) ;
#42794 = CARTESIAN_POINT ( 'NONE',  ( -9.975583804105555785, -14.65598652642324673, 71.44287259100559595 ) ) ;
#42795 = ORIENTED_EDGE ( 'NONE', *, *, #13139, .T. ) ;
#42796 = CARTESIAN_POINT ( 'NONE',  ( -17.42409385541300892, -14.80920654474439679, 47.99999999999994316 ) ) ;
#42797 = CARTESIAN_POINT ( 'NONE',  ( -20.36919052476639180, -21.22336078664356407, 58.78908032405391992 ) ) ;
#42798 = CARTESIAN_POINT ( 'NONE',  ( -10.08052694344373812, -16.06451652471636748, 68.09272548404199199 ) ) ;
#42799 = EDGE_LOOP ( 'NONE', ( #7320, #4478, #32889, #17045 ) ) ;
#42800 = EDGE_CURVE ( 'NONE', #11228, #19229, #26659, .T. ) ;
#42801 = CARTESIAN_POINT ( 'NONE',  ( -24.61605457543312525, -12.86511826566283290, 66.41751344402152313 ) ) ;
#42802 = VECTOR ( 'NONE', #47885, 1000.000000000000000 ) ;
#42803 = CARTESIAN_POINT ( 'NONE',  ( -8.621879165042305004, -16.10189953769286575, 53.49999999999995026 ) ) ;
#42804 = AXIS2_PLACEMENT_3D ( 'NONE', #23668, #9621, #43593 ) ;
#42805 = ORIENTED_EDGE ( 'NONE', *, *, #33172, .F. ) ;
#42806 = ORIENTED_EDGE ( 'NONE', *, *, #13746, .F. ) ;
#42807 = CARTESIAN_POINT ( 'NONE',  ( -23.44680839214612789, -18.37680329023430303, 72.77870615285404199 ) ) ;
#42808 = FACE_OUTER_BOUND ( 'NONE', #16357, .T. ) ;
#42809 = CARTESIAN_POINT ( 'NONE',  ( -10.99575410903449679, -18.57485570963264010, 57.85068653066719691 ) ) ;
#42810 = CARTESIAN_POINT ( 'NONE',  ( -20.10534385650551670, -8.801233750844183135, 48.81488406609782515 ) ) ;
#42811 = CARTESIAN_POINT ( 'NONE',  ( -24.45563495707309087, -14.29732410816288279, 69.65835052054990228 ) ) ;
#42812 =( BOUNDED_CURVE ( )  B_SPLINE_CURVE ( 3, ( #16864, #21557, #43241, #17103 ),
 .UNSPECIFIED., .F., .F. ) 
 B_SPLINE_CURVE_WITH_KNOTS ( ( 4, 4 ),
 ( 0.000000000000000000, 0.4074455897393707282 ),
 .UNSPECIFIED. ) 
 CURVE ( )  GEOMETRIC_REPRESENTATION_ITEM ( )  RATIONAL_B_SPLINE_CURVE ( ( 1.000000000000000000, 0.4567392136813279713, 0.3561768502900288236, 0.6983129098261023904 ) ) 
 REPRESENTATION_ITEM ( '' )  );
#42813 = LINE ( 'NONE', #12279, #40876 ) ;
#42814 = CARTESIAN_POINT ( 'NONE',  ( -23.22139416215049579, -18.73524918430105046, 69.40445189021075123 ) ) ;
#42815 = FACE_OUTER_BOUND ( 'NONE', #37676, .T. ) ;
#42816 = EDGE_LOOP ( 'NONE', ( #135, #43064, #41308, #23638 ) ) ;
#42817 = VERTEX_POINT ( 'NONE', #16708 ) ;
#42818 = EDGE_CURVE ( 'NONE', #4674, #37124, #47749, .T. ) ;
#42819 = CARTESIAN_POINT ( 'NONE',  ( -12.38751766673716581, -20.29879047900762501, 68.53646224134315901 ) ) ;
#42820 = LINE ( 'NONE', #28031, #18918 ) ;
#42821 = CARTESIAN_POINT ( 'NONE',  ( -13.29676203468008033, -8.606078807347360637, 57.08312357396523140 ) ) ;
#42822 = ADVANCED_FACE ( 'NONE', ( #42106 ), #23155, .F. ) ;
#42823 = CARTESIAN_POINT ( 'NONE',  ( -20.84966316371748363, -20.97445663613623523, 58.52986464729110594 ) ) ;
#42824 =( BOUNDED_CURVE ( )  B_SPLINE_CURVE ( 3, ( #12770, #27784, #9088, #24099 ),
 .UNSPECIFIED., .F., .F. ) 
 B_SPLINE_CURVE_WITH_KNOTS ( ( 4, 4 ),
 ( 0.4074455897393662873, 0.5000000000000000000 ),
 .UNSPECIFIED. ) 
 CURVE ( )  GEOMETRIC_REPRESENTATION_ITEM ( )  RATIONAL_B_SPLINE_CURVE ( ( 0.6983129098260995038, 0.7760317562606738884, 0.8765941196519654310, 0.9999999999999525935 ) ) 
 REPRESENTATION_ITEM ( '' )  );
#42825 = ORIENTED_EDGE ( 'NONE', *, *, #5266, .F. ) ;
#42826 = LINE ( 'NONE', #39609, #39026 ) ;
#42827 = CARTESIAN_POINT ( 'NONE',  ( -23.78676244964941233, -10.93361294341921131, 73.54688584860882372 ) ) ;
#42828 = CARTESIAN_POINT ( 'NONE',  ( -15.61466140752867915, -21.57136684691790407, 72.27248776654836604 ) ) ;
#42829 = CARTESIAN_POINT ( 'NONE',  ( -13.69284385541286753, -8.630756214087254463, 51.74842643355279392 ) ) ;
#42830 = EDGE_CURVE ( 'NONE', #22802, #21258, #16473, .T. ) ;
#42831 = VERTEX_POINT ( 'NONE', #8369 ) ;
#42832 = ADVANCED_FACE ( 'NONE', ( #46043 ), #30028, .T. ) ;
#42833 = CARTESIAN_POINT ( 'NONE',  ( -10.55741651006804993, -16.16889119771467875, 68.08653743916322298 ) ) ;
#42834 =( BOUNDED_CURVE ( )  B_SPLINE_CURVE ( 3, ( #17617, #35845, #10003, #43507 ),
 .UNSPECIFIED., .F., .F. ) 
 B_SPLINE_CURVE_WITH_KNOTS ( ( 4, 4 ),
 ( 0.000000000000000000, 0.4074455897393603476 ),
 .UNSPECIFIED. ) 
 CURVE ( )  GEOMETRIC_REPRESENTATION_ITEM ( )  RATIONAL_B_SPLINE_CURVE ( ( 1.000000000000000000, 0.4567392136813374082, 0.3561768502900323208, 0.6983129098260847378 ) ) 
 REPRESENTATION_ITEM ( '' )  );
#42835 = AXIS2_PLACEMENT_3D ( 'NONE', #36350, #17867, #14399 ) ;
#42836 = CARTESIAN_POINT ( 'NONE',  ( -24.00901317767523935, -17.32824147414624960, 69.42811846502259243 ) ) ;
#42837 = EDGE_CURVE ( 'NONE', #8500, #9814, #10183, .T. ) ;
#42838 = EDGE_CURVE ( 'NONE', #27599, #39007, #31228, .T. ) ;
#42839 = VECTOR ( 'NONE', #18601, 1000.000000000000000 ) ;
#42840 = ORIENTED_EDGE ( 'NONE', *, *, #1915, .T. ) ;
#42841 = CARTESIAN_POINT ( 'NONE',  ( -10.12358845859998624, -13.32384912816304556, 74.72171712345732431 ) ) ;
#42842 = CARTESIAN_POINT ( 'NONE',  ( -24.72409385541305582, -15.80920654474410725, 65.99999999999998579 ) ) ;
#42843 = DIRECTION ( 'NONE',  ( 0.9687793358424821033, -0.2479245821708677133, 0.000000000000000000 ) ) ;
#42844 = VERTEX_POINT ( 'NONE', #20429 ) ;
#42845 = CARTESIAN_POINT ( 'NONE',  ( -13.14081611093705604, -9.205013627624930805, 70.94105531385672236 ) ) ;
#42846 = ORIENTED_EDGE ( 'NONE', *, *, #44869, .T. ) ;
#42847 = CARTESIAN_POINT ( 'NONE',  ( -10.01581026994268342, -14.02033193174257342, 61.07967820595483488 ) ) ;
#42848 = DIRECTION ( 'NONE',  ( 1.190035119058586791E-06, 1.172070126139376962E-06, 0.9999999999986050048 ) ) ;
#42849 = ORIENTED_EDGE ( 'NONE', *, *, #23366, .F. ) ;
#42850 = CARTESIAN_POINT ( 'NONE',  ( -10.29788529736029012, -12.63615789972814163, 64.42982626965611814 ) ) ;
#42851 = CARTESIAN_POINT ( 'NONE',  ( -17.88659385650551670, -9.302874398569244363, 51.68646062012417985 ) ) ;
#42852 = ORIENTED_EDGE ( 'NONE', *, *, #21760, .F. ) ;
#42853 = CARTESIAN_POINT ( 'NONE',  ( -17.92189248921373235, -7.825646680082669171, 60.15231005022496902 ) ) ;
#42854 = CARTESIAN_POINT ( 'NONE',  ( -24.10114604821131223, -12.70328962272956019, 73.31395830697397287 ) ) ;
#42855 = CARTESIAN_POINT ( 'NONE',  ( -16.36834346081282732, -22.18410778960565466, 61.94063409281806543 ) ) ;
#42856 = VERTEX_POINT ( 'NONE', #39124 ) ;
#42857 = CARTESIAN_POINT ( 'NONE',  ( -17.42409385541299471, -14.80920654474435594, 52.02966884056656482 ) ) ;
#42858 = CARTESIAN_POINT ( 'NONE',  ( -11.47236147394688111, -10.32806163424019985, 74.55389795262664165 ) ) ;
#42859 = CARTESIAN_POINT ( 'NONE',  ( -12.88390949798720442, -15.97110509908812936, 49.52966884056655772 ) ) ;
#42860 = CARTESIAN_POINT ( 'NONE',  ( -20.50148804175696782, -8.024372594274959525, 66.90291339721898112 ) ) ;
#42861 = CARTESIAN_POINT ( 'NONE',  ( -20.81696265954430558, -20.93198702957875668, 62.11471400680572685 ) ) ;
#42862 = ORIENTED_EDGE ( 'NONE', *, *, #46719, .F. ) ;
#42863 = ORIENTED_EDGE ( 'NONE', *, *, #16755, .F. ) ;
#42864 = CARTESIAN_POINT ( 'NONE',  ( -23.81758491572420411, -18.63389732182343650, 72.90221683627511595 ) ) ;
#42865 = CARTESIAN_POINT ( 'NONE',  ( -14.42683416945219221, -8.428067588089273698, 67.40975083869261653 ) ) ;
#42866 = VERTEX_POINT ( 'NONE', #5410 ) ;
#42867 = CYLINDRICAL_SURFACE ( 'NONE', #15453, 1.999999999999999112 ) ;
#42868 = DIRECTION ( 'NONE',  ( 1.000000000000000000, 0.000000000000000000, 0.000000000000000000 ) ) ;
#42869 = CARTESIAN_POINT ( 'NONE',  ( -18.44909385759799036, -8.112991634885936776, 51.74999426922421719 ) ) ;
#42870 = CARTESIAN_POINT ( 'NONE',  ( -18.50931870666621037, -21.77518001355031529, 72.28510940651260341 ) ) ;
#42871 = CARTESIAN_POINT ( 'NONE',  ( -19.82413079548422274, -21.27835043604049403, 56.49999999999994316 ) ) ;
#42872 = B_SPLINE_CURVE_WITH_KNOTS ( 'NONE', 1,
 ( #43340, #47272 ),
 .UNSPECIFIED., .F., .F.,
 ( 2, 2 ),
 ( 0.000000000000000000, 1.000000000000000000 ),
 .UNSPECIFIED. ) ;
#42873 = CARTESIAN_POINT ( 'NONE',  ( -10.79589914290667885, -12.39663942728299517, 60.89033620964060134 ) ) ;
#42874 = CIRCLE ( 'NONE', #1201, 0.4000000000000006883 ) ;
#42875 = ORIENTED_EDGE ( 'NONE', *, *, #12111, .F. ) ;
#42876 = EDGE_CURVE ( 'NONE', #46252, #9124, #3709, .T. ) ;
#42877 = CARTESIAN_POINT ( 'NONE',  ( -16.65185932245351808, -21.81708442718849383, 65.51092266128213737 ) ) ;
#42878 = AXIS2_PLACEMENT_3D ( 'NONE', #25028, #17619, #35847 ) ;
#42879 = CARTESIAN_POINT ( 'NONE',  ( -20.77150559172585886, -8.660957557044635990, 59.85741905887537939 ) ) ;
#42880 = CARTESIAN_POINT ( 'NONE',  ( -11.13733870171179596, -11.61806121328041996, 67.90392505421056057 ) ) ;
#42881 = CARTESIAN_POINT ( 'NONE',  ( -14.30855566557790404, -8.484641631233271752, 70.74429704309763167 ) ) ;
#42882 = LINE ( 'NONE', #23930, #16652 ) ;
#42883 = ORIENTED_EDGE ( 'NONE', *, *, #16356, .F. ) ;
#42884 = EDGE_LOOP ( 'NONE', ( #35207, #45650, #43484, #8606, #12774 ) ) ;
#42885 = ORIENTED_EDGE ( 'NONE', *, *, #7381, .F. ) ;
#42886 = CARTESIAN_POINT ( 'NONE',  ( -10.88757860859750082, -12.29993007400385352, 57.43930338741527919 ) ) ;
#42887 = ORIENTED_EDGE ( 'NONE', *, *, #11483, .T. ) ;
#42888 = EDGE_CURVE ( 'NONE', #44738, #21373, #27785, .T. ) ;
#42889 = CARTESIAN_POINT ( 'NONE',  ( -19.74436319619195501, -10.72363366794506412, 49.52966884056655772 ) ) ;
#42890 = CARTESIAN_POINT ( 'NONE',  ( -10.01391823204708231, -15.58571177677185915, 57.68137499724732464 ) ) ;
#42891 = EDGE_CURVE ( 'NONE', #20914, #35358, #32493, .T. ) ;
#42892 = EDGE_CURVE ( 'NONE', #44110, #115, #10969, .T. ) ;
#42893 = EDGE_LOOP ( 'NONE', ( #23247, #5322, #14488, #18462 ) ) ;
#42894 = CARTESIAN_POINT ( 'NONE',  ( -11.16720021946830244, -11.56054808309503557, 67.91864607954204303 ) ) ;
#42895 = CARTESIAN_POINT ( 'NONE',  ( -22.37985696210566999, -19.82347738784875801, 69.32417989525721680 ) ) ;
#42896 = ORIENTED_EDGE ( 'NONE', *, *, #35444, .F. ) ;
#42897 = CARTESIAN_POINT ( 'NONE',  ( -10.81107399027072091, -12.51381874052989751, 57.34359806747983868 ) ) ;
#42898 = ORIENTED_EDGE ( 'NONE', *, *, #13348, .T. ) ;
#42899 = CARTESIAN_POINT ( 'NONE',  ( -10.12170670794182392, -13.33288566098140393, 74.85534528062055415 ) ) ;
#42900 = VECTOR ( 'NONE', #39722, 1000.000000000000000 ) ;
#42901 = ORIENTED_EDGE ( 'NONE', *, *, #41812, .F. ) ;
#42902 = EDGE_CURVE ( 'NONE', #39181, #4870, #7837, .T. ) ;
#42903 = CARTESIAN_POINT ( 'NONE',  ( -16.00544582274271477, -7.903112417841744453, 63.95538887075813506 ) ) ;
#42904 = CARTESIAN_POINT ( 'NONE',  ( -12.98528529603622594, -9.327379713820903362, 74.41103219219326093 ) ) ;
#42905 = CARTESIAN_POINT ( 'NONE',  ( -19.30128557755455176, -21.60500301973953086, 58.81035253397666196 ) ) ;
#42906 = ORIENTED_EDGE ( 'NONE', *, *, #609, .F. ) ;
#42907 = CARTESIAN_POINT ( 'NONE',  ( -24.27065772746464134, -17.74681645512229622, 62.61214498559143493 ) ) ;
#42908 = CARTESIAN_POINT ( 'NONE',  ( -24.42568804997961607, -14.79584355430348097, 62.90223455604580494 ) ) ;
#42909 = CARTESIAN_POINT ( 'NONE',  ( -13.62949042321701398, -8.926946430974666669, 56.96967755885751217 ) ) ;
#42910 = CYLINDRICAL_SURFACE ( 'NONE', #36288, 0.1500000000000009936 ) ;
#42911 = CARTESIAN_POINT ( 'NONE',  ( -20.51077986664673602, -21.09370094575390198, 58.83402211390806968 ) ) ;
#42912 = VERTEX_POINT ( 'NONE', #43327 ) ;
#42913 = DIRECTION ( 'NONE',  ( -0.9904243694481096316, -0.1380563957348939497, -6.973877022548522575E-08 ) ) ;
#42914 = CARTESIAN_POINT ( 'NONE',  ( -11.73260633559210042, -10.00184260618991416, 67.61401560909513364 ) ) ;
#42915 = PLANE ( 'NONE',  #17178 ) ;
#42916 = CARTESIAN_POINT ( 'NONE',  ( -23.54659830298692569, -19.05403935986104003, 66.08035378328281695 ) ) ;
#42917 = CARTESIAN_POINT ( 'NONE',  ( -14.14525230689395130, -20.99386949692624427, 72.21142318359106582 ) ) ;
#42918 = CARTESIAN_POINT ( 'NONE',  ( -16.56159385650551386, -9.295667164867525756, 49.30633214617472504 ) ) ;
#42919 = EDGE_CURVE ( 'NONE', #31686, #48232, #7290, .T. ) ;
#42920 = ORIENTED_EDGE ( 'NONE', *, *, #22928, .T. ) ;
#42921 = DIRECTION ( 'NONE',  ( -0.9858639740050658684, -0.1675476790616295675, 1.191395510700210208E-16 ) ) ;
#42922 = CARTESIAN_POINT ( 'NONE',  ( -10.78978130820344994, -12.42417047965500743, 57.62857332104950814 ) ) ;
#42923 = ORIENTED_EDGE ( 'NONE', *, *, #29235, .F. ) ;
#42924 = CARTESIAN_POINT ( 'NONE',  ( -24.27033155520888030, -13.12649183948492393, 62.98264177272948672 ) ) ;
#42925 = CARTESIAN_POINT ( 'NONE',  ( -10.50429924535250414, -16.15944446069507023, 71.46222527016213633 ) ) ;
#42926 = CARTESIAN_POINT ( 'NONE',  ( -22.83929682888979329, -10.29453308790038157, 66.55654356380499337 ) ) ;
#42927 = CARTESIAN_POINT ( 'NONE',  ( -22.52972399543339677, -9.943266245822872662, 69.89689837695897268 ) ) ;
#42928 = CARTESIAN_POINT ( 'NONE',  ( -14.78766009005058812, -21.34800739930362568, 58.45145834864037937 ) ) ;
#42929 = ORIENTED_EDGE ( 'NONE', *, *, #4108, .T. ) ;
#42930 = CARTESIAN_POINT ( 'NONE',  ( -12.10369268100898132, -9.594121713099781346, 57.27430968559156810 ) ) ;
#42931 = DIRECTION ( 'NONE',  ( 0.000000000000000000, 0.000000000000000000, 1.000000000000000000 ) ) ;
#42932 = DIRECTION ( 'NONE',  ( -0.9796876409582463419, 0.2005296141562636081, 7.890952370353029293E-08 ) ) ;
#42933 = ORIENTED_EDGE ( 'NONE', *, *, #1713, .T. ) ;
#42934 = CARTESIAN_POINT ( 'NONE',  ( -10.43024361443327130, -12.24190297806011962, 57.49003819789888325 ) ) ;
#42935 = CARTESIAN_POINT ( 'NONE',  ( -10.39864765667697988, -15.39886713103467741, 57.57352593471627955 ) ) ;
#42936 = CARTESIAN_POINT ( 'NONE',  ( -23.24966709594328051, -18.77981918306044307, 66.12389400104751758 ) ) ;
#42937 = DIRECTION ( 'NONE',  ( -3.413470714839332458E-33, 1.190614954331866791E-16, -1.000000000000000000 ) ) ;
#42938 = ORIENTED_EDGE ( 'NONE', *, *, #20210, .T. ) ;
#42939 = ORIENTED_EDGE ( 'NONE', *, *, #374, .F. ) ;
#42940 = AXIS2_PLACEMENT_3D ( 'NONE', #21140, #44518, #25320 ) ;
#42941 = CARTESIAN_POINT ( 'NONE',  ( -21.11784385541304943, -6.860780111191487229, 51.02154966934377001 ) ) ;
#42942 = DIRECTION ( 'NONE',  ( -0.2853368233144828459, 0.3443586753093350605, 0.8944271909999156334 ) ) ;
#42943 = CARTESIAN_POINT ( 'NONE',  ( -14.81535805098777736, -7.777528402031248511, 56.49999999999994316 ) ) ;
#42944 = CARTESIAN_POINT ( 'NONE',  ( -11.55673057814116333, -10.21815940138198009, 71.01247170384147012 ) ) ;
#42945 = CARTESIAN_POINT ( 'NONE',  ( -22.92130433334872563, -10.47544214307853672, 59.67491392133583616 ) ) ;
#42946 = EDGE_CURVE ( 'NONE', #5216, #37238, #39093, .T. ) ;
#42947 = CARTESIAN_POINT ( 'NONE',  ( -14.02573509563205789, -20.92901172694171308, 68.68298393627175358 ) ) ;
#42948 = CARTESIAN_POINT ( 'NONE',  ( -12.57210041907703335, -17.42762882506661271, 53.88362224778187226 ) ) ;
#42949 = CARTESIAN_POINT ( 'NONE',  ( -24.23330780873085644, -17.83228236547056156, 62.59644069454639492 ) ) ;
#42950 = ORIENTED_EDGE ( 'NONE', *, *, #2760, .T. ) ;
#42951 =( BOUNDED_CURVE ( )  B_SPLINE_CURVE ( 3, ( #337, #37240, #26925, #11649 ),
 .UNSPECIFIED., .F., .F. ) 
 B_SPLINE_CURVE_WITH_KNOTS ( ( 4, 4 ),
 ( 0.9074455897393648440, 1.000000000000000000 ),
 .UNSPECIFIED. ) 
 CURVE ( )  GEOMETRIC_REPRESENTATION_ITEM ( )  RATIONAL_B_SPLINE_CURVE ( ( 0.6983129098260881795, 0.7760317562606939834, 0.8765941196519979606, 1.000000000000000000 ) ) 
 REPRESENTATION_ITEM ( '' )  );
#42952 = DIRECTION ( 'NONE',  ( -0.1240347345892086062, 1.145860353393066553E-16, -0.9922778767136676281 ) ) ;
#42953 = CARTESIAN_POINT ( 'NONE',  ( -24.27033198218900978, -13.12649362337911541, 62.83264177274070050 ) ) ;
#42954 = ORIENTED_EDGE ( 'NONE', *, *, #26378, .T. ) ;
#42955 = ADVANCED_FACE ( 'NONE', ( #18091 ), #25994, .T. ) ;
#42956 = EDGE_CURVE ( 'NONE', #33912, #35760, #33692, .T. ) ;
#42957 = CARTESIAN_POINT ( 'NONE',  ( -21.29196722032537537, -20.70380199363842877, 72.53918572867779346 ) ) ;
#42958 = DIRECTION ( 'NONE',  ( 8.339041846367054613E-07, 7.401746001654338994E-06, -0.9999999999722594124 ) ) ;
#42959 = VERTEX_POINT ( 'NONE', #10491 ) ;
#42960 = CYLINDRICAL_SURFACE ( 'NONE', #19110, 1.999999999999999556 ) ;
#42961 = EDGE_CURVE ( 'NONE', #10578, #41130, #33430, .T. ) ;
#42962 = FACE_OUTER_BOUND ( 'NONE', #17660, .T. ) ;
#42963 = ADVANCED_FACE ( 'NONE', ( #41010 ), #211, .T. ) ;
#42964 = DIRECTION ( 'NONE',  ( 0.2393415023380396911, -0.9709354485539016810, 6.438601123316501445E-08 ) ) ;
#42965 = CARTESIAN_POINT ( 'NONE',  ( -22.58392976434795330, -19.53954411336175667, 72.83503833621796275 ) ) ;
#42966 = VERTEX_POINT ( 'NONE', #15864 ) ;
#42967 = CARTESIAN_POINT ( 'NONE',  ( -18.53556661698576136, -22.17591588139245573, 72.40015654177148008 ) ) ;
#42968 = DIRECTION ( 'NONE',  ( -3.071710424422018668E-17, 6.404604876783312462E-16, 1.000000000000000000 ) ) ;
#42970 =( BOUNDED_CURVE ( )  B_SPLINE_CURVE ( 3, ( #7557, #18869, #29707, #45728 ),
 .UNSPECIFIED., .F., .F. ) 
 B_SPLINE_CURVE_WITH_KNOTS ( ( 4, 4 ),
 ( 0.5000000000000000000, 0.9074455897393707282 ),
 .UNSPECIFIED. ) 
 CURVE ( )  GEOMETRIC_REPRESENTATION_ITEM ( )  RATIONAL_B_SPLINE_CURVE ( ( 1.000000000000003553, 0.4567392136813279158, 0.3561768502900262146, 0.6983129098261022794 ) ) 
 REPRESENTATION_ITEM ( '' )  );
#42969 = CARTESIAN_POINT ( 'NONE',  ( -11.32522400900782067, -11.27219014254736074, 60.96413645226084554 ) ) ;
#42971 = AXIS2_PLACEMENT_3D ( 'NONE', #15679, #48694, #208 ) ;
#42972 = DIRECTION ( 'NONE',  ( -0.2479245821708777886, -0.9687793358424794388, 0.000000000000000000 ) ) ;
#42973 = DIRECTION ( 'NONE',  ( -3.549360974551883545E-17, 6.371834667872732552E-18, 1.000000000000000000 ) ) ;
#42974 = DIRECTION ( 'NONE',  ( -0.8356905716187447153, 0.5492005722024784209, 7.728900804118605128E-08 ) ) ;
#42975 = EDGE_CURVE ( 'NONE', #37066, #23568, #1331, .T. ) ;
#42976 = LINE ( 'NONE', #31656, #19599 ) ;
#42977 = VERTEX_POINT ( 'NONE', #26230 ) ;
#42978 = B_SPLINE_CURVE_WITH_KNOTS ( 'NONE', 3,
 ( #27839, #46481, #930, #31445, #34394, #41565, #23336, #30737, #20122, #453 ),
 .UNSPECIFIED., .F., .F.,
 ( 4, 2, 2, 2, 4 ),
 ( 0.6272669072877811169, 0.7522669073073010582, 0.8772669073268211104, 1.002266907346341052, 1.127266907365860993 ),
 .UNSPECIFIED. ) ;
#42979 = CARTESIAN_POINT ( 'NONE',  ( -12.10506971550441335, -10.25793058095366561, 67.78280305760789304 ) ) ;
#42980 = CYLINDRICAL_SURFACE ( 'NONE', #26625, 0.1500000000000077383 ) ;
#42981 = CYLINDRICAL_SURFACE ( 'NONE', #23541, 2.000000000000003109 ) ;
#42982 = ORIENTED_EDGE ( 'NONE', *, *, #42756, .F. ) ;
#42983 = CARTESIAN_POINT ( 'NONE',  ( -20.11870507851999079, -21.33255209822014820, 69.09049654866474555 ) ) ;
#42984 = EDGE_LOOP ( 'NONE', ( #21840, #1238, #27284, #23718, #44607 ) ) ;
#42985 = ORIENTED_EDGE ( 'NONE', *, *, #38094, .T. ) ;
#42986 = ORIENTED_EDGE ( 'NONE', *, *, #29940, .F. ) ;
#42987 = DIRECTION ( 'NONE',  ( -0.9687793358424819923, 0.2479245821708680464, 0.000000000000000000 ) ) ;
#42988 = CARTESIAN_POINT ( 'NONE',  ( -23.78500266573477262, -11.88707733699690827, 59.78235732566622573 ) ) ;
#42989 = CARTESIAN_POINT ( 'NONE',  ( -21.33694788700791278, -9.004934622526002741, 73.60128753634342047 ) ) ;
#42990 = CARTESIAN_POINT ( 'NONE',  ( -21.68202464530013529, -12.85132308587069438, 52.02966884056656482 ) ) ;
#42991 = CARTESIAN_POINT ( 'NONE',  ( -16.32275379891173372, -22.17735803940487926, 61.95579338972356709 ) ) ;
#42992 = ORIENTED_EDGE ( 'NONE', *, *, #36794, .F. ) ;
#42993 = ORIENTED_EDGE ( 'NONE', *, *, #41608, .F. ) ;
#42994 = CARTESIAN_POINT ( 'NONE',  ( -20.58659385650551599, -9.302874398569244363, 51.68646062012417985 ) ) ;
#42995 = CARTESIAN_POINT ( 'NONE',  ( -11.47327410250610313, -11.02222997523968573, 60.77066038170728035 ) ) ;
#42996 = CARTESIAN_POINT ( 'NONE',  ( -24.87380742036101466, -14.88762772862374284, 59.36583317909604318 ) ) ;
#42997 = CARTESIAN_POINT ( 'NONE',  ( -23.21838898650911531, -18.73703798069015392, 65.82389378437922289 ) ) ;
#42998 = ADVANCED_FACE ( 'NONE', ( #26726 ), #34578, .T. ) ;
#42999 = CARTESIAN_POINT ( 'NONE',  ( -22.78034385650551741, -6.424090610841176385, 49.80797279389977916 ) ) ;
#43000 = VERTEX_POINT ( 'NONE', #41746 ) ;
#43001 = CARTESIAN_POINT ( 'NONE',  ( -24.26499789074519597, -17.75976756996305639, 62.65856417960095825 ) ) ;
#43002 = ADVANCED_FACE ( 'NONE', ( #4319 ), #37530, .F. ) ;
#43003 = CARTESIAN_POINT ( 'NONE',  ( -12.96596534320165794, -9.347742485070138940, 70.84925352874383009 ) ) ;
#43004 = CARTESIAN_POINT ( 'NONE',  ( -17.24796809485249227, -7.811422621481736606, 67.12925709854650336 ) ) ;
#43005 = AXIS2_PLACEMENT_3D ( 'NONE', #19084, #41748, #30432 ) ;
#43006 = VERTEX_POINT ( 'NONE', #8032 ) ;
#43007 = CARTESIAN_POINT ( 'NONE',  ( -21.11784385541296061, -6.860780111191562725, 51.02154966934399027 ) ) ;
#43008 = B_SPLINE_CURVE_WITH_KNOTS ( 'NONE', 3,
 ( #37992, #8446, #4276, #12377, #30873, #45887, #42679, #23732, #12143, #11911 ),
 .UNSPECIFIED., .F., .F.,
 ( 4, 2, 2, 2, 4 ),
 ( 0.000000000000000000, 0.2500000000000000000, 0.5000000000000000000, 0.7500000000000000000, 1.000000000000000000 ),
 .UNSPECIFIED. ) ;
#43009 = CARTESIAN_POINT ( 'NONE',  ( -9.975583786612773451, -14.65598763567812313, 71.44287367974872893 ) ) ;
#43010 = CARTESIAN_POINT ( 'NONE',  ( -18.55956930788366677, -7.446158750330262421, 74.02559786541287679 ) ) ;
#43011 = LINE ( 'NONE', #24312, #38110 ) ;
#43012 = EDGE_CURVE ( 'NONE', #43621, #30016, #23711, .T. ) ;
#43013 = ORIENTED_EDGE ( 'NONE', *, *, #47323, .T. ) ;
#43014 = CARTESIAN_POINT ( 'NONE',  ( -19.62595585458452163, -8.103479577873935469, 60.10526007146324901 ) ) ;
#43015 = ADVANCED_FACE ( 'NONE', ( #14869 ), #617, .T. ) ;
#43016 = CARTESIAN_POINT ( 'NONE',  ( -22.94084299836913843, -19.11815316549774479, 58.88410675570529662 ) ) ;
#43017 = CARTESIAN_POINT ( 'NONE',  ( -20.13087680518396994, -7.868272569338301103, 73.82758314367622177 ) ) ;
#43018 = ORIENTED_EDGE ( 'NONE', *, *, #46172, .F. ) ;
#43019 = CARTESIAN_POINT ( 'NONE',  ( -19.40930774675918613, -7.628578061947676403, 60.11092995211872392 ) ) ;
#43020 = VERTEX_POINT ( 'NONE', #8258 ) ;
#43021 = CARTESIAN_POINT ( 'NONE',  ( -14.09914604623946488, -8.649277798895779412, 74.19954655170327840 ) ) ;
#43022 = CARTESIAN_POINT ( 'NONE',  ( -9.974235501303020612, -14.86645057852294016, 75.05424837986554110 ) ) ;
#43023 = EDGE_CURVE ( 'NONE', #43233, #20025, #30434, .T. ) ;
#43024 = ORIENTED_EDGE ( 'NONE', *, *, #21135, .F. ) ;
#43025 = FACE_OUTER_BOUND ( 'NONE', #16640, .T. ) ;
#43026 = CARTESIAN_POINT ( 'NONE',  ( -45.92409385541306222, -14.90920654474410867, 70.50000000000000000 ) ) ;
#43027 = DIRECTION ( 'NONE',  ( 1.000000000000000000, -4.164305804376849172E-17, 1.614929280266638808E-16 ) ) ;
#43028 = DIRECTION ( 'NONE',  ( -0.9687793358424821033, 0.2479245821708677133, 0.000000000000000000 ) ) ;
#43029 = VERTEX_POINT ( 'NONE', #26964 ) ;
#43030 = DIRECTION ( 'NONE',  ( -0.3478314405900308492, -0.9375570856950864451, 0.000000000000000000 ) ) ;
#43031 = UNCERTAINTY_MEASURE_WITH_UNIT (LENGTH_MEASURE( 1.000000000000000082E-05 ), #15533, 'distance_accuracy_value', 'NONE');
#43032 = ADVANCED_FACE ( 'NONE', ( #45923 ), #18576, .T. ) ;
#43033 = CARTESIAN_POINT ( 'NONE',  ( -20.94477883430487708, -21.37566986424753068, 58.75819861804361466 ) ) ;
#43034 = CARTESIAN_POINT ( 'NONE',  ( -23.41700317716350810, -19.23526875778016176, 62.51553421167685087 ) ) ;
#43035 = ORIENTED_EDGE ( 'NONE', *, *, #44305, .F. ) ;
#43036 = DIRECTION ( 'NONE',  ( -3.071710424422018668E-17, 6.404604876783312462E-16, 1.000000000000000000 ) ) ;
#43037 = AXIS2_PLACEMENT_3D ( 'NONE', #41906, #42150, #37707 ) ;
#43038 = VECTOR ( 'NONE', #8147, 1000.000000000000227 ) ;
#43039 = DIRECTION ( 'NONE',  ( 2.866981220435666553E-17, -1.000000000000000000, -1.190614954331866791E-16 ) ) ;
#43040 = ORIENTED_EDGE ( 'NONE', *, *, #36111, .T. ) ;
#43041 = EDGE_LOOP ( 'NONE', ( #4226, #18300 ) ) ;
#43042 = CARTESIAN_POINT ( 'NONE',  ( -13.01353397724842154, -8.804979801064929390, 64.09441804368185558 ) ) ;
#43043 = CARTESIAN_POINT ( 'NONE',  ( -35.32409385541306079, -25.10920654474410441, 52.29999999999998295 ) ) ;
#43044 = AXIS2_PLACEMENT_3D ( 'NONE', #43451, #43695, #40235 ) ;
#43045 = CARTESIAN_POINT ( 'NONE',  ( -18.98034385650551670, -6.424090610841176385, 49.80797279389977916 ) ) ;
#43046 = CARTESIAN_POINT ( 'NONE',  ( -12.14425506381237518, -10.13739722748950634, 64.32914326607961186 ) ) ;
#43047 = CARTESIAN_POINT ( 'NONE',  ( -19.28352822169459202, -22.07505156356299381, 53.49999999999994316 ) ) ;
#43048 = CARTESIAN_POINT ( 'NONE',  ( -18.64414733763933896, -7.459617552211802227, 74.00210948319649162 ) ) ;
#43049 = CARTESIAN_POINT ( 'NONE',  ( -23.34288328645119037, -19.33377384263253873, 59.06905932422779415 ) ) ;
#43050 = ORIENTED_EDGE ( 'NONE', *, *, #40239, .T. ) ;
#43051 = VERTEX_POINT ( 'NONE', #42227 ) ;
#43052 = CARTESIAN_POINT ( 'NONE',  ( -10.64512080333459387, -11.71903002653516168, 74.81486074884371362 ) ) ;
#43053 = CARTESIAN_POINT ( 'NONE',  ( 0.000000000000000000, 0.000000000000000000, 0.000000000000000000 ) ) ;
#43054 = DIRECTION ( 'NONE',  ( 0.9687793358424821033, -0.2479245821708677133, 0.000000000000000000 ) ) ;
#43055 = CYLINDRICAL_SURFACE ( 'NONE', #28398, 1.999999999999994893 ) ;
#43056 = CARTESIAN_POINT ( 'NONE',  ( -13.38575581802539993, -9.030060914960570173, 60.72478133471773276 ) ) ;
#43057 = DIRECTION ( 'NONE',  ( -3.071710424422018668E-17, 6.404604876783312462E-16, 1.000000000000000000 ) ) ;
#43058 = ADVANCED_FACE ( 'NONE', ( #45443 ), #13303, .T. ) ;
#43059 = ORIENTED_EDGE ( 'NONE', *, *, #24493, .T. ) ;
#43060 = CARTESIAN_POINT ( 'NONE',  ( 8.575906144586951996, -6.109215713985405749, 50.50605614422795497 ) ) ;
#43061 = CARTESIAN_POINT ( 'NONE',  ( -24.02298749829535751, -11.35118778494372194, 66.52940360090373417 ) ) ;
#43062 = CARTESIAN_POINT ( 'NONE',  ( -17.16863824095212010, -7.760122409783657638, 67.02039628079666045 ) ) ;
#43063 = CARTESIAN_POINT ( 'NONE',  ( -24.51063837352987207, -17.11019555850099039, 72.99680753360935626 ) ) ;
#43064 = ORIENTED_EDGE ( 'NONE', *, *, #37854, .T. ) ;
#43065 = CARTESIAN_POINT ( 'NONE',  ( -24.41403469082061051, -14.40519231153102986, 69.76348327924310411 ) ) ;
#43066 = AXIS2_PLACEMENT_3D ( 'NONE', #28631, #6222, #3245 ) ;
#43067 = AXIS2_PLACEMENT_3D ( 'NONE', #11106, #33478, #23170 ) ;
#43068 = CARTESIAN_POINT ( 'NONE',  ( -19.27972737141692861, -8.007758698492196459, 60.26092978174835935 ) ) ;
#43069 = CARTESIAN_POINT ( 'NONE',  ( -33.95962776134579286, -8.109206544744111511, 50.50000000000000000 ) ) ;
#43070 = EDGE_CURVE ( 'NONE', #37096, #45761, #47378, .T. ) ;
#43071 = CARTESIAN_POINT ( 'NONE',  ( -18.67229796221712590, -7.919758957113036679, 73.95137594816235094 ) ) ;
#43072 = CARTESIAN_POINT ( 'NONE',  ( -11.35070632453979478, -11.22329048540824559, 57.09414325051740491 ) ) ;
#43073 = ADVANCED_FACE ( 'NONE', ( #22533 ), #35330, .T. ) ;
#43074 = CARTESIAN_POINT ( 'NONE',  ( -22.55534385759798965, -8.623186033802570094, 49.24843789510466507 ) ) ;
#43075 = ORIENTED_EDGE ( 'NONE', *, *, #17440, .T. ) ;
#43076 = CARTESIAN_POINT ( 'NONE',  ( -10.49080373283728207, -13.84193255407867262, 57.73208522591303193 ) ) ;
#43077 = ORIENTED_EDGE ( 'NONE', *, *, #37674, .T. ) ;
#43078 = FACE_OUTER_BOUND ( 'NONE', #603, .T. ) ;
#43079 = ADVANCED_FACE ( 'NONE', ( #5045 ), #9476, .T. ) ;
#43080 = CYLINDRICAL_SURFACE ( 'NONE', #13191, 1.250000000000001110 ) ;
#43081 = ORIENTED_EDGE ( 'NONE', *, *, #14290, .T. ) ;
#43082 = CARTESIAN_POINT ( 'NONE',  ( -18.46885980906216318, -22.18634193242058572, 68.92859349268570668 ) ) ;
#43083 = CARTESIAN_POINT ( 'NONE',  ( -11.42506541550659449, -10.39151053845774442, 74.61601874447606519 ) ) ;
#43084 = EDGE_LOOP ( 'NONE', ( #16190, #43964, #17980, #25777, #19891 ) ) ;
#43085 = CARTESIAN_POINT ( 'NONE',  ( -15.34465393633500696, -21.54586957516256263, 68.86120835375241711 ) ) ;
#43086 = EDGE_CURVE ( 'NONE', #18610, #41894, #5285, .T. ) ;
#43087 =( BOUNDED_CURVE ( )  B_SPLINE_CURVE ( 3, ( #48028, #44120, #25384, #37160 ),
 .UNSPECIFIED., .F., .F. ) 
 B_SPLINE_CURVE_WITH_KNOTS ( ( 4, 4 ),
 ( 0.5000000000000000000, 0.9074455897393596260 ),
 .UNSPECIFIED. ) 
 CURVE ( )  GEOMETRIC_REPRESENTATION_ITEM ( )  RATIONAL_B_SPLINE_CURVE ( ( 1.000000000000005107, 0.4567392136813352987, 0.3561768502900278799, 0.6983129098260882905 ) ) 
 REPRESENTATION_ITEM ( '' )  );
#43088 = CARTESIAN_POINT ( 'NONE',  ( -17.61716384397549362, -7.761810361906310796, 63.55057029321027784 ) ) ;
#43089 = CARTESIAN_POINT ( 'NONE',  ( -10.90975526000855389, -17.37128585871089825, 64.91274058815852754 ) ) ;
#43090 = VERTEX_POINT ( 'NONE', #31869 ) ;
#43091 = LINE ( 'NONE', #16238, #38890 ) ;
#43092 = DIRECTION ( 'NONE',  ( 0.000000000000000000, 0.000000000000000000, 1.000000000000000000 ) ) ;
#43093 = CARTESIAN_POINT ( 'NONE',  ( -20.66848101912799862, -8.549761622307149977, 60.12653141481577990 ) ) ;
#43094 = CARTESIAN_POINT ( 'NONE',  ( -12.30444741248500051, -20.22242042389802918, 64.98019641849691652 ) ) ;
#43095 = ORIENTED_EDGE ( 'NONE', *, *, #29153, .F. ) ;
#43096 = ORIENTED_EDGE ( 'NONE', *, *, #22500, .F. ) ;
#43097 = CARTESIAN_POINT ( 'NONE',  ( -11.70707196628297986, -18.84868401720091313, 68.51689578196801733 ) ) ;
#43098 = CARTESIAN_POINT ( 'NONE',  ( -10.99529498506645275, -17.70292631970418640, 71.86718196782238977 ) ) ;
#43099 = VERTEX_POINT ( 'NONE', #13377 ) ;
#43101 = CARTESIAN_POINT ( 'NONE',  ( -21.99229891970641404, -20.18939897536854389, 65.84854503242263490 ) ) ;
#43100 = CIRCLE ( 'NONE', #28930, 1.999999999999994893 ) ;
#43102 = DIRECTION ( 'NONE',  ( 0.9687793358424821033, -0.2479245821708677133, 0.000000000000000000 ) ) ;
#43103 = CARTESIAN_POINT ( 'NONE',  ( -19.29284385759799036, -8.630756214087126565, 51.74842643355248129 ) ) ;
#43104 = CARTESIAN_POINT ( 'NONE',  ( -10.42512874152911628, -14.93649829652840744, 74.79778865176552927 ) ) ;
#43105 = AXIS2_PLACEMENT_3D ( 'NONE', #38181, #19479, #27113 ) ;
#43106 = EDGE_CURVE ( 'NONE', #35822, #42531, #25435, .T. ) ;
#43107 = CARTESIAN_POINT ( 'NONE',  ( -11.01197672498280866, -17.74032467813711378, 71.85246142747085685 ) ) ;
#43108 = CARTESIAN_POINT ( 'NONE',  ( -12.31380134045779506, -10.02538898168817916, 60.55918086676557976 ) ) ;
#43109 =( BOUNDED_CURVE ( )  B_SPLINE_CURVE ( 3, ( #41162, #29106, #14531, #29591 ),
 .UNSPECIFIED., .F., .F. ) 
 B_SPLINE_CURVE_WITH_KNOTS ( ( 4, 4 ),
 ( 0.9074455897393640669, 1.000000000000000000 ),
 .UNSPECIFIED. ) 
 CURVE ( )  GEOMETRIC_REPRESENTATION_ITEM ( )  RATIONAL_B_SPLINE_CURVE ( ( 0.6983129098260918433, 0.7760317562606970920, 0.8765941196519998480, 1.000000000000000000 ) ) 
 REPRESENTATION_ITEM ( '' )  );
#43110 = VECTOR ( 'NONE', #11529, 1000.000000000000114 ) ;
#43111 = CIRCLE ( 'NONE', #40741, 5.000000000000000000 ) ;
#43112 = ADVANCED_FACE ( 'NONE', ( #12665 ), #28716, .T. ) ;
#43113 = VERTEX_POINT ( 'NONE', #32115 ) ;
#43114 = CARTESIAN_POINT ( 'NONE',  ( -16.52316554273587101, -21.80170452179945073, 65.24036514508233608 ) ) ;
#43115 = EDGE_CURVE ( 'NONE', #31776, #7068, #12422, .T. ) ;
#43116 = CARTESIAN_POINT ( 'NONE',  ( -20.73702004518044717, -8.642678983225538403, 60.14125279966339832 ) ) ;
#43117 = EDGE_CURVE ( 'NONE', #19371, #43552, #42336, .T. ) ;
#43118 = CARTESIAN_POINT ( 'NONE',  ( 18.54465614458695200, 0.6407533398237036382, 50.52649563099625851 ) ) ;
#43119 = AXIS2_PLACEMENT_3D ( 'NONE', #17750, #32324, #9909 ) ;
#43120 = CARTESIAN_POINT ( 'NONE',  ( 8.575906144586953772, 2.171027184030513979, 40.53108358537571831 ) ) ;
#43121 = ORIENTED_EDGE ( 'NONE', *, *, #42705, .F. ) ;
#43122 = ORIENTED_EDGE ( 'NONE', *, *, #48055, .F. ) ;
#43123 =( BOUNDED_SURFACE ( )  B_SPLINE_SURFACE ( 3, 1, ( 
 ( #2431, #2897 ),
 ( #6610, #32699 ),
 ( #43566, #32929 ),
 ( #47971, #14208 ),
 ( #21150, #13963 ),
 ( #21864, #28541 ),
 ( #9826, #29261 ) ),
 .UNSPECIFIED., .T., .F., .F. ) 
 B_SPLINE_SURFACE_WITH_KNOTS ( ( 4, 3, 4 ),
 ( 2, 2 ),
 ( 0.000000000000000000, 0.5000000000000000000, 1.000000000000000000 ),
 ( 0.000000000000000000, 1.000000000000000000 ),
 .UNSPECIFIED. ) 
 GEOMETRIC_REPRESENTATION_ITEM ( )  RATIONAL_B_SPLINE_SURFACE ( (
 ( 1.000000000000000000, 1.000000000000000000),
 ( 0.3333333333333335369, 0.3333333333333330373),
 ( 0.3333333333333335369, 0.3333333333333330373),
 ( 1.000000000000000000, 1.000000000000000000),
 ( 0.3333333333333333703, 0.3333333333333333703),
 ( 0.3333333333333333703, 0.3333333333333333703),
 ( 1.000000000000000000, 1.000000000000000000) ) ) 
 REPRESENTATION_ITEM ( '' )  SURFACE ( )  );
#43124 = EDGE_LOOP ( 'NONE', ( #11677, #41156 ) ) ;
#43125 = CARTESIAN_POINT ( 'NONE',  ( -11.49500183448702906, -10.99442376238782515, 57.22375354680192316 ) ) ;
#43126 = CARTESIAN_POINT ( 'NONE',  ( -22.52837755674526221, -10.01897815596726282, 70.20281741071431725 ) ) ;
#43127 = CARTESIAN_POINT ( 'NONE',  ( -21.69182758944758049, -9.260652778598187140, 63.30039755155743109 ) ) ;
#43128 = VERTEX_POINT ( 'NONE', #35554 ) ;
#43129 = CARTESIAN_POINT ( 'NONE',  ( -10.79923826878429338, -11.40118965656789030, 67.81138754266618207 ) ) ;
#43130 = FACE_OUTER_BOUND ( 'NONE', #3766, .T. ) ;
#43131 = EDGE_LOOP ( 'NONE', ( #27229, #10959, #11889 ) ) ;
#43132 = LINE ( 'NONE', #6440, #41780 ) ;
#43133 = AXIS2_PLACEMENT_3D ( 'NONE', #48345, #26435, #41208 ) ;
#43134 = CARTESIAN_POINT ( 'NONE',  ( -16.97946104448713456, -21.84517140583366057, 72.46543221429990922 ) ) ;
#43135 = CIRCLE ( 'NONE', #11681, 1.999999999999998890 ) ;
#43136 = ORIENTED_EDGE ( 'NONE', *, *, #20472, .T. ) ;
#43137 = CARTESIAN_POINT ( 'NONE',  ( -23.34611022102891553, -10.28892344017613958, 59.70865101996992053 ) ) ;
#43138 = ORIENTED_EDGE ( 'NONE', *, *, #6420, .F. ) ;
#43139 = CARTESIAN_POINT ( 'NONE',  ( -10.60399964645595716, -13.23185723771246280, 71.20828540032704268 ) ) ;
#43140 = VECTOR ( 'NONE', #19354, 1000.000000000000000 ) ;
#43141 = EDGE_LOOP ( 'NONE', ( #29666, #48707, #30550, #30480, #24432 ) ) ;
#43142 = CARTESIAN_POINT ( 'NONE',  ( -11.90827771948429792, -19.81721557328689798, 58.04965466949625608 ) ) ;
#43143 = DIRECTION ( 'NONE',  ( -3.071710424422018668E-17, 6.404604876783312462E-16, 1.000000000000000000 ) ) ;
#43144 = B_SPLINE_CURVE_WITH_KNOTS ( 'NONE', 1,
 ( #32576, #29862 ),
 .UNSPECIFIED., .F., .F.,
 ( 2, 2 ),
 ( 0.000000000000000000, 1.000000000000000000 ),
 .UNSPECIFIED. ) ;
#43145 = EDGE_CURVE ( 'NONE', #28258, #48324, #27925, .T. ) ;
#43146 = EDGE_LOOP ( 'NONE', ( #42360, #3110, #29233 ) ) ;
#43147 = CARTESIAN_POINT ( 'NONE',  ( -9.975583804105555785, -14.65598652642324673, 71.44287259100559595 ) ) ;
#43148 = LINE ( 'NONE', #16540, #18694 ) ;
#43149 = CARTESIAN_POINT ( 'NONE',  ( -22.22619359738691003, -20.50513629785891823, 58.94938195453792673 ) ) ;
#43150 = EDGE_CURVE ( 'NONE', #30656, #2574, #28893, .T. ) ;
#43151 = CIRCLE ( 'NONE', #18747, 1.249999999999999556 ) ;
#43152 = CARTESIAN_POINT ( 'NONE',  ( -24.86242989439883289, -14.39095395922188558, 66.36788051138485400 ) ) ;
#43153 = CARTESIAN_POINT ( 'NONE',  ( -10.46835810950011059, -15.59615148508074789, 61.33789074736403535 ) ) ;
#43154 = CARTESIAN_POINT ( 'NONE',  ( -13.26872317195175199, -21.05283485551296607, 53.49999999999994316 ) ) ;
#43155 = EDGE_LOOP ( 'NONE', ( #44221, #28267, #48180, #9472 ) ) ;
#43156 = CARTESIAN_POINT ( 'NONE',  ( -17.44177517589205451, -7.809228866840242311, 63.74160293238216468 ) ) ;
#43157 = CARTESIAN_POINT ( 'NONE',  ( -24.66525519625502127, -13.05740165471419623, 63.02602501031626048 ) ) ;
#43158 = DIRECTION ( 'NONE',  ( -0.3478314405900308492, -0.9375570856950864451, 0.000000000000000000 ) ) ;
#43159 = CARTESIAN_POINT ( 'NONE',  ( -17.20139249542113191, -7.812750000685961815, 70.49035839633111777 ) ) ;
#43160 = CARTESIAN_POINT ( 'NONE',  ( -19.97882496985426570, -21.80761570639785063, 69.11199379919601427 ) ) ;
#43161 = CARTESIAN_POINT ( 'NONE',  ( -16.33659385650551599, -6.915538690918074494, 49.31353937987644542 ) ) ;
#43162 = ORIENTED_EDGE ( 'NONE', *, *, #39545, .F. ) ;
#43163 = CARTESIAN_POINT ( 'NONE',  ( -16.48749555294751445, -7.817952760528972256, 60.50028745231125527 ) ) ;
#43164 = CYLINDRICAL_SURFACE ( 'NONE', #31310, 0.1500000000000047962 ) ;
#43165 = ORIENTED_EDGE ( 'NONE', *, *, #25705, .F. ) ;
#43166 = FACE_OUTER_BOUND ( 'NONE', #48350, .T. ) ;
#43167 = DIRECTION ( 'NONE',  ( 0.9687793358424822143, -0.2479245821708672415, 0.000000000000000000 ) ) ;
#43168 = CARTESIAN_POINT ( 'NONE',  ( -12.80657247161177814, -9.477853225175101315, 70.73436560138682694 ) ) ;
#43169 = CARTESIAN_POINT ( 'NONE',  ( -23.10898443554464521, -18.97874941859272724, 62.35406906767577340 ) ) ;
#43170 = CARTESIAN_POINT ( 'NONE',  ( -21.36489679027069499, -8.963475500412677377, 73.60128753237400190 ) ) ;
#43171 = B_SPLINE_CURVE_WITH_KNOTS ( 'NONE', 3,
 ( #17624, #17860, #6802, #17392, #32657, #2380, #13918, #9545, #44250, #32883 ),
 .UNSPECIFIED., .F., .F.,
 ( 4, 2, 2, 2, 4 ),
 ( 0.6272669072782520727, 0.7522669073001176931, 0.8772669073219834246, 1.002266907343849045, 1.127266907365714665 ),
 .UNSPECIFIED. ) ;
#43172 = ORIENTED_EDGE ( 'NONE', *, *, #797, .F. ) ;
#43173 = CARTESIAN_POINT ( 'NONE',  ( -22.51726247777427403, -19.68384842258191725, 72.94400547081133368 ) ) ;
#43174 = EDGE_CURVE ( 'NONE', #14, #28748, #33724, .T. ) ;
#43175 = CARTESIAN_POINT ( 'NONE',  ( 18.57590614458706924, 3.151498850453803957, 50.28409723815717314 ) ) ;
#43176 = CARTESIAN_POINT ( 'NONE',  ( -21.99213670719075253, -20.17946569659695299, 59.04970794435396897 ) ) ;
#43177 = EDGE_CURVE ( 'NONE', #1862, #39476, #36890, .T. ) ;
#43178 = ADVANCED_FACE ( 'NONE', ( #3026 ), #44415, .T. ) ;
#43179 = ADVANCED_FACE ( 'NONE', ( #32589 ), #18724, .T. ) ;
#43180 = ORIENTED_EDGE ( 'NONE', *, *, #41861, .F. ) ;
#43181 = DIRECTION ( 'NONE',  ( 3.071710424422018668E-17, -6.404604876783312462E-16, -1.000000000000000000 ) ) ;
#43182 = AXIS2_PLACEMENT_3D ( 'NONE', #29158, #7497, #40969 ) ;
#43183 = CARTESIAN_POINT ( 'NONE',  ( -10.42804297987642670, -12.24802435162854941, 57.45140417473248107 ) ) ;
#43184 = AXIS2_PLACEMENT_3D ( 'NONE', #24351, #1441, #28284 ) ;
#43185 = LINE ( 'NONE', #47833, #37889 ) ;
#43186 = DIRECTION ( 'NONE',  ( -3.071710424422018668E-17, 6.404604876783312462E-16, 1.000000000000000000 ) ) ;
#43187 = CARTESIAN_POINT ( 'NONE',  ( -48.32834917456199975, -13.51240245935757578, 70.50000000000000000 ) ) ;
#43188 = AXIS2_PLACEMENT_3D ( 'NONE', #10653, #309, #14768 ) ;
#43189 = AXIS2_PLACEMENT_3D ( 'NONE', #13551, #47316, #20962 ) ;
#43190 = VERTEX_POINT ( 'NONE', #33052 ) ;
#43191 = EDGE_LOOP ( 'NONE', ( #11209, #20936, #13347, #29677 ) ) ;
#43192 = CARTESIAN_POINT ( 'NONE',  ( -18.13659385541304303, -8.995762431863214559, 51.38120296130585274 ) ) ;
#43193 = CARTESIAN_POINT ( 'NONE',  ( -21.21873014114744294, -20.75103526016286537, 69.34890365675909152 ) ) ;
#43194 = B_SPLINE_CURVE_WITH_KNOTS ( 'NONE', 3,
 ( #17704, #48005, #6883, #7137, #18192, #29292, #14710, #44327, #29782, #10580 ),
 .UNSPECIFIED., .F., .F.,
 ( 4, 2, 2, 2, 4 ),
 ( 0.000000000000000000, 0.2500000000000000000, 0.5000000000000000000, 0.7500000000000000000, 1.000000000000000000 ),
 .UNSPECIFIED. ) ;
#43195 = CARTESIAN_POINT ( 'NONE',  ( -12.96596438542217555, -9.347743257243967818, 70.99925352873879092 ) ) ;
#43196 = VECTOR ( 'NONE', #38792, 1000.000000000000000 ) ;
#43197 = FACE_OUTER_BOUND ( 'NONE', #20720, .T. ) ;
#43198 = CARTESIAN_POINT ( 'NONE',  ( -12.06140467229625912, -20.05244645202335008, 53.49999999999994316 ) ) ;
#43199 = EDGE_CURVE ( 'NONE', #29130, #2205, #1384, .T. ) ;
#43200 = CARTESIAN_POINT ( 'NONE',  ( -10.70532053225239544, -12.67267096592666498, 61.08381491717225487 ) ) ;
#43201 = EDGE_LOOP ( 'NONE', ( #6061, #7562 ) ) ;
#43202 = CARTESIAN_POINT ( 'NONE',  ( -20.18792757799173287, -7.890760935853403879, 73.97742500291465717 ) ) ;
#43203 = CARTESIAN_POINT ( 'NONE',  ( -36.42409385541304800, -6.859212275519750435, 50.50378509014258555 ) ) ;
#43204 = ORIENTED_EDGE ( 'NONE', *, *, #15741, .F. ) ;
#43205 = CARTESIAN_POINT ( 'NONE',  ( -22.34470957656571599, -19.78791530553215949, 69.47417989488683077 ) ) ;
#43206 = FACE_OUTER_BOUND ( 'NONE', #18190, .T. ) ;
#43207 = ORIENTED_EDGE ( 'NONE', *, *, #39607, .T. ) ;
#43208 = CARTESIAN_POINT ( 'NONE',  ( -24.47354778464749003, -12.39902454472287197, 73.42720984402279782 ) ) ;
#43209 = CYLINDRICAL_SURFACE ( 'NONE', #10062, 0.1500000000000045186 ) ;
#43210 = ORIENTED_EDGE ( 'NONE', *, *, #31715, .T. ) ;
#43211 = LINE ( 'NONE', #27699, #41142 ) ;
#43212 = CARTESIAN_POINT ( 'NONE',  ( -22.62394951084894146, -10.04809318868971424, 70.29706442286226320 ) ) ;
#43213 = ADVANCED_FACE ( 'NONE', ( #21523 ), #36504, .F. ) ;
#43214 = AXIS2_PLACEMENT_3D ( 'NONE', #36113, #32440, #2867 ) ;
#43215 = CARTESIAN_POINT ( 'NONE',  ( -16.71957921250844592, -21.82421608262117729, 68.71032757591046902 ) ) ;
#43216 = CARTESIAN_POINT ( 'NONE',  ( -19.45281838860202228, -9.697037067072807659, 53.49999999999995026 ) ) ;
#43217 = ORIENTED_EDGE ( 'NONE', *, *, #27051, .F. ) ;
#43218 = FACE_OUTER_BOUND ( 'NONE', #3083, .T. ) ;
#43219 = CARTESIAN_POINT ( 'NONE',  ( -10.38215599771421793, -15.21658347440237513, 57.86792906985348850 ) ) ;
#43220 = VECTOR ( 'NONE', #9078, 1000.000000000000227 ) ;
#43222 = CARTESIAN_POINT ( 'NONE',  ( -21.32332200014554857, -12.20934075487643788, 52.02966884056656482 ) ) ;
#43221 = CIRCLE ( 'NONE', #29037, 7.500000000000001776 ) ;
#43223 = PLANE ( 'NONE',  #18692 ) ;
#43224 = ITEM_DEFINED_TRANSFORMATION ( 'NONE', 'NONE', #48689,  #29031 ) ;
#43225 = FACE_OUTER_BOUND ( 'NONE', #39325, .T. ) ;
#43226 = CYLINDRICAL_SURFACE ( 'NONE', #6658, 0.1500000000000026590 ) ;
#43227 = CARTESIAN_POINT ( 'NONE',  ( -16.78411603780843464, -21.83009879966275690, 68.84560651669730191 ) ) ;
#43228 = ORIENTED_EDGE ( 'NONE', *, *, #40291, .F. ) ;
#43229 = FACE_OUTER_BOUND ( 'NONE', #35376, .T. ) ;
#43230 = VECTOR ( 'NONE', #46127, 1000.000000000000000 ) ;
#43231 = CARTESIAN_POINT ( 'NONE',  ( -22.63183829035100914, -15.47396055967928952, 50.77966884056655772 ) ) ;
#43232 = CYLINDRICAL_SURFACE ( 'NONE', #2298, 1.999999999999999112 ) ;
#43233 = VERTEX_POINT ( 'NONE', #17793 ) ;
#43234 = CARTESIAN_POINT ( 'NONE',  ( -15.06786346506120822, -21.45763672053845994, 68.66772992167511802 ) ) ;
#43235 = ORIENTED_EDGE ( 'NONE', *, *, #32277, .T. ) ;
#43236 = EDGE_CURVE ( 'NONE', #26989, #21060, #2121, .T. ) ;
#43237 = ADVANCED_FACE ( 'NONE', ( #48326 ), #10440, .T. ) ;
#43238 = ORIENTED_EDGE ( 'NONE', *, *, #19020, .T. ) ;
#43239 = ORIENTED_EDGE ( 'NONE', *, *, #8535, .T. ) ;
#43240 =( REPRESENTATION_RELATIONSHIP ('NONE','NONE', #2768, #11272 ) REPRESENTATION_RELATIONSHIP_WITH_TRANSFORMATION ( #22819 )SHAPE_REPRESENTATION_RELATIONSHIP( ) );
#43241 = CARTESIAN_POINT ( 'NONE',  ( -18.88931992898283241, -7.909354906767774196, 63.43088992718812591 ) ) ;
#43242 = CARTESIAN_POINT ( 'NONE',  ( -14.60689809042302834, -8.346551666329650843, 64.08978840692945766 ) ) ;
#43243 =( BOUNDED_CURVE ( )  B_SPLINE_CURVE ( 3, ( #27114, #8408, #15283, #45125 ),
 .UNSPECIFIED., .F., .F. ) 
 B_SPLINE_CURVE_WITH_KNOTS ( ( 4, 4 ),
 ( 0.000000000000000000, 0.4074455897393584602 ),
 .UNSPECIFIED. ) 
 CURVE ( )  GEOMETRIC_REPRESENTATION_ITEM ( )  RATIONAL_B_SPLINE_CURVE ( ( 1.000000000000000000, 0.4567392136813362979, 0.3561768502900319322, 0.6983129098260868473 ) ) 
 REPRESENTATION_ITEM ( '' )  );
#43244 = CARTESIAN_POINT ( 'NONE',  ( -41.91674091423659121, -14.80920654474421205, 67.05882352941175384 ) ) ;
#43245 = CARTESIAN_POINT ( 'NONE',  ( -24.71637841307600425, -13.28356005536694973, 59.50234599550952197 ) ) ;
#43246 = DIRECTION ( 'NONE',  ( 1.927470528863119542E-16, 0.000000000000000000, -1.000000000000000000 ) ) ;
#43247 = ORIENTED_EDGE ( 'NONE', *, *, #33077, .F. ) ;
#43248 = VERTEX_POINT ( 'NONE', #14561 ) ;
#43249 = EDGE_CURVE ( 'NONE', #27864, #12986, #29644, .T. ) ;
#43250 = ADVANCED_FACE ( 'NONE', ( #36029 ), #2310, .F. ) ;
#43251 = CARTESIAN_POINT ( 'NONE',  ( -22.55534385650551599, -7.417179338643134834, 52.18511593390279302 ) ) ;
#43252 = EDGE_CURVE ( 'NONE', #10544, #6966, #47385, .T. ) ;
#43253 = CARTESIAN_POINT ( 'NONE',  ( -21.59804090337381410, -20.98026344205569771, 72.70941702861115630 ) ) ;
#43254 = DIRECTION ( 'NONE',  ( -0.3566357048164924826, 0.9342435303763381160, -8.054691247152028744E-09 ) ) ;
#43255 = CARTESIAN_POINT ( 'NONE',  ( -24.09752231370279318, -16.92234466904679024, 73.07439273860526896 ) ) ;
#43256 =( BOUNDED_CURVE ( )  B_SPLINE_CURVE ( 2, ( #30154, #44935, #22505, #48599, #30396, #4056, #10939, #22020, #3541 ),
 .UNSPECIFIED., .F., .F. ) 
 B_SPLINE_CURVE_WITH_KNOTS ( ( 3, 2, 2, 2, 3 ),
 ( 0.1250000000000000555, 0.1354166666666666852, 0.1458333333333333703, 0.1562500000000000000, 0.1666666666666666297 ),
 .UNSPECIFIED. ) 
 CURVE ( )  GEOMETRIC_REPRESENTATION_ITEM ( )  RATIONAL_B_SPLINE_CURVE ( ( 0.9999999999999995559, 0.9238795325112871826, 1.000000000000000000, 0.9238795325112867385, 1.000000000000000000, 0.9238795325112867385, 1.000000000000000000, 0.9238795325112869605, 0.9999999999999997780 ) ) 
 REPRESENTATION_ITEM ( '' )  );
#43257 = CARTESIAN_POINT ( 'NONE',  ( -23.17409385650551457, -9.792211528768504536, 50.49490371617623197 ) ) ;
#43258 = AXIS2_PLACEMENT_3D ( 'NONE', #17830, #32852, #6291 ) ;
#43259 = ORIENTED_EDGE ( 'NONE', *, *, #18949, .T. ) ;
#43260 = CARTESIAN_POINT ( 'NONE',  ( -14.79343629209028244, -21.77935231311171194, 61.82874611184421099 ) ) ;
#43261 = EDGE_CURVE ( 'NONE', #4554, #21712, #37808, .T. ) ;
#43262 = CARTESIAN_POINT ( 'NONE',  ( -16.33297564533955537, -22.17887142534084433, 61.90568129439025569 ) ) ;
#43263 = CARTESIAN_POINT ( 'NONE',  ( -24.39763799706551950, -15.84669482609578317, 69.54779622430707775 ) ) ;
#43264 = CONICAL_SURFACE ( 'NONE', #16488, 0.5560000000000009379, 0.06981317007976595157 ) ;
#43265 = ORIENTED_EDGE ( 'NONE', *, *, #35097, .T. ) ;
#43266 = DIRECTION ( 'NONE',  ( -0.000000000000000000, -1.000000000000000000, -0.000000000000000000 ) ) ;
#43267 =( BOUNDED_CURVE ( )  B_SPLINE_CURVE ( 3, ( #27636, #17005, #46356, #12847 ),
 .UNSPECIFIED., .F., .F. ) 
 B_SPLINE_CURVE_WITH_KNOTS ( ( 4, 4 ),
 ( 0.5000000000000000000, 0.9074455897393693959 ),
 .UNSPECIFIED. ) 
 CURVE ( )  GEOMETRIC_REPRESENTATION_ITEM ( )  RATIONAL_B_SPLINE_CURVE ( ( 1.000000000000035749, 0.4567392136813320791, 0.3561768502900052313, 0.6983129098260940637 ) ) 
 REPRESENTATION_ITEM ( '' )  );
#43268 = CARTESIAN_POINT ( 'NONE',  ( -10.36968235478426870, -15.03336378326449285, 71.48349971081816534 ) ) ;
#43269 = CARTESIAN_POINT ( 'NONE',  ( -11.02439547600630831, -11.97273370266293036, 74.85840233422536016 ) ) ;
#43270 = CARTESIAN_POINT ( 'NONE',  ( -24.47390369988710290, -14.86621679291170928, 59.24300234023566247 ) ) ;
#43271 = ORIENTED_EDGE ( 'NONE', *, *, #46225, .T. ) ;
#43272 = CARTESIAN_POINT ( 'NONE',  ( -50.42409385541305511, -14.80920654474410547, 56.99999999999998579 ) ) ;
#43273 = CARTESIAN_POINT ( 'NONE',  ( -11.46043843694620179, -11.04924462883820802, 57.50903212149482613 ) ) ;
#43274 = ORIENTED_EDGE ( 'NONE', *, *, #34342, .T. ) ;
#43275 = CARTESIAN_POINT ( 'NONE',  ( -17.03931138636480824, -19.49188718695241462, 49.52966884056656482 ) ) ;
#43276 = VERTEX_POINT ( 'NONE', #14811 ) ;
#43277 = CARTESIAN_POINT ( 'NONE',  ( -11.73187771999763740, -10.73495407577211580, 74.66558189934212919 ) ) ;
#43278 = CARTESIAN_POINT ( 'NONE',  ( -9.973358241295501969, -14.79494948476079941, 74.98434255746357735 ) ) ;
#43279 = EDGE_LOOP ( 'NONE', ( #5392, #8759, #2815, #18955, #48653 ) ) ;
#43280 = CARTESIAN_POINT ( 'NONE',  ( -17.39761409878557785, -7.809256622337199971, 67.02039592144427615 ) ) ;
#43281 = CARTESIAN_POINT ( 'NONE',  ( -10.76785811675246940, -12.48515291162924434, 57.61385273545094066 ) ) ;
#43282 = B_SPLINE_CURVE_WITH_KNOTS ( 'NONE', 1,
 ( #1229, #23173 ),
 .UNSPECIFIED., .F., .F.,
 ( 2, 2 ),
 ( 0.000000000000000000, 1.000000000000000000 ),
 .UNSPECIFIED. ) ;
#43283 = AXIS2_PLACEMENT_3D ( 'NONE', #44847, #26123, #31513 ) ;
#43284 = CARTESIAN_POINT ( 'NONE',  ( -12.26752988409003642, -16.72227946798956921, 53.49899999999994549 ) ) ;
#43285 = EDGE_LOOP ( 'NONE', ( #28070, #34309, #27307, #19060 ) ) ;
#43286 = CARTESIAN_POINT ( 'NONE',  ( -24.17969144601942233, -17.95015662838525117, 59.04732501252154009 ) ) ;
#43287 = CARTESIAN_POINT ( 'NONE',  ( -10.85795890819061427, -18.96892932606922244, 54.30803469517866944 ) ) ;
#43288 = B_SPLINE_CURVE_WITH_KNOTS ( 'NONE', 1,
 ( #46726, #5614 ),
 .UNSPECIFIED., .F., .F.,
 ( 2, 2 ),
 ( 0.000000000000000000, 1.000000000000000000 ),
 .UNSPECIFIED. ) ;
#43289 = CARTESIAN_POINT ( 'NONE',  ( -11.50273385864769438, -11.07591097799543256, 57.50903212538073461 ) ) ;
#43290 = VERTEX_POINT ( 'NONE', #15806 ) ;
#43291 = CARTESIAN_POINT ( 'NONE',  ( -10.61061218858606914, -11.79566089880681545, 74.69693755219159925 ) ) ;
#43292 = AXIS2_PLACEMENT_3D ( 'NONE', #9705, #21508, #28647 ) ;
#43293 = EDGE_CURVE ( 'NONE', #29409, #9616, #18339, .T. ) ;
#43294 = ORIENTED_EDGE ( 'NONE', *, *, #7330, .F. ) ;
#43295 = ORIENTED_EDGE ( 'NONE', *, *, #42221, .T. ) ;
#43296 = DIRECTION ( 'NONE',  ( -3.071710424422018668E-17, 6.404604876783312462E-16, 1.000000000000000000 ) ) ;
#43297 = FACE_OUTER_BOUND ( 'NONE', #29483, .T. ) ;
#43298 = CARTESIAN_POINT ( 'NONE',  ( -13.18473975798692877, -20.93551490194142062, 58.23145353898504339 ) ) ;
#43299 = CIRCLE ( 'NONE', #11057, 4.686499999999998778 ) ;
#43300 = CARTESIAN_POINT ( 'NONE',  ( -17.85534385650552025, -7.417179338643134834, 52.18511593390279302 ) ) ;
#43301 = CARTESIAN_POINT ( 'NONE',  ( -12.29586577630491995, -9.966054570304006432, 64.32914351779317030 ) ) ;
#43302 = CARTESIAN_POINT ( 'NONE',  ( -19.54382994836049292, -21.48060488537790746, 62.06791645429107263 ) ) ;
#43303 = CARTESIAN_POINT ( 'NONE',  ( -23.62389146642398075, -18.18225743695742835, 72.91935080803692415 ) ) ;
#43304 = B_SPLINE_CURVE_WITH_KNOTS ( 'NONE', 3,
 ( #14288, #39940, #2984, #10628 ),
 .UNSPECIFIED., .F., .F.,
 ( 4, 4 ),
 ( 0.001310108020964425440, 0.002761379516307286858 ),
 .UNSPECIFIED. ) ;
#43305 = B_SPLINE_CURVE_WITH_KNOTS ( 'NONE', 3,
 ( #18113, #6710, #14784, #14536, #13830, #7209, #36709, #33263, #25654, #33505 ),
 .UNSPECIFIED., .F., .F.,
 ( 4, 2, 2, 2, 4 ),
 ( 0.6272669072878462870, 0.7522669073073414703, 0.8772669073268366535, 1.002266907346331948, 1.127266907365827020 ),
 .UNSPECIFIED. ) ;
#43306 = CARTESIAN_POINT ( 'NONE',  ( -8.424093855413053333, -15.80920654474410725, 47.99999999999998579 ) ) ;
#43307 = CARTESIAN_POINT ( 'NONE',  ( -11.26201241829012822, -11.37794026804562009, 68.03353368067536167 ) ) ;
#43308 = VERTEX_POINT ( 'NONE', #8203 ) ;
#43309 = ORIENTED_EDGE ( 'NONE', *, *, #39671, .F. ) ;
#43310 = EDGE_CURVE ( 'NONE', #8530, #33575, #40364, .T. ) ;
#43311 = CARTESIAN_POINT ( 'NONE',  ( -10.58771178721467798, -11.84651422905517926, 74.67185031923813199 ) ) ;
#43312 = DIRECTION ( 'NONE',  ( 0.000000000000000000, 0.000000000000000000, 1.000000000000000000 ) ) ;
#43313 = EDGE_CURVE ( 'NONE', #19312, #48635, #6052, .T. ) ;
#43314 = CARTESIAN_POINT ( 'NONE',  ( -22.91784385541302882, -6.860780111191215447, 51.02154966934360658 ) ) ;
#43315 = CARTESIAN_POINT ( 'NONE',  ( -20.62633693628556486, -21.09014860362536226, 58.65034946679929817 ) ) ;
#43316 = CARTESIAN_POINT ( 'NONE',  ( -22.42700247402090241, -19.70584170416704595, 72.92783938554663337 ) ) ;
#43317 = DIRECTION ( 'NONE',  ( 0.4501286257827957216, 0.8929637284072022840, -1.500157796035321876E-08 ) ) ;
#43318 = ADVANCED_FACE ( 'NONE', ( #48577 ), #4259, .F. ) ;
#43319 = ORIENTED_EDGE ( 'NONE', *, *, #43935, .T. ) ;
#43320 = CARTESIAN_POINT ( 'NONE',  ( -20.10179291524702805, -21.76144317846600629, 72.66124644823618439 ) ) ;
#43321 = CARTESIAN_POINT ( 'NONE',  ( -10.21764033814386963, -12.91954908504599331, 67.92327745040803677 ) ) ;
#43322 = VECTOR ( 'NONE', #14230, 1000.000000000000000 ) ;
#43323 = DIRECTION ( 'NONE',  ( -3.071710424422018668E-17, 6.404604876783312462E-16, 1.000000000000000000 ) ) ;
#43324 = CARTESIAN_POINT ( 'NONE',  ( -17.42409385541300182, -14.80920654474440745, 53.27966884056655061 ) ) ;
#43325 = ORIENTED_EDGE ( 'NONE', *, *, #8088, .F. ) ;
#43326 = CIRCLE ( 'NONE', #29967, 1.999999999999999556 ) ;
#43327 = CARTESIAN_POINT ( 'NONE',  ( -17.00410685006708178, -7.771727545396207582, 73.96018273221115180 ) ) ;
#43328 = B_SPLINE_CURVE_WITH_KNOTS ( 'NONE', 1,
 ( #9584, #5876 ),
 .UNSPECIFIED., .F., .F.,
 ( 2, 2 ),
 ( 0.000000000000000000, 1.000000000000000000 ),
 .UNSPECIFIED. ) ;
#43329 = CARTESIAN_POINT ( 'NONE',  ( -17.65006842549283306, -20.30456235612523841, 54.07175714974878389 ) ) ;
#43330 = CARTESIAN_POINT ( 'NONE',  ( -22.37880076751769920, -9.788815724235030657, 73.68981091303635367 ) ) ;
#43331 = CIRCLE ( 'NONE', #44922, 1.949999999999999734 ) ;
#43332 = DIRECTION ( 'NONE',  ( 1.077913161596394792E-05, -7.121115469840252016E-06, -0.9999999999165499753 ) ) ;
#43333 = CARTESIAN_POINT ( 'NONE',  ( -14.79267687185098268, -7.839273151334183787, 56.97187263562120307 ) ) ;
#43334 = CARTESIAN_POINT ( 'NONE',  ( -20.92409385541305511, -10.60920654474410618, 81.99999999999998579 ) ) ;
#43335 = ORIENTED_EDGE ( 'NONE', *, *, #5615, .F. ) ;
#43336 = CARTESIAN_POINT ( 'NONE',  ( -20.36206934058443352, -7.962967395703286044, 70.35126086822562286 ) ) ;
#43337 = EDGE_LOOP ( 'NONE', ( #48533, #10253, #5914, #23918 ) ) ;
#43338 = CARTESIAN_POINT ( 'NONE',  ( -11.30839666586712688, -19.06371641305695519, 68.41700838957257247 ) ) ;
#43339 = VERTEX_POINT ( 'NONE', #37231 ) ;
#43340 = CARTESIAN_POINT ( 'NONE',  ( -16.32745258320347759, -21.77369344365219561, 61.77040269689842944 ) ) ;
#43341 = CARTESIAN_POINT ( 'NONE',  ( -15.29909385650551634, -8.114302828567740988, 52.18300498402516041 ) ) ;
#43342 = B_SPLINE_CURVE_WITH_KNOTS ( 'NONE', 1,
 ( #28830, #43876 ),
 .UNSPECIFIED., .F., .F.,
 ( 2, 2 ),
 ( 0.000000000000000000, 1.000000000000000000 ),
 .UNSPECIFIED. ) ;
#43343 = ORIENTED_EDGE ( 'NONE', *, *, #40676, .F. ) ;
#43344 = CARTESIAN_POINT ( 'NONE',  ( -20.47409385759799250, -6.859212275519751323, 50.50378509014259265 ) ) ;
#43345 =( BOUNDED_CURVE ( )  B_SPLINE_CURVE ( 3, ( #16660, #41820, #8095, #4378 ),
 .UNSPECIFIED., .F., .F. ) 
 B_SPLINE_CURVE_WITH_KNOTS ( ( 4, 4 ),
 ( 0.5000000000000000000, 0.9074455897393636228 ),
 .UNSPECIFIED. ) 
 CURVE ( )  GEOMETRIC_REPRESENTATION_ITEM ( )  RATIONAL_B_SPLINE_CURVE ( ( 0.9999999999999772404, 0.4567392136813265835, 0.3561768502900441447, 0.6983129098261050549 ) ) 
 REPRESENTATION_ITEM ( '' )  );
#43346 = ADVANCED_FACE ( 'NONE', ( #41193 ), #45383, .F. ) ;
#43347 = CARTESIAN_POINT ( 'NONE',  ( -24.05845721068777010, -12.57644527891515551, 73.54225570276561541 ) ) ;
#43348 = CARTESIAN_POINT ( 'NONE',  ( -16.29919166237813144, -22.17386956490665639, 62.01214078850637890 ) ) ;
#43349 = ORIENTED_EDGE ( 'NONE', *, *, #4934, .T. ) ;
#43350 = DIRECTION ( 'NONE',  ( 1.411223637948141806E-06, 4.279116285847032870E-06, 0.9999999999898486758 ) ) ;
#43351 = CARTESIAN_POINT ( 'NONE',  ( -10.81230840161673790, -17.25685697075765646, 64.64211442681141762 ) ) ;
#43352 = CARTESIAN_POINT ( 'NONE',  ( -12.41315173547891959, -9.850077678253004621, 57.38935532239157311 ) ) ;
#43353 = AXIS2_PLACEMENT_3D ( 'NONE', #5589, #21079, #12719 ) ;
#43354 = CARTESIAN_POINT ( 'NONE',  ( -12.26752988409003642, -16.72227946798956921, 54.07175714974876968 ) ) ;
#43355 = ORIENTED_EDGE ( 'NONE', *, *, #10890, .T. ) ;
#43356 = ORIENTED_EDGE ( 'NONE', *, *, #46058, .F. ) ;
#43357 = AXIS2_PLACEMENT_3D ( 'NONE', #30988, #16911, #19664 ) ;
#43358 = CARTESIAN_POINT ( 'NONE',  ( -24.09792875595538320, -17.08130417324981565, 72.88336032035921619 ) ) ;
#43359 = CARTESIAN_POINT ( 'NONE',  ( -22.11771078617523401, -17.70194497944557455, 53.88362224778187226 ) ) ;
#43360 = ORIENTED_EDGE ( 'NONE', *, *, #43177, .F. ) ;
#43361 = CARTESIAN_POINT ( 'NONE',  ( -24.32752865423570654, -15.96790753223159598, 66.36324927017490438 ) ) ;
#43362 = CARTESIAN_POINT ( 'NONE',  ( -23.25771167494501412, -18.77452406822311559, 62.35406629416942081 ) ) ;
#43363 = CARTESIAN_POINT ( 'NONE',  ( -17.09909385759799250, -8.105421454601382081, 49.25000573077640098 ) ) ;
#43364 = CARTESIAN_POINT ( 'NONE',  ( -23.81923673697547272, -10.98750725051906585, 73.55531620916923430 ) ) ;
#43365 = CARTESIAN_POINT ( 'NONE',  ( -24.72409385541305582, -15.80920654474410725, 65.99999999999998579 ) ) ;
#43366 = CARTESIAN_POINT ( 'NONE',  ( -12.26902398874117495, -19.54473763108856943, 58.22682373989366766 ) ) ;
#43367 = AXIS2_PLACEMENT_3D ( 'NONE', #29441, #33111, #10256 ) ;
#43368 = ORIENTED_EDGE ( 'NONE', *, *, #19904, .T. ) ;
#43369 = CARTESIAN_POINT ( 'NONE',  ( -14.90981300391231024, -21.39562377109201208, 61.63600440604547970 ) ) ;
#43370 = EDGE_CURVE ( 'NONE', #34219, #33529, #45419, .T. ) ;
#43371 = AXIS2_PLACEMENT_3D ( 'NONE', #46155, #16584, #9219 ) ;
#43372 = CARTESIAN_POINT ( 'NONE',  ( -12.52712847051791378, -9.194636617869647921, 74.36277061998997340 ) ) ;
#43373 = CARTESIAN_POINT ( 'NONE',  ( -13.54291793993416348, -20.63484089686539846, 61.81646374971770541 ) ) ;
#43374 = ADVANCED_FACE ( 'NONE', ( #30617 ), #11395, .T. ) ;
#43375 = ORIENTED_EDGE ( 'NONE', *, *, #1774, .F. ) ;
#43376 = EDGE_LOOP ( 'NONE', ( #494, #39945, #23309, #34130 ) ) ;
#43377 = EDGE_CURVE ( 'NONE', #24336, #29465, #39555, .T. ) ;
#43378 = ORIENTED_EDGE ( 'NONE', *, *, #3307, .F. ) ;
#43379 = DIRECTION ( 'NONE',  ( 0.6205284308219183309, 0.7841839494287597967, -8.002013567987250328E-17 ) ) ;
#43380 = CARTESIAN_POINT ( 'NONE',  ( -18.53201708017407157, -7.846807123103141102, 74.14064401780551350 ) ) ;
#43381 = EDGE_CURVE ( 'NONE', #2631, #12097, #40949, .T. ) ;
#43382 = ORIENTED_EDGE ( 'NONE', *, *, #29669, .F. ) ;
#43383 = EDGE_CURVE ( 'NONE', #10750, #47624, #7235, .T. ) ;
#43384 = CARTESIAN_POINT ( 'NONE',  ( -15.68502974777997316, -7.977065180327442384, 70.90989839958919561 ) ) ;
#43385 = CIRCLE ( 'NONE', #10341, 2.500000000000000444 ) ;
#43386 = CARTESIAN_POINT ( 'NONE',  ( -10.43298842381219238, -15.77843866184169208, 57.72359922229868801 ) ) ;
#43387 = EDGE_LOOP ( 'NONE', ( #27241, #18695, #41669, #8411, #16218 ) ) ;
#43388 = AXIS2_PLACEMENT_3D ( 'NONE', #116, #14588, #18304 ) ;
#43389 = CARTESIAN_POINT ( 'NONE',  ( -35.32409385541306079, -8.109206544744111511, 51.54999999999998295 ) ) ;
#43390 = CARTESIAN_POINT ( 'NONE',  ( -12.54407977911866290, -20.43842634917980661, 71.90630053519338105 ) ) ;
#43391 = ORIENTED_EDGE ( 'NONE', *, *, #19223, .F. ) ;
#43392 =( BOUNDED_CURVE ( )  B_SPLINE_CURVE ( 3, ( #46883, #46654, #13123, #28174 ),
 .UNSPECIFIED., .F., .F. ) 
 B_SPLINE_CURVE_WITH_KNOTS ( ( 4, 4 ),
 ( 0.9074455897393605142, 1.000000000000000000 ),
 .UNSPECIFIED. ) 
 CURVE ( )  GEOMETRIC_REPRESENTATION_ITEM ( )  RATIONAL_B_SPLINE_CURVE ( ( 0.6983129098260745238, 0.7760317562606822150, 0.8765941196519907441, 1.000000000000000000 ) ) 
 REPRESENTATION_ITEM ( '' )  );
#43393 = CARTESIAN_POINT ( 'NONE',  ( -23.38410589725464916, -10.33907962427212190, 59.71708035543083071 ) ) ;
#43394 = ORIENTED_EDGE ( 'NONE', *, *, #43585, .T. ) ;
#43395 = CARTESIAN_POINT ( 'NONE',  ( -10.56492483649129710, -13.18000429128331596, 71.50828586225091499 ) ) ;
#43396 = ORIENTED_EDGE ( 'NONE', *, *, #40384, .F. ) ;
#43397 = CARTESIAN_POINT ( 'NONE',  ( -11.91924650590474855, -19.82915612511634862, 58.12020671644349790 ) ) ;
#43398 = CARTESIAN_POINT ( 'NONE',  ( -18.22409385759798894, -9.359200813967568422, 50.49621490985803263 ) ) ;
#43399 = PLANE ( 'NONE',  #6893 ) ;
#43400 = ORIENTED_EDGE ( 'NONE', *, *, #9178, .T. ) ;
#43401 = CYLINDRICAL_SURFACE ( 'NONE', #46674, 1.250000000000001110 ) ;
#43402 = CARTESIAN_POINT ( 'NONE',  ( -24.68275054790482770, -16.48720572190336853, 59.23837039904986312 ) ) ;
#43403 = CARTESIAN_POINT ( 'NONE',  ( -22.78034385650551741, -6.424090610841176385, 49.80797279389978627 ) ) ;
#43404 = CIRCLE ( 'NONE', #35507, 5.249999999999998224 ) ;
#43405 = ADVANCED_FACE ( 'NONE', ( #37476 ), #22239, .T. ) ;
#43406 = CARTESIAN_POINT ( 'NONE',  ( -17.73224099643095286, -22.30287356026373047, 54.27966884056655061 ) ) ;
#43407 = DIRECTION ( 'NONE',  ( 0.9687793358424817702, -0.2479245821708686570, 0.000000000000000000 ) ) ;
#43408 = PLANE ( 'NONE',  #18773 ) ;
#43409 = VERTEX_POINT ( 'NONE', #33531 ) ;
#43411 = CARTESIAN_POINT ( 'NONE',  ( -24.42668993457695592, -13.99045928592870780, 73.40799407547365263 ) ) ;
#43410 =( BOUNDED_CURVE ( )  B_SPLINE_CURVE ( 3, ( #41963, #23251, #8004, #30162 ),
 .UNSPECIFIED., .F., .F. ) 
 B_SPLINE_CURVE_WITH_KNOTS ( ( 4, 4 ),
 ( 0.9074455897393632897, 1.000000000000000000 ),
 .UNSPECIFIED. ) 
 CURVE ( )  GEOMETRIC_REPRESENTATION_ITEM ( )  RATIONAL_B_SPLINE_CURVE ( ( 0.6983129098260799639, 0.7760317562606869890, 0.8765941196519936307, 1.000000000000000000 ) ) 
 REPRESENTATION_ITEM ( '' )  );
#43412 = CARTESIAN_POINT ( 'NONE',  ( -11.84391856442395863, -19.03561180790773832, 71.97220474003518120 ) ) ;
#43413 = FACE_OUTER_BOUND ( 'NONE', #30374, .T. ) ;
#43414 = CYLINDRICAL_SURFACE ( 'NONE', #28941, 0.1500000000000028533 ) ;
#43415 = DIRECTION ( 'NONE',  ( -0.9687793358424819923, 0.2479245821708680464, 0.000000000000000000 ) ) ;
#43416 = CARTESIAN_POINT ( 'NONE',  ( -13.97409385650551528, -9.792211528768506312, 50.49490371617623197 ) ) ;
#43417 = VERTEX_POINT ( 'NONE', #29877 ) ;
#43418 = CARTESIAN_POINT ( 'NONE',  ( -21.00733138479494855, -11.77013360165372013, 49.52966884056655772 ) ) ;
#43419 = CARTESIAN_POINT ( 'NONE',  ( -24.83245720896766073, -15.59649170587275258, 73.04657806100746598 ) ) ;
#43420 = VERTEX_POINT ( 'NONE', #31083 ) ;
#43421 = CARTESIAN_POINT ( 'NONE',  ( -11.29385091374517458, -19.04286921470785288, 68.33194352083310719 ) ) ;
#43422 = DIRECTION ( 'NONE',  ( -6.867234345585437148E-33, 2.395284034871317367E-16, -1.000000000000000000 ) ) ;
#43423 = CARTESIAN_POINT ( 'NONE',  ( -14.50361122469707986, -8.447475796767067280, 63.86266978723202925 ) ) ;
#43424 = CARTESIAN_POINT ( 'NONE',  ( -13.71338950266841472, -20.80363499509022773, 64.98628881289567971 ) ) ;
#43425 = DIRECTION ( 'NONE',  ( 1.066846710266752623E-06, -9.113387007412332089E-06, -0.9999999999579038956 ) ) ;
#43426 = ORIENTED_EDGE ( 'NONE', *, *, #37266, .T. ) ;
#43427 = EDGE_CURVE ( 'NONE', #30899, #48422, #6060, .T. ) ;
#43428 = DIRECTION ( 'NONE',  ( 1.000000000000000000, -4.164305804376849172E-17, 1.614929280266638808E-16 ) ) ;
#43429 = CARTESIAN_POINT ( 'NONE',  ( -22.63008543824757979, -10.12971389395683097, 70.01178520543939499 ) ) ;
#43430 = ORIENTED_EDGE ( 'NONE', *, *, #38739, .F. ) ;
#43431 = CARTESIAN_POINT ( 'NONE',  ( -15.50784783684063051, -8.076599273749138774, 74.07985659288991087 ) ) ;
#43432 = AXIS2_PLACEMENT_3D ( 'NONE', #6417, #17484, #47307 ) ;
#43433 = CARTESIAN_POINT ( 'NONE',  ( -12.23220172533774885, -19.57856247689574403, 57.92682373937842044 ) ) ;
#43434 = CARTESIAN_POINT ( 'NONE',  ( -24.18334793769576407, -17.94238558166073716, 59.12565671406948553 ) ) ;
#43435 = CARTESIAN_POINT ( 'NONE',  ( -11.10681587527927938, -11.67891925637714223, 71.10332952723315714 ) ) ;
#43436 = CARTESIAN_POINT ( 'NONE',  ( -16.55445166459533368, -21.75508766523052628, 65.22564429726746482 ) ) ;
#43437 = ORIENTED_EDGE ( 'NONE', *, *, #15861, .T. ) ;
#43438 = ORIENTED_EDGE ( 'NONE', *, *, #44259, .T. ) ;
#43439 = CARTESIAN_POINT ( 'NONE',  ( -18.47409385541304161, -6.859212275519751323, 50.50378509014259265 ) ) ;
#43440 = EDGE_CURVE ( 'NONE', #3060, #46704, #14843, .T. ) ;
#43441 = DIRECTION ( 'NONE',  ( 0.000000000000000000, 0.000000000000000000, -1.000000000000000000 ) ) ;
#43442 = EDGE_CURVE ( 'NONE', #45009, #26785, #23793, .T. ) ;
#43443 = CARTESIAN_POINT ( 'NONE',  ( -15.17160733334415212, -8.120315110694912519, 74.23552617732688930 ) ) ;
#43444 = ADVANCED_FACE ( 'NONE', ( #34776 ), #9166, .F. ) ;
#43445 = CARTESIAN_POINT ( 'NONE',  ( -20.00946575929301474, -8.250368826910309039, 74.02096600124984604 ) ) ;
#43446 = CARTESIAN_POINT ( 'NONE',  ( -14.03825670519393753, -20.93587830947642914, 68.56511064978960235 ) ) ;
#43447 = VERTEX_POINT ( 'NONE', #20004 ) ;
#43448 = CARTESIAN_POINT ( 'NONE',  ( -19.31536540323461182, -22.01519918219321781, 58.71845705497510437 ) ) ;
#43449 = CARTESIAN_POINT ( 'NONE',  ( -10.40888613812686359, -14.10966362093629378, 61.06821293886368807 ) ) ;
#43450 = ORIENTED_EDGE ( 'NONE', *, *, #24228, .T. ) ;
#43451 = CARTESIAN_POINT ( 'NONE',  ( -50.42609385541305755, -14.80920654474413745, 60.01764705882352047 ) ) ;
#43452 = EDGE_CURVE ( 'NONE', #4090, #13117, #47771, .T. ) ;
#43453 = DIRECTION ( 'NONE',  ( -0.9789991564298998750, -0.2038642972899922245, 4.410747590293501250E-08 ) ) ;
#43454 = ADVANCED_FACE ( 'NONE', ( #13074 ), #1690, .T. ) ;
#43456 = VERTEX_POINT ( 'NONE', #39189 ) ;
#43455 =( BOUNDED_CURVE ( )  B_SPLINE_CURVE ( 3, ( #41433, #11643, #46110, #23724 ),
 .UNSPECIFIED., .F., .F. ) 
 B_SPLINE_CURVE_WITH_KNOTS ( ( 4, 4 ),
 ( 0.000000000000000000, 0.4074455897393601256 ),
 .UNSPECIFIED. ) 
 CURVE ( )  GEOMETRIC_REPRESENTATION_ITEM ( )  RATIONAL_B_SPLINE_CURVE ( ( 1.000000000000000000, 0.4567392136813438475, 0.3561768502900347078, 0.6983129098260726364 ) ) 
 REPRESENTATION_ITEM ( '' )  );
#43457 = DIRECTION ( 'NONE',  ( 0.000000000000000000, 0.000000000000000000, 1.000000000000000000 ) ) ;
#43458 = CARTESIAN_POINT ( 'NONE',  ( -10.40277073914389661, -15.44443991871667343, 57.56792809063193772 ) ) ;
#43459 = ADVANCED_FACE ( 'NONE', ( #23717 ), #16042, .T. ) ;
#43461 = EDGE_CURVE ( 'NONE', #44694, #4434, #5477, .T. ) ;
#43460 = ORIENTED_EDGE ( 'NONE', *, *, #42205, .F. ) ;
#43462 = LINE ( 'NONE', #1336, #46648 ) ;
#43463 = CARTESIAN_POINT ( 'NONE',  ( -17.57409385541300395, -6.859212275519753099, 50.50378509014294792 ) ) ;
#43464 = CARTESIAN_POINT ( 'NONE',  ( -46.92409385541305511, -14.80920654474410547, 61.49999999999999289 ) ) ;
#43465 = CARTESIAN_POINT ( 'NONE',  ( -13.92409385541305511, -10.10920654474410618, 81.49999999999998579 ) ) ;
#43466 = ORIENTED_EDGE ( 'NONE', *, *, #25951, .T. ) ;
#43467 = CARTESIAN_POINT ( 'NONE',  ( -14.36817892824948473, -8.455618309860652104, 67.54503025475186462 ) ) ;
#43468 = CARTESIAN_POINT ( 'NONE',  ( -22.33041860316855320, -20.41560964288588664, 62.34943852502606632 ) ) ;
#43469 = CARTESIAN_POINT ( 'NONE',  ( -11.05034076241727625, -11.79557573020262318, 71.37388789199357575 ) ) ;
#43470 = CARTESIAN_POINT ( 'NONE',  ( -11.29385027892729987, -19.04286830487734861, 68.33194243210506613 ) ) ;
#43471 = CONTEXT_DEPENDENT_SHAPE_REPRESENTATION ( #23104, #18503 ) ;
#43472 = B_SPLINE_CURVE_WITH_KNOTS ( 'NONE', 3,
 ( #31359, #12880, #46390, #31612, #20283, #38499, #23254, #46636, #4525, #27183 ),
 .UNSPECIFIED., .F., .F.,
 ( 4, 2, 2, 2, 4 ),
 ( 0.000000000000000000, 0.2500000000000000000, 0.5000000000000000000, 0.7500000000000000000, 1.000000000000000000 ),
 .UNSPECIFIED. ) ;
#43473 = CARTESIAN_POINT ( 'NONE',  ( -20.32146343473794303, -8.373352561929221949, 73.86529255602565058 ) ) ;
#43474 = CARTESIAN_POINT ( 'NONE',  ( -11.44117050972369221, -11.17454573989694921, 60.96269276219595667 ) ) ;
#43475 = B_SPLINE_CURVE_WITH_KNOTS ( 'NONE', 1,
 ( #43502, #20841 ),
 .UNSPECIFIED., .F., .F.,
 ( 2, 2 ),
 ( 0.000000000000000000, 1.000000000000000000 ),
 .UNSPECIFIED. ) ;
#43476 = CARTESIAN_POINT ( 'NONE',  ( -16.16221056564778991, -7.466773990862017207, 60.24382527849350311 ) ) ;
#43477 = CARTESIAN_POINT ( 'NONE',  ( -23.46260449798628045, -11.17067817067885649, 73.51193301756617871 ) ) ;
#43478 = ORIENTED_EDGE ( 'NONE', *, *, #36128, .F. ) ;
#43479 = DIRECTION ( 'NONE',  ( 1.224646799147353207E-16, 1.000000000000000000, -1.912410701131276611E-32 ) ) ;
#43480 = CARTESIAN_POINT ( 'NONE',  ( -20.09379292320953425, -21.76456661724738950, 72.58291472526767052 ) ) ;
#43481 = CARTESIAN_POINT ( 'NONE',  ( -13.26872317195175199, -21.05283485551296607, 47.99999999999994316 ) ) ;
#43482 = ORIENTED_EDGE ( 'NONE', *, *, #13189, .T. ) ;
#43483 = CARTESIAN_POINT ( 'NONE',  ( -19.86401518824997225, -21.42384811948916834, 69.22010401872219632 ) ) ;
#43484 = ORIENTED_EDGE ( 'NONE', *, *, #8134, .T. ) ;
#43485 = EDGE_CURVE ( 'NONE', #41320, #10012, #5720, .T. ) ;
#43486 = ORIENTED_EDGE ( 'NONE', *, *, #27622, .T. ) ;
#43487 = VERTEX_POINT ( 'NONE', #2006 ) ;
#43488 = B_SPLINE_CURVE_WITH_KNOTS ( 'NONE', 3,
 ( #16107, #12681, #27702, #42733, #39752, #42965, #2325, #2573, #12915, #39999 ),
 .UNSPECIFIED., .F., .F.,
 ( 4, 2, 2, 2, 4 ),
 ( 0.000000000000000000, 0.2500000000000000000, 0.5000000000000000000, 0.7500000000000000000, 1.000000000000000000 ),
 .UNSPECIFIED. ) ;
#43489 = CARTESIAN_POINT ( 'NONE',  ( -17.42409385541300892, -14.80920654474439679, 47.99999999999994316 ) ) ;
#43490 = DIRECTION ( 'NONE',  ( 0.9640890753730593232, -0.2655790932026004803, 6.310348465037888425E-08 ) ) ;
#43491 = DIRECTION ( 'NONE',  ( 0.9687793358424821033, -0.2479245821708677133, 0.000000000000000000 ) ) ;
#43492 = DIRECTION ( 'NONE',  ( 0.9687793358424823253, -0.2479245821708663811, 0.000000000000000000 ) ) ;
#43493 = CARTESIAN_POINT ( 'NONE',  ( -22.72031779163844689, -16.29245029320677673, 53.49999999999995026 ) ) ;
#43494 = VERTEX_POINT ( 'NONE', #14268 ) ;
#43495 = ORIENTED_EDGE ( 'NONE', *, *, #47646, .T. ) ;
#43496 = CARTESIAN_POINT ( 'NONE',  ( -18.05534385650551599, -7.417179338643134834, 52.18511593390279302 ) ) ;
#43497 = EDGE_CURVE ( 'NONE', #40716, #29465, #14234, .T. ) ;
#43498 = CARTESIAN_POINT ( 'NONE',  ( -21.06634951290973845, -21.30826427787840771, 62.29966696806321380 ) ) ;
#43499 = CARTESIAN_POINT ( 'NONE',  ( -24.09293239453862512, -16.93698224962508547, 72.95624128829483368 ) ) ;
#43500 = CARTESIAN_POINT ( 'NONE',  ( -19.74284385650551599, -8.811426318492348031, 52.18089403414751359 ) ) ;
#43501 = ORIENTED_EDGE ( 'NONE', *, *, #17824, .F. ) ;
#43502 = CARTESIAN_POINT ( 'NONE',  ( -10.37382936219775154, -14.83089353207902228, 74.81251018390588570 ) ) ;
#43504 = LINE ( 'NONE', #28482, #32320 ) ;
#43503 = B_SPLINE_CURVE_WITH_KNOTS ( 'NONE', 3,
 ( #42861, #1010, #23421, #27104, #20456, #46318, #12572, #4704, #9375, #9131 ),
 .UNSPECIFIED., .F., .F.,
 ( 4, 2, 2, 2, 4 ),
 ( 0.000000000000000000, 0.2500000000000000000, 0.5000000000000000000, 0.7500000000000000000, 1.000000000000000000 ),
 .UNSPECIFIED. ) ;
#43505 = VERTEX_POINT ( 'NONE', #13788 ) ;
#43506 = LINE ( 'NONE', #32644, #9973 ) ;
#43507 = CARTESIAN_POINT ( 'NONE',  ( -10.72552571836178181, -12.61109718544098790, 60.79853568372240602 ) ) ;
#43508 = CARTESIAN_POINT ( 'NONE',  ( -20.78299823145727387, -8.610459808214880439, 59.85597358678664648 ) ) ;
#43509 = ADVANCED_FACE ( 'NONE', ( #47324 ), #6433, .T. ) ;
#43510 = EDGE_CURVE ( 'NONE', #4674, #37124, #46548, .T. ) ;
#43511 = CARTESIAN_POINT ( 'NONE',  ( -18.85724798917316392, -7.906108138700305155, 67.18599644112759961 ) ) ;
#43512 = VECTOR ( 'NONE', #44713, 1000.000000000000114 ) ;
#43513 = ORIENTED_EDGE ( 'NONE', *, *, #45159, .F. ) ;
#43514 = DIRECTION ( 'NONE',  ( -0.9000732436326450703, -0.4357386327795698677, 2.072980810273451787E-08 ) ) ;
#43515 = CARTESIAN_POINT ( 'NONE',  ( -22.75539019595755263, -10.19575032747719590, 66.82710158566565894 ) ) ;
#43516 = DIRECTION ( 'NONE',  ( -3.071710424422018668E-17, 6.404604876783312462E-16, 1.000000000000000000 ) ) ;
#43517 = ORIENTED_EDGE ( 'NONE', *, *, #5999, .T. ) ;
#43518 = CARTESIAN_POINT ( 'NONE',  ( -15.61111608319569477, -19.14379616117205885, 52.02966884056656482 ) ) ;
#43519 = VERTEX_POINT ( 'NONE', #6909 ) ;
#43520 = DIRECTION ( 'NONE',  ( -2.866981220435666553E-17, 1.000000000000000000, 1.190614954331866791E-16 ) ) ;
#43521 = EDGE_CURVE ( 'NONE', #41728, #2374, #17725, .T. ) ;
#43522 = EDGE_CURVE ( 'NONE', #29624, #8171, #24825, .T. ) ;
#43523 = CARTESIAN_POINT ( 'NONE',  ( -10.37051006938303388, -14.56035623187037942, 74.94211941000891386 ) ) ;
#43524 = ORIENTED_EDGE ( 'NONE', *, *, #30844, .T. ) ;
#43525 = FACE_OUTER_BOUND ( 'NONE', #15578, .T. ) ;
#43526 = CARTESIAN_POINT ( 'NONE',  ( -21.88020070643341697, -20.20778541568678932, 58.76442927266135285 ) ) ;
#43527 = CARTESIAN_POINT ( 'NONE',  ( -24.46557908765160860, -17.24254831546467415, 73.13981945087590475 ) ) ;
#43528 = CARTESIAN_POINT ( 'NONE',  ( -21.20587034079417776, -21.22798937808393660, 65.78465149344722818 ) ) ;
#43529 = ORIENTED_EDGE ( 'NONE', *, *, #39547, .T. ) ;
#43530 = CARTESIAN_POINT ( 'NONE',  ( -21.94239013569476171, -20.22099906679998327, 58.76442899523448204 ) ) ;
#43531 = UNCERTAINTY_MEASURE_WITH_UNIT (LENGTH_MEASURE( 1.000000000000000082E-05 ), #30536, 'distance_accuracy_value', 'NONE');
#43532 =( BOUNDED_CURVE ( )  B_SPLINE_CURVE ( 3, ( #14840, #14354, #8001, #22509 ),
 .UNSPECIFIED., .F., .F. ) 
 B_SPLINE_CURVE_WITH_KNOTS ( ( 4, 4 ),
 ( 0.4074455897393626236, 0.5000000000000000000 ),
 .UNSPECIFIED. ) 
 CURVE ( )  GEOMETRIC_REPRESENTATION_ITEM ( )  RATIONAL_B_SPLINE_CURVE ( ( 0.6983129098260836276, 0.7760317562606876551, 0.8765941196519922984, 0.9999999999999961142 ) ) 
 REPRESENTATION_ITEM ( '' )  );
#43533 = CARTESIAN_POINT ( 'NONE',  ( -14.78754716229542865, -8.270772359302402066, 60.31996282000578447 ) ) ;
#43534 = CARTESIAN_POINT ( 'NONE',  ( -23.42532328873747005, -19.22384396101403681, 62.46911485589509994 ) ) ;
#43535 = EDGE_LOOP ( 'NONE', ( #41293, #30133 ) ) ;
#43536 = LINE ( 'NONE', #2399, #350 ) ;
#43537 = CARTESIAN_POINT ( 'NONE',  ( -24.25486363958986757, -13.06355980472538292, 63.11792038370487035 ) ) ;
#43538 = EDGE_CURVE ( 'NONE', #21212, #22802, #6720, .T. ) ;
#43539 = ORIENTED_EDGE ( 'NONE', *, *, #25234, .F. ) ;
#43540 = ORIENTED_EDGE ( 'NONE', *, *, #42091, .T. ) ;
#43541 = CARTESIAN_POINT ( 'NONE',  ( -20.66696855643225561, -21.06909979829504209, 58.94475164909854925 ) ) ;
#43542 = FACE_OUTER_BOUND ( 'NONE', #26286, .T. ) ;
#43543 = CARTESIAN_POINT ( 'NONE',  ( -10.02022215050942577, -15.63848034003142295, 61.17755693646328297 ) ) ;
#43544 = CARTESIAN_POINT ( 'NONE',  ( -16.95534385650551812, -7.417179338643134834, 52.18511593390279302 ) ) ;
#43545 = CARTESIAN_POINT ( 'NONE',  ( -21.89218479126588335, -8.847617444388541585, 66.83866863626586508 ) ) ;
#43546 = CARTESIAN_POINT ( 'NONE',  ( -24.41553149706675896, -15.71832598455623398, 69.81835354388927328 ) ) ;
#43547 =( BOUNDED_CURVE ( )  B_SPLINE_CURVE ( 3, ( #17473, #32502, #31778, #39156 ),
 .UNSPECIFIED., .F., .F. ) 
 B_SPLINE_CURVE_WITH_KNOTS ( ( 4, 4 ),
 ( 0.000000000000000000, 0.4074455897393658987 ),
 .UNSPECIFIED. ) 
 CURVE ( )  GEOMETRIC_REPRESENTATION_ITEM ( )  RATIONAL_B_SPLINE_CURVE ( ( 1.000000000000000000, 0.4567392136813347991, 0.3561768502900313216, 0.6983129098260896228 ) ) 
 REPRESENTATION_ITEM ( '' )  );
#43548 = DIRECTION ( 'NONE',  ( 0.000000000000000000, 0.000000000000000000, -1.000000000000000000 ) ) ;
#43549 = CARTESIAN_POINT ( 'NONE',  ( -10.13258936719380898, -16.33817337277914561, 71.63245765104117879 ) ) ;
#43550 =( BOUNDED_CURVE ( )  B_SPLINE_CURVE ( 3, ( #10432, #10903, #45145, #26175 ),
 .UNSPECIFIED., .F., .F. ) 
 B_SPLINE_CURVE_WITH_KNOTS ( ( 4, 4 ),
 ( 0.4074455897393624570, 0.5000000000000000000 ),
 .UNSPECIFIED. ) 
 CURVE ( )  GEOMETRIC_REPRESENTATION_ITEM ( )  RATIONAL_B_SPLINE_CURVE ( ( 0.6983129098261117162, 0.7760317562607033093, 0.8765941196519960732, 0.9999999999999825695 ) ) 
 REPRESENTATION_ITEM ( '' )  );
#43551 = CARTESIAN_POINT ( 'NONE',  ( -18.95165573079047761, -7.922886716408846119, 70.67068327992531351 ) ) ;
#43552 = VERTEX_POINT ( 'NONE', #13555 ) ;
#43553 = EDGE_LOOP ( 'NONE', ( #18702, #47469 ) ) ;
#43554 = CARTESIAN_POINT ( 'NONE',  ( -24.39416267077224987, -15.91966209353573802, 73.14736799148198543 ) ) ;
#43555 = VECTOR ( 'NONE', #29216, 1000.000000000000000 ) ;
#43556 = CARTESIAN_POINT ( 'NONE',  ( -21.91034708787274710, -20.18261625685872218, 59.06442899735736773 ) ) ;
#43557 = CARTESIAN_POINT ( 'NONE',  ( -19.93475561761363934, -21.40553454266635569, 65.62053285436006433 ) ) ;
#43558 = CARTESIAN_POINT ( 'NONE',  ( -13.41424841794075462, -8.530288970272771110, 57.22613703607469660 ) ) ;
#43559 = CARTESIAN_POINT ( 'NONE',  ( -13.54823083431842612, -20.69819501703281617, 61.66646323538943619 ) ) ;
#43560 = CARTESIAN_POINT ( 'NONE',  ( -21.17409385650551812, -9.792211528768504536, 50.49490371617623197 ) ) ;
#43561 =( BOUNDED_CURVE ( )  B_SPLINE_CURVE ( 3, ( #22603, #48447, #16098, #37601 ),
 .UNSPECIFIED., .F., .F. ) 
 B_SPLINE_CURVE_WITH_KNOTS ( ( 4, 4 ),
 ( 0.9074455897393652881, 1.000000000000000000 ),
 .UNSPECIFIED. ) 
 CURVE ( )  GEOMETRIC_REPRESENTATION_ITEM ( )  RATIONAL_B_SPLINE_CURVE ( ( 0.6983129098260858481, 0.7760317562606919850, 0.8765941196519967393, 1.000000000000000000 ) ) 
 REPRESENTATION_ITEM ( '' )  );
#43562 = VERTEX_POINT ( 'NONE', #502 ) ;
#43563 = CARTESIAN_POINT ( 'NONE',  ( -17.42409385541305511, -14.80920654474410725, 47.99999999999998579 ) ) ;
#43564 = PLANE ( 'NONE',  #33157 ) ;
#43565 = CARTESIAN_POINT ( 'NONE',  ( -17.63866254341385442, -7.362211269489866261, 63.66561597723832477 ) ) ;
#43566 = CARTESIAN_POINT ( 'NONE',  ( -10.44761804341386124, -15.84536169652562343, 60.92300268024614240 ) ) ;
#43567 = EDGE_LOOP ( 'NONE', ( #31607, #25869, #19793, #12713, #60 ) ) ;
#43568 = CARTESIAN_POINT ( 'NONE',  ( -13.71339110807025641, -20.80363600241853561, 65.13628881288371986 ) ) ;
#43569 = DIRECTION ( 'NONE',  ( 0.000000000000000000, 0.9999954153791273948, 0.003028072113819836077 ) ) ;
#43570 = EDGE_CURVE ( 'NONE', #31120, #1645, #44589, .T. ) ;
#43571 = LINE ( 'NONE', #24617, #46206 ) ;
#43572 = CARTESIAN_POINT ( 'NONE',  ( -24.45714095472541771, -14.31630891555219165, 69.66747352629326429 ) ) ;
#43573 = CARTESIAN_POINT ( 'NONE',  ( -10.82029165754025257, -17.28804506987337675, 68.39721911992690195 ) ) ;
#43574 = ORIENTED_EDGE ( 'NONE', *, *, #24223, .F. ) ;
#43575 = CARTESIAN_POINT ( 'NONE',  ( -20.87058393588507244, -20.90343486309737031, 65.65624275338501548 ) ) ;
#43576 = VERTEX_POINT ( 'NONE', #4203 ) ;
#43577 = AXIS2_PLACEMENT_3D ( 'NONE', #32728, #32267, #36412 ) ;
#43578 = CARTESIAN_POINT ( 'NONE',  ( -23.85748962928175132, -11.92509172808648543, 59.49707787073156595 ) ) ;
#43579 = EDGE_CURVE ( 'NONE', #44745, #44593, #7414, .T. ) ;
#43580 = EDGE_CURVE ( 'NONE', #34640, #45327, #19210, .T. ) ;
#43581 = CARTESIAN_POINT ( 'NONE',  ( -14.79284385759798859, -8.630756214087126565, 51.74842643355248129 ) ) ;
#43582 = VERTEX_POINT ( 'NONE', #26606 ) ;
#43583 = CARTESIAN_POINT ( 'NONE',  ( -17.39591213481957155, -7.359259842313431221, 67.17039592573394202 ) ) ;
#43584 = VECTOR ( 'NONE', #3790, 1000.000000000000000 ) ;
#43585 = EDGE_CURVE ( 'NONE', #7661, #48493, #4510, .T. ) ;
#43586 = CARTESIAN_POINT ( 'NONE',  ( -14.96159385650551776, -9.295667164867525756, 49.30633214617472504 ) ) ;
#43587 = ORIENTED_EDGE ( 'NONE', *, *, #9551, .F. ) ;
#43588 = CARTESIAN_POINT ( 'NONE',  ( -27.42409385541305511, -10.10920654474410618, 79.49999999999998579 ) ) ;
#43589 = ADVANCED_FACE ( 'NONE', ( #11577 ), #38151, .F. ) ;
#43590 = CARTESIAN_POINT ( 'NONE',  ( -24.08343201129240185, -12.65065468682437100, 73.25842202001697956 ) ) ;
#43591 = CARTESIAN_POINT ( 'NONE',  ( -10.90988520595749023, -17.37161216853074919, 64.64241850740873474 ) ) ;
#43592 = EDGE_LOOP ( 'NONE', ( #20128, #18409, #498, #24427, #38096 ) ) ;
#43593 = DIRECTION ( 'NONE',  ( 4.115385489419834812E-17, 0.9999954153791273948, 0.003028072113822188795 ) ) ;
#43594 = CARTESIAN_POINT ( 'NONE',  ( -10.95719248119807254, -18.50832987904905735, 57.98527366719552845 ) ) ;
#43595 = CARTESIAN_POINT ( 'NONE',  ( -10.65397967773411203, -12.84193750263848521, 64.56276319717653678 ) ) ;
#43596 = DIRECTION ( 'NONE',  ( -1.000000000000000000, 4.164305804376849172E-17, -1.614929280266638808E-16 ) ) ;
#43597 = EDGE_CURVE ( 'NONE', #3423, #27443, #30068, .T. ) ;
#43598 = VERTEX_POINT ( 'NONE', #21 ) ;
#43599 = VERTEX_POINT ( 'NONE', #7170 ) ;
#43600 = CARTESIAN_POINT ( 'NONE',  ( -24.48810908846319734, -17.17637088580320537, 73.06831457992643664 ) ) ;
#43601 = CARTESIAN_POINT ( 'NONE',  ( -10.98557796499954087, -17.68114198556070704, 71.86718193507100239 ) ) ;
#43602 = ORIENTED_EDGE ( 'NONE', *, *, #1575, .F. ) ;
#43603 = DIRECTION ( 'NONE',  ( 4.133538118270764137E-06, -2.214839422975871337E-07, 0.9999999999914324089 ) ) ;
#43604 = CARTESIAN_POINT ( 'NONE',  ( -19.01159385759799036, -8.990409506049200417, 49.61344411288074951 ) ) ;
#43605 = DIRECTION ( 'NONE',  ( -0.000000000000000000, 0.000000000000000000, 1.000000000000000000 ) ) ;
#43606 = CARTESIAN_POINT ( 'NONE',  ( -10.60570763719787735, -17.81143699334987218, 71.68222866232767387 ) ) ;
#43607 = CARTESIAN_POINT ( 'NONE',  ( -24.84449963183508459, -13.71944596863515464, 54.27966884056654351 ) ) ;
#43608 = EDGE_LOOP ( 'NONE', ( #27959, #44402, #45088, #17150 ) ) ;
#43609 = CARTESIAN_POINT ( 'NONE',  ( -20.88147674714181079, -8.209942860146695054, 60.02620543942160225 ) ) ;
#43610 = CARTESIAN_POINT ( 'NONE',  ( -13.00788241525034827, -8.809089704718775948, 64.03133736531236764 ) ) ;
#43611 = CARTESIAN_POINT ( 'NONE',  ( -24.87417961795293664, -14.80849281899037884, 59.42795564617806292 ) ) ;
#43612 = LINE ( 'NONE', #5931, #2544 ) ;
#43613 = VERTEX_POINT ( 'NONE', #14744 ) ;
#43614 = VECTOR ( 'NONE', #28637, 1000.000000000000000 ) ;
#43615 = VERTEX_POINT ( 'NONE', #45090 ) ;
#43616 = DIRECTION ( 'NONE',  ( -3.071710424422018668E-17, 6.404604876783312462E-16, 1.000000000000000000 ) ) ;
#43617 = AXIS2_PLACEMENT_3D ( 'NONE', #23978, #22570, #34801 ) ;
#43618 = CARTESIAN_POINT ( 'NONE',  ( -10.01365112473739316, -14.04198459531795962, 61.02547148049693249 ) ) ;
#43619 = B_SPLINE_CURVE_WITH_KNOTS ( 'NONE', 3,
 ( #8588, #31231, #5379, #12759, #46254, #12512, #27536, #8840, #28013, #23857 ),
 .UNSPECIFIED., .F., .F.,
 ( 4, 2, 2, 2, 4 ),
 ( 0.1272669073658264094, 0.2522669073439470777, 0.3772669073220676905, 0.5022669073001884144, 0.6272669072783090272 ),
 .UNSPECIFIED. ) ;
#43620 = EDGE_CURVE ( 'NONE', #18637, #3366, #23390, .T. ) ;
#43621 = VERTEX_POINT ( 'NONE', #3452 ) ;
#43622 = CARTESIAN_POINT ( 'NONE',  ( -24.26595340233995302, -13.32969406988797623, 59.36267925071750540 ) ) ;
#43623 = CARTESIAN_POINT ( 'NONE',  ( 18.62590614458706995, 0.6407533398239845246, 50.52649563099625851 ) ) ;
#43624 = EDGE_CURVE ( 'NONE', #34217, #24292, #19947, .T. ) ;
#43625 = ORIENTED_EDGE ( 'NONE', *, *, #3132, .F. ) ;
#43626 = CARTESIAN_POINT ( 'NONE',  ( -24.43112999227502868, -15.58634490091466951, 73.00303748142292193 ) ) ;
#43627 =( BOUNDED_SURFACE ( )  B_SPLINE_SURFACE ( 3, 1, ( 
 ( #35932, #1481 ),
 ( #16967, #5189 ),
 ( #31528, #46063 ),
 ( #35209, #42858 ),
 ( #16239, #27344 ),
 ( #42377, #9373 ),
 ( #20197, #8646 ) ),
 .UNSPECIFIED., .T., .F., .F. ) 
 B_SPLINE_SURFACE_WITH_KNOTS ( ( 4, 3, 4 ),
 ( 2, 2 ),
 ( 0.000000000000000000, 0.5000000000000000000, 1.000000000000000000 ),
 ( 0.000000000000000000, 1.000000000000000000 ),
 .UNSPECIFIED. ) 
 GEOMETRIC_REPRESENTATION_ITEM ( )  RATIONAL_B_SPLINE_SURFACE ( (
 ( 1.000000000000000000, 1.000000000000000000),
 ( 0.3333333333333335369, 0.3333333333333330373),
 ( 0.3333333333333335369, 0.3333333333333330373),
 ( 1.000000000000000000, 1.000000000000000000),
 ( 0.3333333333333333703, 0.3333333333333333703),
 ( 0.3333333333333333703, 0.3333333333333333703),
 ( 1.000000000000000000, 1.000000000000000000) ) ) 
 REPRESENTATION_ITEM ( '' )  SURFACE ( )  );
#43628 = CARTESIAN_POINT ( 'NONE',  ( -20.39989816187257077, -8.414049535419632520, 70.34280313098182091 ) ) ;
#43629 = CARTESIAN_POINT ( 'NONE',  ( -45.98959949296581584, -14.20920654474410760, 71.05212771298751306 ) ) ;
#43630 = B_SPLINE_CURVE_WITH_KNOTS ( 'NONE', 1,
 ( #37442, #26637 ),
 .UNSPECIFIED., .F., .F.,
 ( 2, 2 ),
 ( 0.000000000000000000, 1.000000000000000000 ),
 .UNSPECIFIED. ) ;
#43631 = ORIENTED_EDGE ( 'NONE', *, *, #15741, .T. ) ;
#43632 = CARTESIAN_POINT ( 'NONE',  ( -11.85162103594838001, -10.49015045520576983, 71.25420998615621215 ) ) ;
#43633 = ORIENTED_EDGE ( 'NONE', *, *, #44297, .T. ) ;
#43634 = CARTESIAN_POINT ( 'NONE',  ( -16.09584876169039802, -7.477806291315723719, 63.85666425603482566 ) ) ;
#43635 = CARTESIAN_POINT ( 'NONE',  ( -12.36794907275616850, -19.72224022788673636, 61.54678633597969650 ) ) ;
#43636 = B_SPLINE_CURVE_WITH_KNOTS ( 'NONE', 1,
 ( #41703, #34291 ),
 .UNSPECIFIED., .F., .F.,
 ( 2, 2 ),
 ( 0.000000000000000000, 1.000000000000000000 ),
 .UNSPECIFIED. ) ;
#43637 = EDGE_LOOP ( 'NONE', ( #16601, #16830, #25789, #15768 ) ) ;
#43638 = DIRECTION ( 'NONE',  ( 5.828394909737395597E-08, -1.590814177254004958E-07, -0.9999999999999855671 ) ) ;
#43639 = CARTESIAN_POINT ( 'NONE',  ( -10.64854695470030599, -12.86019059820356958, 64.55364013863997741 ) ) ;
#43640 = EDGE_CURVE ( 'NONE', #43552, #23522, #23402, .T. ) ;
#43641 = CARTESIAN_POINT ( 'NONE',  ( -17.03931138636480824, -19.49188718695241107, 52.02966884056656482 ) ) ;
#43642 = EDGE_CURVE ( 'NONE', #30663, #26903, #11761, .T. ) ;
#43643 = DIRECTION ( 'NONE',  ( 1.000000000000000000, 0.000000000000000000, -0.000000000000000000 ) ) ;
#43644 = CARTESIAN_POINT ( 'NONE',  ( 18.57590614458706924, 3.116243883476995880, 50.28399048308531860 ) ) ;
#43645 = CARTESIAN_POINT ( 'NONE',  ( -4.424093855413056886, -27.10920654474410796, 47.99999999999998579 ) ) ;
#43646 = ORIENTED_EDGE ( 'NONE', *, *, #8609, .F. ) ;
#43647 = DIRECTION ( 'NONE',  ( -0.8603395911234872351, -0.5097212845717460361, 0.000000000000000000 ) ) ;
#43648 = CARTESIAN_POINT ( 'NONE',  ( -11.80131277442636240, -10.54314289786156777, 67.65463988879716339 ) ) ;
#43649 = CARTESIAN_POINT ( 'NONE',  ( -16.16909865928699830, -7.465622663876843923, 60.30690150944003136 ) ) ;
#43650 = AXIS2_PLACEMENT_3D ( 'NONE', #20135, #35142, #39331 ) ;
#43651 = CARTESIAN_POINT ( 'NONE',  ( -16.58751095051766455, -21.80939428823196025, 65.22564390318969174 ) ) ;
#43652 = EDGE_CURVE ( 'NONE', #44029, #32817, #16764, .T. ) ;
#43653 = CARTESIAN_POINT ( 'NONE',  ( -17.94284385759799250, -7.587656875400192291, 49.25157356644813689 ) ) ;
#43654 = DIRECTION ( 'NONE',  ( -3.071710424422018668E-17, 6.404604876783312462E-16, 1.000000000000000000 ) ) ;
#43655 = AXIS2_PLACEMENT_3D ( 'NONE', #45517, #4619, #30973 ) ;
#43656 = VERTEX_POINT ( 'NONE', #29556 ) ;
#43657 = VERTEX_POINT ( 'NONE', #40883 ) ;
#43658 = DIRECTION ( 'NONE',  ( -0.2479245821708776221, -0.9687793358424795498, 0.000000000000000000 ) ) ;
#43659 = CARTESIAN_POINT ( 'NONE',  ( -24.32852063849251323, -13.38246526728995001, 59.37740068604990995 ) ) ;
#43660 = EDGE_LOOP ( 'NONE', ( #21217, #5566, #44956, #20831 ) ) ;
#43662 = DIRECTION ( 'NONE',  ( -1.000000000000000000, 4.164305804376849172E-17, -1.614929280266638808E-16 ) ) ;
#43661 = B_SPLINE_CURVE_WITH_KNOTS ( 'NONE', 3,
 ( #19984, #12830, #23441, #4729, #31307, #27850, #46336, #42652, #38934, #8912 ),
 .UNSPECIFIED., .F., .F.,
 ( 4, 2, 2, 2, 4 ),
 ( 0.000000000000000000, 0.2500000000000000000, 0.5000000000000000000, 0.7500000000000000000, 1.000000000000000000 ),
 .UNSPECIFIED. ) ;
#43664 = FACE_OUTER_BOUND ( 'NONE', #33429, .T. ) ;
#43663 = CARTESIAN_POINT ( 'NONE',  ( -10.55855397105558779, -16.42450592920206276, 71.33261492083846633 ) ) ;
#43665 = CARTESIAN_POINT ( 'NONE',  ( -23.12535468111908443, -10.01343724238356359, 66.65686954956312604 ) ) ;
#43666 = CARTESIAN_POINT ( 'NONE',  ( -6.424093855413058662, -25.10920654474410441, 52.99999999999998579 ) ) ;
#43667 = CARTESIAN_POINT ( 'NONE',  ( -10.85938897953544924, -12.23054697885984510, 57.74345952600154419 ) ) ;
#43668 = ADVANCED_FACE ( 'NONE', ( #48508 ), #41366, .F. ) ;
#43669 = VERTEX_POINT ( 'NONE', #18970 ) ;
#43670 = FACE_BOUND ( 'NONE', #32151, .T. ) ;
#43671 = CARTESIAN_POINT ( 'NONE',  ( -24.82668569956033622, -13.96895926810607946, 73.29988393021096726 ) ) ;
#43672 = LINE ( 'NONE', #20762, #20223 ) ;
#43673 = DIRECTION ( 'NONE',  ( -3.071710424422018668E-17, 6.404604876783312462E-16, 1.000000000000000000 ) ) ;
#43674 = ORIENTED_EDGE ( 'NONE', *, *, #18984, .F. ) ;
#43675 = CARTESIAN_POINT ( 'NONE',  ( -10.38078067960954520, -14.50222210708341741, 68.15800126083217947 ) ) ;
#43676 = FILL_AREA_STYLE_COLOUR ( '', #37640 ) ;
#43677 = CARTESIAN_POINT ( 'NONE',  ( -17.00410561000564513, -7.771727611841390271, 74.26018273220857679 ) ) ;
#43678 = CARTESIAN_POINT ( 'NONE',  ( -21.08710395203513244, -20.77481533096753452, 69.07066874357158781 ) ) ;
#43679 = CARTESIAN_POINT ( 'NONE',  ( -21.41370985594940990, -18.61458953632344659, 53.88362224778186516 ) ) ;
#43680 = CARTESIAN_POINT ( 'NONE',  ( -15.87557486115803052, -7.931373420853708112, 67.44007279014866185 ) ) ;
#43681 = EDGE_LOOP ( 'NONE', ( #2712, #37256, #22134, #41916 ) ) ;
#43682 = ORIENTED_EDGE ( 'NONE', *, *, #41610, .F. ) ;
#43683 = CARTESIAN_POINT ( 'NONE',  ( -18.30534385541304232, -7.595227055684746986, 51.75156210489594599 ) ) ;
#43684 = CARTESIAN_POINT ( 'NONE',  ( -13.24520478104276933, -9.193358983593601153, 64.19481115367814539 ) ) ;
#43685 = CARTESIAN_POINT ( 'NONE',  ( -19.24829632005326019, -7.991050106228435368, 67.04504941182814548 ) ) ;
#43686 =( BOUNDED_SURFACE ( )  B_SPLINE_SURFACE ( 3, 1, ( 
 ( #25723, #21785 ),
 ( #21324, #28695 ),
 ( #44227, #14125 ),
 ( #43732, #9985 ),
 ( #47653, #40739 ),
 ( #40030, #48134 ),
 ( #13891, #28934 ) ),
 .UNSPECIFIED., .T., .F., .F. ) 
 B_SPLINE_SURFACE_WITH_KNOTS ( ( 4, 3, 4 ),
 ( 2, 2 ),
 ( 0.000000000000000000, 0.5000000000000000000, 1.000000000000000000 ),
 ( 0.000000000000000000, 1.000000000000000000 ),
 .UNSPECIFIED. ) 
 GEOMETRIC_REPRESENTATION_ITEM ( )  RATIONAL_B_SPLINE_SURFACE ( (
 ( 1.000000000000000000, 1.000000000000000000),
 ( 0.3333333333333335369, 0.3333333333333330373),
 ( 0.3333333333333335369, 0.3333333333333330373),
 ( 1.000000000000000000, 1.000000000000000000),
 ( 0.3333333333333333703, 0.3333333333333333703),
 ( 0.3333333333333333703, 0.3333333333333333703),
 ( 1.000000000000000000, 1.000000000000000000) ) ) 
 REPRESENTATION_ITEM ( '' )  SURFACE ( )  );
#43687 = ADVANCED_FACE ( 'NONE', ( #33975 ), #13678, .T. ) ;
#43688 = CIRCLE ( 'NONE', #25561, 1.250000000000007994 ) ;
#43689 = CARTESIAN_POINT ( 'NONE',  ( -45.92409385541306932, -12.76354662275040042, 70.50000000000000000 ) ) ;
#43690 = DIRECTION ( 'NONE',  ( -1.000000000000000000, -2.866981220435670867E-17, 3.652049423109068320E-16 ) ) ;
#43691 = ORIENTED_EDGE ( 'NONE', *, *, #10858, .T. ) ;
#43692 = CARTESIAN_POINT ( 'NONE',  ( -21.05173877328207510, -20.79594606475588137, 65.86988551343767995 ) ) ;
#43693 = CARTESIAN_POINT ( 'NONE',  ( -21.02116742812006223, -20.87599269455877860, 61.99982634431184181 ) ) ;
#43694 = ORIENTED_EDGE ( 'NONE', *, *, #11522, .F. ) ;
#43695 = DIRECTION ( 'NONE',  ( -3.413470714839332458E-33, 1.190614954331866791E-16, -1.000000000000000000 ) ) ;
#43696 =( BOUNDED_CURVE ( )  B_SPLINE_CURVE ( 3, ( #34338, #8760, #26735, #19581 ),
 .UNSPECIFIED., .F., .F. ) 
 B_SPLINE_CURVE_WITH_KNOTS ( ( 4, 4 ),
 ( 0.9074455897393663983, 1.000000000000000000 ),
 .UNSPECIFIED. ) 
 CURVE ( )  GEOMETRIC_REPRESENTATION_ITEM ( )  RATIONAL_B_SPLINE_CURVE ( ( 0.6983129098261007250, 0.7760317562607048636, 0.8765941196520046219, 1.000000000000000000 ) ) 
 REPRESENTATION_ITEM ( '' )  );
#43697 = CARTESIAN_POINT ( 'NONE',  ( -18.54053647975129238, -21.77400351277580270, 68.81514511891278119 ) ) ;
#43698 = VERTEX_POINT ( 'NONE', #27573 ) ;
#43699 = CARTESIAN_POINT ( 'NONE',  ( -18.98390459359973548, -7.933620001262258192, 66.91543923465640376 ) ) ;
#43700 = LINE ( 'NONE', #16600, #25763 ) ;
#43701 = ORIENTED_EDGE ( 'NONE', *, *, #4051, .F. ) ;
#43702 = CARTESIAN_POINT ( 'NONE',  ( 18.57590614458706924, 0.6667653706756797582, 50.27657325150221368 ) ) ;
#43703 = EDGE_CURVE ( 'NONE', #956, #4771, #18338, .T. ) ;
#43704 = CARTESIAN_POINT ( 'NONE',  ( -23.33759372854072822, -18.55733037075456693, 72.83538601489385655 ) ) ;
#43705 = CYLINDRICAL_SURFACE ( 'NONE', #1452, 0.1500000000000056566 ) ;
#43706 = CARTESIAN_POINT ( 'NONE',  ( -10.77407439928238908, -17.16094721493464093, 57.89580409822232099 ) ) ;
#43707 = ORIENTED_EDGE ( 'NONE', *, *, #31645, .F. ) ;
#43708 = CARTESIAN_POINT ( 'NONE',  ( -22.38400238879419391, -20.36826089713532895, 62.41934470639706944 ) ) ;
#43709 = CARTESIAN_POINT ( 'NONE',  ( -24.53780083649505173, -12.59584922708229904, 69.95738295622972203 ) ) ;
#43710 = ADVANCED_FACE ( 'NONE', ( #31753 ), #1215, .T. ) ;
#43711 = DIRECTION ( 'NONE',  ( -3.071710424422018668E-17, 6.404604876783312462E-16, 1.000000000000000000 ) ) ;
#43712 = DIRECTION ( 'NONE',  ( -1.770046493635803029E-07, 8.183081527205841035E-08, 0.9999999999999809042 ) ) ;
#43713 = B_SPLINE_CURVE_WITH_KNOTS ( 'NONE', 3,
 ( #30915, #35311, #12424, #5047, #27444, #28181, #12186, #42477, #24252, #43205 ),
 .UNSPECIFIED., .F., .F.,
 ( 4, 2, 2, 2, 4 ),
 ( 0.000000000000000000, 0.2500000000000000000, 0.5000000000000000000, 0.7500000000000000000, 1.000000000000000000 ),
 .UNSPECIFIED. ) ;
#43714 = CARTESIAN_POINT ( 'NONE',  ( -11.42622084110231029, -18.51434063454204093, 61.27710833181471628 ) ) ;
#43715 = CARTESIAN_POINT ( 'NONE',  ( -23.04635137988585214, -19.07596084359022726, 65.96822594231640835 ) ) ;
#43716 = ORIENTED_EDGE ( 'NONE', *, *, #18703, .F. ) ;
#43717 = CARTESIAN_POINT ( 'NONE',  ( -24.34788207851723740, -17.55975901192373811, 66.12074161205516987 ) ) ;
#43718 = ADVANCED_FACE ( 'NONE', ( #15745 ), #31510, .F. ) ;
#43719 = CARTESIAN_POINT ( 'NONE',  ( -20.15980875465224997, -21.73879204183439029, 72.59752904776686933 ) ) ;
#43720 = CARTESIAN_POINT ( 'NONE',  ( -10.00117625416208433, -15.44487358686203571, 57.68297391752145842 ) ) ;
#43721 = B_SPLINE_CURVE_WITH_KNOTS ( 'NONE', 1,
 ( #18241, #2745 ),
 .UNSPECIFIED., .F., .F.,
 ( 2, 2 ),
 ( 0.000000000000000000, 1.000000000000000000 ),
 .UNSPECIFIED. ) ;
#43722 = EDGE_LOOP ( 'NONE', ( #43976, #26760 ) ) ;
#43723 = CARTESIAN_POINT ( 'NONE',  ( -18.02409385541303877, -9.359200813967568422, 50.49621490985803263 ) ) ;
#43724 = CIRCLE ( 'NONE', #4374, 5.249999999999998224 ) ;
#43725 = ORIENTED_EDGE ( 'NONE', *, *, #1349, .F. ) ;
#43726 = VERTEX_POINT ( 'NONE', #5413 ) ;
#43727 = VERTEX_POINT ( 'NONE', #42355 ) ;
#43728 = CARTESIAN_POINT ( 'NONE',  ( -18.76558283008973049, -7.480892646508040755, 70.55563411965815135 ) ) ;
#43729 = CARTESIAN_POINT ( 'NONE',  ( -23.19494587819374942, -18.77118419879135303, 66.12389430422854275 ) ) ;
#43730 = DIRECTION ( 'NONE',  ( 0.09855345062332551698, 0.9951317587989213509, 3.188559572831062401E-08 ) ) ;
#43731 = EDGE_CURVE ( 'NONE', #35167, #16426, #8312, .T. ) ;
#43732 = CARTESIAN_POINT ( 'NONE',  ( -13.01616685277437391, -9.306763517318227485, 70.86397465682092900 ) ) ;
#43733 = ADVANCED_FACE ( 'NONE', ( #1719 ), #20433, .T. ) ;
#43734 = ORIENTED_EDGE ( 'NONE', *, *, #31173, .F. ) ;
#43735 = ORIENTED_EDGE ( 'NONE', *, *, #44535, .T. ) ;
#43736 = CARTESIAN_POINT ( 'NONE',  ( -19.34909385650551883, -8.104110260919579645, 48.81699501597546487 ) ) ;
#43737 = B_SPLINE_CURVE_WITH_KNOTS ( 'NONE', 3,
 ( #44361, #6677, #29822, #21934, #32995, #29327, #14505, #18226, #44133, #11103 ),
 .UNSPECIFIED., .F., .F.,
 ( 4, 2, 2, 2, 4 ),
 ( 0.000000000000000000, 0.2500000000000000000, 0.5000000000000000000, 0.7500000000000000000, 1.000000000000000000 ),
 .UNSPECIFIED. ) ;
#43738 = EDGE_CURVE ( 'NONE', #23048, #25893, #45926, .T. ) ;
#43739 = CARTESIAN_POINT ( 'NONE',  ( -24.87381043567631878, -14.88698653629387003, 59.42112968367225534 ) ) ;
#43740 = CARTESIAN_POINT ( 'NONE',  ( -23.70015231925135168, -18.82353928378165975, 69.47867257277708575 ) ) ;
#43741 = CARTESIAN_POINT ( 'NONE',  ( -19.91159385650551528, -6.922745924619793101, 51.69366785382590024 ) ) ;
#43742 = VERTEX_POINT ( 'NONE', #27085 ) ;
#43743 = CARTESIAN_POINT ( 'NONE',  ( -23.85748962928175132, -11.92509172808648543, 59.49707787073156595 ) ) ;
#43744 = DIRECTION ( 'NONE',  ( 3.549360974554993999E-17, -6.371834667797928663E-18, -1.000000000000000000 ) ) ;
#43745 = ORIENTED_EDGE ( 'NONE', *, *, #20153, .T. ) ;
#43746 = LINE ( 'NONE', #47668, #12318 ) ;
#43747 = VECTOR ( 'NONE', #17923, 1000.000000000000227 ) ;
#43748 = AXIS2_PLACEMENT_3D ( 'NONE', #24489, #39247, #9940 ) ;
#43749 = ORIENTED_EDGE ( 'NONE', *, *, #33091, .F. ) ;
#43750 = FACE_OUTER_BOUND ( 'NONE', #20544, .T. ) ;
#43751 = DIRECTION ( 'NONE',  ( -5.731567514496413899E-31, -1.020425574103664789E-16, -1.000000000000000000 ) ) ;
#43752 = CARTESIAN_POINT ( 'NONE',  ( -18.97054410961560578, -7.521390078327941708, 67.08567059339527816 ) ) ;
#43753 = VERTEX_POINT ( 'NONE', #34715 ) ;
#43754 = DIRECTION ( 'NONE',  ( 6.312331213287273068E-07, 6.220915576652692866E-06, 0.9999999999804508599 ) ) ;
#43755 = DIRECTION ( 'NONE',  ( 0.9687793358424821033, -0.2479245821708679909, 0.000000000000000000 ) ) ;
#43756 = CARTESIAN_POINT ( 'NONE',  ( -19.23866564181064831, -21.62168251543363695, 58.82507384655652771 ) ) ;
#43757 = VERTEX_POINT ( 'NONE', #42610 ) ;
#43758 = DIRECTION ( 'NONE',  ( 3.071710424422018668E-17, -6.404604876783312462E-16, -1.000000000000000000 ) ) ;
#43759 = B_SPLINE_CURVE_WITH_KNOTS ( 'NONE', 1,
 ( #2176, #6117 ),
 .UNSPECIFIED., .F., .F.,
 ( 2, 2 ),
 ( 0.000000000000000000, 1.000000000000000000 ),
 .UNSPECIFIED. ) ;
#43760 = CARTESIAN_POINT ( 'NONE',  ( -24.85346453946240786, -14.25412306239375049, 69.90921191474365060 ) ) ;
#43761 = EDGE_LOOP ( 'NONE', ( #16625, #21358 ) ) ;
#43762 = CARTESIAN_POINT ( 'NONE',  ( -13.26809664353323726, -20.51382390604332784, 61.66079502706314486 ) ) ;
#43763 = CARTESIAN_POINT ( 'NONE',  ( -9.974215871585233373, -14.86485004610319827, 74.91283608227215041 ) ) ;
#43765 = EDGE_CURVE ( 'NONE', #35674, #38958, #15986, .T. ) ;
#43764 = ORIENTED_EDGE ( 'NONE', *, *, #43863, .T. ) ;
#43766 = CARTESIAN_POINT ( 'NONE',  ( -22.51726263819124441, -19.68384825699994423, 72.79400547081151274 ) ) ;
#43767 = FACE_OUTER_BOUND ( 'NONE', #6105, .T. ) ;
#43768 = CARTESIAN_POINT ( 'NONE',  ( -13.26948432366006969, -9.109728530933422164, 60.32461385657482822 ) ) ;
#43769 = CARTESIAN_POINT ( 'NONE',  ( -13.47245400663725690, -21.12492667118925382, 65.10133491818508844 ) ) ;
#43770 = ORIENTED_EDGE ( 'NONE', *, *, #24938, .F. ) ;
#43771 = CARTESIAN_POINT ( 'NONE',  ( -18.11889279746774051, -21.82488571228486052, 65.49532159284275679 ) ) ;
#43772 = CARTESIAN_POINT ( 'NONE',  ( -19.03203220252169459, -7.534746275656669212, 67.09410107843321214 ) ) ;
#43773 = DIRECTION ( 'NONE',  ( 0.6607190350373965959, 0.7506333037770516192, 0.000000000000000000 ) ) ;
#43774 = VERTEX_POINT ( 'NONE', #38650 ) ;
#43775 = CARTESIAN_POINT ( 'NONE',  ( -9.979672921070292801, -14.51892525773737574, 67.90154210966345261 ) ) ;
#43776 = CARTESIAN_POINT ( 'NONE',  ( -24.77850173595669503, -15.99961219664241696, 66.24041782031707726 ) ) ;
#43777 = ORIENTED_EDGE ( 'NONE', *, *, #38491, .F. ) ;
#43778 = VERTEX_POINT ( 'NONE', #15983 ) ;
#43779 = CARTESIAN_POINT ( 'NONE',  ( -14.81801217541857518, -21.30606701939088765, 58.45152577640163116 ) ) ;
#43780 = CARTESIAN_POINT ( 'NONE',  ( -15.56648003470729336, -8.060123005460294365, 70.83663087793784996 ) ) ;
#43781 = CARTESIAN_POINT ( 'NONE',  ( -10.03035368457962662, -15.72374687363213575, 61.22284448286259817 ) ) ;
#43782 = CARTESIAN_POINT ( 'NONE',  ( -10.59051903643958958, -13.04363995460383663, 74.82250634059326444 ) ) ;
#43783 = CARTESIAN_POINT ( 'NONE',  ( -19.45112228907181873, -7.640138419055735319, 60.08376115775335791 ) ) ;
#43784 = CARTESIAN_POINT ( 'NONE',  ( -21.18398602608336745, -21.24092397535611809, 65.69958545398036165 ) ) ;
#43785 = CARTESIAN_POINT ( 'NONE',  ( -12.40538917401127961, -20.31523793222865493, 68.52152763170285255 ) ) ;
#43786 = CARTESIAN_POINT ( 'NONE',  ( -20.50783594841701785, -8.027295835816985914, 66.96599399791791996 ) ) ;
#43787 = ADVANCED_FACE ( 'NONE', ( #31029 ), #46046, .T. ) ;
#43788 = AXIS2_PLACEMENT_3D ( 'NONE', #19182, #15713, #45792 ) ;
#43789 = VECTOR ( 'NONE', #31015, 1000.000000000000000 ) ;
#43790 = VERTEX_POINT ( 'NONE', #17917 ) ;
#43791 = ORIENTED_EDGE ( 'NONE', *, *, #6136, .T. ) ;
#43792 = CARTESIAN_POINT ( 'NONE',  ( -24.83263366448169762, -15.59490076022755112, 73.18799035805197661 ) ) ;
#43793 = EDGE_CURVE ( 'NONE', #26823, #24042, #21804, .T. ) ;
#43794 = EDGE_CURVE ( 'NONE', #19879, #29515, #43571, .T. ) ;
#43795 = CARTESIAN_POINT ( 'NONE',  ( -19.86472783040103707, -8.248401445373296781, 73.94770042502594265 ) ) ;
#43796 = DIRECTION ( 'NONE',  ( 0.000000000000000000, 0.000000000000000000, 1.000000000000000000 ) ) ;
#43797 = FACE_OUTER_BOUND ( 'NONE', #38458, .T. ) ;
#43798 = VECTOR ( 'NONE', #2368, 1000.000000000000000 ) ;
#43799 = CARTESIAN_POINT ( 'NONE',  ( -4.924093855413050669, -6.359206544744109735, 52.99999999999998579 ) ) ;
#43800 = B_SPLINE_CURVE_WITH_KNOTS ( 'NONE', 1,
 ( #24686, #25399 ),
 .UNSPECIFIED., .F., .F.,
 ( 2, 2 ),
 ( 0.000000000000000000, 1.000000000000000000 ),
 .UNSPECIFIED. ) ;
#43801 = CARTESIAN_POINT ( 'NONE',  ( -19.31784385650551528, -9.790100578890868377, 49.79778022625163203 ) ) ;
#43802 = ORIENTED_EDGE ( 'NONE', *, *, #11617, .T. ) ;
#43803 = B_SPLINE_CURVE_WITH_KNOTS ( 'NONE', 1,
 ( #34196, #33962 ),
 .UNSPECIFIED., .F., .F.,
 ( 2, 2 ),
 ( 0.000000000000000000, 1.000000000000000000 ),
 .UNSPECIFIED. ) ;
#43804 = CARTESIAN_POINT ( 'NONE',  ( -15.22312280068192081, -21.51522583983519255, 61.79167741754957177 ) ) ;
#43805 = CARTESIAN_POINT ( 'NONE',  ( -19.96591064584176323, -21.38508948087614669, 72.40478736589766129 ) ) ;
#43806 = DIRECTION ( 'NONE',  ( 0.9687793358424821033, -0.2479245821708677133, 0.000000000000000000 ) ) ;
#43807 = CARTESIAN_POINT ( 'NONE',  ( -10.42257993575900876, -15.70014684107950842, 68.12200980565171449 ) ) ;
#43808 = VERTEX_POINT ( 'NONE', #2671 ) ;
#43809 = CARTESIAN_POINT ( 'NONE',  ( -10.59785598015707819, -16.35919899344940021, 71.55636283569445766 ) ) ;
#43810 = CARTESIAN_POINT ( 'NONE',  ( -24.72409385541305582, -15.80920654474410725, 65.99999999999998579 ) ) ;
#43811 = ADVANCED_FACE ( 'NONE', ( #28780 ), #17679, .T. ) ;
#43812 = FACE_OUTER_BOUND ( 'NONE', #21223, .T. ) ;
#43813 =( BOUNDED_CURVE ( )  B_SPLINE_CURVE ( 3, ( #7755, #4059, #19058, #7004 ),
 .UNSPECIFIED., .F., .F. ) 
 B_SPLINE_CURVE_WITH_KNOTS ( ( 4, 4 ),
 ( 0.000000000000000000, 0.4074455897393629566 ),
 .UNSPECIFIED. ) 
 CURVE ( )  GEOMETRIC_REPRESENTATION_ITEM ( )  RATIONAL_B_SPLINE_CURVE ( ( 1.000000000000000000, 0.4567392136813327452, 0.3561768502900305999, 0.6983129098260936196 ) ) 
 REPRESENTATION_ITEM ( '' )  );
#43814 = B_SPLINE_CURVE_WITH_KNOTS ( 'NONE', 3,
 ( #43720, #40015, #17097, #21310, #24763, #24530, #36302, #2585, #32619, #13880 ),
 .UNSPECIFIED., .F., .F.,
 ( 4, 2, 2, 2, 4 ),
 ( 0.1272669073658393990, 0.2522669073463166267, 0.3772669073267939099, 0.5022669073072711932, 0.6272669072877483654 ),
 .UNSPECIFIED. ) ;
#43815 = B_SPLINE_CURVE_WITH_KNOTS ( 'NONE', 3,
 ( #10178, #5518, #12886, #1566, #13114, #46640, #24480, #24719, #5986, #5271 ),
 .UNSPECIFIED., .F., .F.,
 ( 4, 2, 2, 2, 4 ),
 ( 0.000000000000000000, 0.2500000000000000000, 0.5000000000000000000, 0.7500000000000000000, 1.000000000000000000 ),
 .UNSPECIFIED. ) ;
#43816 = CARTESIAN_POINT ( 'NONE',  ( -19.92409385541305866, -14.80920654474411080, 82.49999999999998579 ) ) ;
#43817 = ORIENTED_EDGE ( 'NONE', *, *, #22792, .T. ) ;
#43818 = CARTESIAN_POINT ( 'NONE',  ( -23.04658630743911374, -18.97915095201261337, 59.11083934693237296 ) ) ;
#43819 = AXIS2_PLACEMENT_3D ( 'NONE', #34252, #30593, #15783 ) ;
#43820 = VECTOR ( 'NONE', #35663, 1000.000000000000000 ) ;
#43821 = ORIENTED_EDGE ( 'NONE', *, *, #15261, .T. ) ;
#43822 = DIRECTION ( 'NONE',  ( 0.8603395911234834603, 0.5097212845717520313, 0.000000000000000000 ) ) ;
#43823 = CARTESIAN_POINT ( 'NONE',  ( -10.23610968374255314, -12.85046669463587143, 67.85336945107273721 ) ) ;
#43824 = B_SPLINE_CURVE_WITH_KNOTS ( 'NONE', 3,
 ( #21357, #5617, #32431, #47452, #20627, #35622, #26198, #104, #11179, #3531 ),
 .UNSPECIFIED., .F., .F.,
 ( 4, 2, 2, 2, 4 ),
 ( 0.1272669073658526662, 0.2522669073488176261, 0.3772669073317826416, 0.5022669073147476571, 0.6272669072977126170 ),
 .UNSPECIFIED. ) ;
#43825 = ORIENTED_EDGE ( 'NONE', *, *, #5122, .T. ) ;
#43826 = EDGE_CURVE ( 'NONE', #6783, #22563, #20260, .T. ) ;
#43827 = CARTESIAN_POINT ( 'NONE',  ( -4.424093855413049781, -6.859206544744110623, 52.99999999999998579 ) ) ;
#43828 = CARTESIAN_POINT ( 'NONE',  ( -14.34284385650551741, -8.811426318492348031, 52.18089403414752070 ) ) ;
#43829 = EDGE_CURVE ( 'NONE', #15022, #47208, #13734, .T. ) ;
#43830 = ORIENTED_EDGE ( 'NONE', *, *, #25635, .T. ) ;
#43831 = FACE_OUTER_BOUND ( 'NONE', #42134, .T. ) ;
#43832 = CARTESIAN_POINT ( 'NONE',  ( -15.95707209241614422, -7.504986913482371236, 63.85506412386598640 ) ) ;
#43833 =( BOUNDED_CURVE ( )  B_SPLINE_CURVE ( 3, ( #46789, #27585, #13517, #47021 ),
 .UNSPECIFIED., .F., .F. ) 
 B_SPLINE_CURVE_WITH_KNOTS ( ( 4, 4 ),
 ( 0.5000000000000000000, 0.9074455897393661763 ),
 .UNSPECIFIED. ) 
 CURVE ( )  GEOMETRIC_REPRESENTATION_ITEM ( )  RATIONAL_B_SPLINE_CURVE ( ( 1.000000000000021982, 0.4567392136813435144, 0.3561768502900192201, 0.6983129098260727474 ) ) 
 REPRESENTATION_ITEM ( '' )  );
#43834 = CARTESIAN_POINT ( 'NONE',  ( -23.52949419687348964, -11.28347464189849703, 70.17738639980606763 ) ) ;
#43835 = ORIENTED_EDGE ( 'NONE', *, *, #36722, .F. ) ;
#43837 = FACE_OUTER_BOUND ( 'NONE', #32597, .T. ) ;
#43836 =( BOUNDED_CURVE ( )  B_SPLINE_CURVE ( 3, ( #21147, #16703, #24360, #9099 ),
 .UNSPECIFIED., .F., .F. ) 
 B_SPLINE_CURVE_WITH_KNOTS ( ( 4, 4 ),
 ( 0.4074455897393593484, 0.5000000000000000000 ),
 .UNSPECIFIED. ) 
 CURVE ( )  GEOMETRIC_REPRESENTATION_ITEM ( )  RATIONAL_B_SPLINE_CURVE ( ( 0.6983129098260878465, 0.7760317562606910968, 0.8765941196519944079, 0.9999999999999958922 ) ) 
 REPRESENTATION_ITEM ( '' )  );
#43838 = DIRECTION ( 'NONE',  ( -1.000000000000000000, -2.866981220435666553E-17, 0.000000000000000000 ) ) ;
#43839 = CARTESIAN_POINT ( 'NONE',  ( -10.66703313327717417, -12.79807994555918960, 64.56836111017611302 ) ) ;
#43840 = LINE ( 'NONE', #17469, #24805 ) ;
#43841 = ORIENTED_EDGE ( 'NONE', *, *, #30300, .T. ) ;
#43842 = ORIENTED_EDGE ( 'NONE', *, *, #36329, .T. ) ;
#43843 = DIRECTION ( 'NONE',  ( -3.071710424422018668E-17, 6.404604876783312462E-16, 1.000000000000000000 ) ) ;
#43844 = DIRECTION ( 'NONE',  ( 0.8651630202045380580, -0.5014907262059380422, -5.433021001198017416E-08 ) ) ;
#43845 = ORIENTED_EDGE ( 'NONE', *, *, #15982, .T. ) ;
#43846 = FACE_OUTER_BOUND ( 'NONE', #35522, .T. ) ;
#43847 = CARTESIAN_POINT ( 'NONE',  ( -19.18034385759799321, -9.360768649639302552, 51.01397948905922419 ) ) ;
#43848 = FACE_OUTER_BOUND ( 'NONE', #30245, .T. ) ;
#43849 = DIRECTION ( 'NONE',  ( -1.669677910507523245E-21, 1.000000000000000000, -1.084253996632606407E-42 ) ) ;
#43850 = CARTESIAN_POINT ( 'NONE',  ( -12.31380156693488992, -10.02538874655004442, 60.85918086676540639 ) ) ;
#43851 =( BOUNDED_CURVE ( )  B_SPLINE_CURVE ( 3, ( #47673, #9777, #1649, #13911 ),
 .UNSPECIFIED., .F., .F. ) 
 B_SPLINE_CURVE_WITH_KNOTS ( ( 4, 4 ),
 ( 0.4074455897393667869, 0.5000000000000000000 ),
 .UNSPECIFIED. ) 
 CURVE ( )  GEOMETRIC_REPRESENTATION_ITEM ( )  RATIONAL_B_SPLINE_CURVE ( ( 0.6983129098261057210, 0.7760317562607094155, 0.8765941196520075085, 1.000000000000000222 ) ) 
 REPRESENTATION_ITEM ( '' )  );
#43852 = ORIENTED_EDGE ( 'NONE', *, *, #7915, .F. ) ;
#43853 = CARTESIAN_POINT ( 'NONE',  ( -20.90753508896134960, -8.676468725517494818, 60.25614029449676678 ) ) ;
#43854 = EDGE_CURVE ( 'NONE', #25404, #7167, #41483, .T. ) ;
#43855 = EDGE_CURVE ( 'NONE', #7670, #17028, #17449, .T. ) ;
#43856 =( LENGTH_UNIT ( ) NAMED_UNIT ( * ) SI_UNIT ( .MILLI., .METRE. ) );
#43857 = DIRECTION ( 'NONE',  ( 1.000000000000000000, -0.000000000000000000, -8.260587980841940012E-17 ) ) ;
#43858 = CARTESIAN_POINT ( 'NONE',  ( -16.58248652804564927, -22.21164012696474899, 65.34751608897319386 ) ) ;
#43859 = STYLED_ITEM ( 'NONE', ( #33779 ), #14655 ) ;
#43860 = ORIENTED_EDGE ( 'NONE', *, *, #22282, .F. ) ;
#43861 = AXIS2_PLACEMENT_3D ( 'NONE', #22182, #10844, #11832 ) ;
#43862 = EDGE_CURVE ( 'NONE', #47879, #13276, #13252, .T. ) ;
#43863 = EDGE_CURVE ( 'NONE', #39854, #3501, #26860, .T. ) ;
#43864 = ORIENTED_EDGE ( 'NONE', *, *, #17843, .F. ) ;
#43865 = CARTESIAN_POINT ( 'NONE',  ( -17.38762135442090795, -7.756298984960698917, 63.43568405917763897 ) ) ;
#43866 = ADVANCED_FACE ( 'NONE', ( #43812 ), #16947, .T. ) ;
#43867 = CARTESIAN_POINT ( 'NONE',  ( -15.49415903819706486, -8.028509590827587417, 74.22985659018391402 ) ) ;
#43868 = VECTOR ( 'NONE', #10208, 1000.000000000000000 ) ;
#43869 = ADVANCED_FACE ( 'NONE', ( #21405 ), #40113, .T. ) ;
#43870 = ORIENTED_EDGE ( 'NONE', *, *, #37472, .T. ) ;
#43871 = CIRCLE ( 'NONE', #21082, 5.249999999999998224 ) ;
#43872 = CARTESIAN_POINT ( 'NONE',  ( -23.96075645138428456, -17.45014240273063066, 65.94357239682317129 ) ) ;
#43873 = DIRECTION ( 'NONE',  ( 0.7800143876985550229, -0.6257615799833393666, 5.505484597913564244E-08 ) ) ;
#43874 = EDGE_CURVE ( 'NONE', #34219, #18401, #23611, .T. ) ;
#43875 = ORIENTED_EDGE ( 'NONE', *, *, #12071, .T. ) ;
#43876 = CARTESIAN_POINT ( 'NONE',  ( -20.88270815654435353, -21.40782497263450068, 58.82970582236164603 ) ) ;
#43877 = CARTESIAN_POINT ( 'NONE',  ( -24.47368665962210343, -14.70950332193510413, 62.72768537250228604 ) ) ;
#43878 = CARTESIAN_POINT ( 'NONE',  ( -23.34190511704397153, -19.33504077159632573, 58.92764702605110472 ) ) ;
#43879 = ORIENTED_EDGE ( 'NONE', *, *, #25362, .T. ) ;
#43880 = CARTESIAN_POINT ( 'NONE',  ( -20.00946575929301474, -8.250368826910309039, 74.02096600124984604 ) ) ;
#43881 = ORIENTED_EDGE ( 'NONE', *, *, #40676, .T. ) ;
#43882 = DIRECTION ( 'NONE',  ( 1.000000000000000000, 0.000000000000000000, -5.466375705775733989E-17 ) ) ;
#43883 = CARTESIAN_POINT ( 'NONE',  ( -13.08950423898529891, -12.99622877252704001, 52.02966884056656482 ) ) ;
#43884 = ORIENTED_EDGE ( 'NONE', *, *, #5321, .F. ) ;
#43885 = CARTESIAN_POINT ( 'NONE',  ( -17.42409385541299471, -14.80920654474435771, 49.52966884056655772 ) ) ;
#43886 = CARTESIAN_POINT ( 'NONE',  ( -13.71339271347209454, -20.80363700974684349, 65.28628881287176000 ) ) ;
#43887 = APPLICATION_CONTEXT ( 'automotive_design' ) ;
#43888 = DIRECTION ( 'NONE',  ( -5.731567514496413899E-31, -1.020425574103664789E-16, -1.000000000000000000 ) ) ;
#43889 = CARTESIAN_POINT ( 'NONE',  ( -17.81160558974998764, -14.71003671187600936, 52.02966884056656482 ) ) ;
#43890 = CARTESIAN_POINT ( 'NONE',  ( -17.77921064978749044, -22.25082400685520057, 58.59048811498988840 ) ) ;
#43891 = DIRECTION ( 'NONE',  ( 0.000000000000000000, 1.000000000000000000, -0.000000000000000000 ) ) ;
#43892 = ORIENTED_EDGE ( 'NONE', *, *, #19931, .T. ) ;
#43893 = CARTESIAN_POINT ( 'NONE',  ( -10.20197030601470090, -12.78660143320473175, 53.49999999999994316 ) ) ;
#43894 = AXIS2_PLACEMENT_3D ( 'NONE', #17397, #31939, #47683 ) ;
#43895 = AXIS2_PLACEMENT_3D ( 'NONE', #16483, #31519, #999 ) ;
#43896 = CARTESIAN_POINT ( 'NONE',  ( -22.94085434386056832, -9.802298134861713308, 70.19673941016031904 ) ) ;
#43897 = DIRECTION ( 'NONE',  ( -3.071710424422018668E-17, 6.404604876783312462E-16, 1.000000000000000000 ) ) ;
#43898 = PLANE ( 'NONE',  #4659 ) ;
#43899 = CARTESIAN_POINT ( 'NONE',  ( -13.63659385650551847, -6.915538690918075382, 49.31353937987644542 ) ) ;
#43900 = ORIENTED_EDGE ( 'NONE', *, *, #6496, .F. ) ;
#43901 = EDGE_LOOP ( 'NONE', ( #33287, #16788, #43259, #10800 ) ) ;
#43902 = CARTESIAN_POINT ( 'NONE',  ( -10.39215589072981416, -14.30487699944780289, 64.68803863382906627 ) ) ;
#43903 = CARTESIAN_POINT ( 'NONE',  ( -24.83263366448169762, -15.59490076022755112, 73.18799035805197661 ) ) ;
#43904 = ORIENTED_EDGE ( 'NONE', *, *, #12413, .T. ) ;
#43905 = CARTESIAN_POINT ( 'NONE',  ( -10.38025826595154477, -14.36272272558099772, 71.47215414551031643 ) ) ;
#43907 = CARTESIAN_POINT ( 'NONE',  ( -11.77456283875730136, -18.94252740843654337, 71.68685932468078192 ) ) ;
#43906 = CARTESIAN_POINT ( 'NONE',  ( -10.14660727810982976, -16.40665786317032371, 71.56094979796495181 ) ) ;
#43908 = CARTESIAN_POINT ( 'NONE',  ( -17.90690210039477392, -22.24367211215778539, 61.99819018155271522 ) ) ;
#43909 = CARTESIAN_POINT ( 'NONE',  ( -19.30746897944592888, -7.600422969554355923, 60.07437648108736994 ) ) ;
#43910 = CARTESIAN_POINT ( 'NONE',  ( -14.66790711817407278, -21.29843871104708342, 58.18089935161520287 ) ) ;
#43911 = EDGE_CURVE ( 'NONE', #1220, #42912, #24984, .T. ) ;
#43912 = CARTESIAN_POINT ( 'NONE',  ( -15.53265176333180619, -21.60105060138385369, 72.33103357390284316 ) ) ;
#43913 = FACE_OUTER_BOUND ( 'NONE', #24939, .T. ) ;
#43914 = AXIS2_PLACEMENT_3D ( 'NONE', #13668, #25269, #2838 ) ;
#43915 = CARTESIAN_POINT ( 'NONE',  ( -12.15399301493812878, -9.543295845094297292, 57.20440096431307353 ) ) ;
#43916 = PLANE ( 'NONE',  #46036 ) ;
#43917 = CARTESIAN_POINT ( 'NONE',  ( -20.75775239920833215, -8.146595409969087598, 63.56767435313065562 ) ) ;
#43918 = EDGE_CURVE ( 'NONE', #47684, #5480, #20109, .T. ) ;
#43919 = ORIENTED_EDGE ( 'NONE', *, *, #34986, .T. ) ;
#43920 = FACE_OUTER_BOUND ( 'NONE', #46323, .T. ) ;
#43921 = CARTESIAN_POINT ( 'NONE',  ( -11.54914866798053197, -18.61512550936221544, 61.46813926877504031 ) ) ;
#43922 = CARTESIAN_POINT ( 'NONE',  ( -24.39703051400040223, -17.43244739030124890, 69.60678083904183211 ) ) ;
#43923 = DIRECTION ( 'NONE',  ( 1.000000000000000000, 2.866981220435666553E-17, 0.000000000000000000 ) ) ;
#43924 = DIRECTION ( 'NONE',  ( -5.731567514496413899E-31, -1.020425574103664789E-16, -1.000000000000000000 ) ) ;
#43925 = DIRECTION ( 'NONE',  ( -5.731567514496413899E-31, -1.020425574103664789E-16, -1.000000000000000000 ) ) ;
#43926 = ORIENTED_EDGE ( 'NONE', *, *, #16103, .T. ) ;
#43927 = ORIENTED_EDGE ( 'NONE', *, *, #24330, .F. ) ;
#43928 = CARTESIAN_POINT ( 'NONE',  ( -17.12409385541304374, -9.359200813967568422, 50.49621490985803263 ) ) ;
#43929 = B_SPLINE_CURVE_WITH_KNOTS ( 'NONE', 1,
 ( #45929, #31875 ),
 .UNSPECIFIED., .F., .F.,
 ( 2, 2 ),
 ( 0.000000000000000000, 1.000000000000000000 ),
 .UNSPECIFIED. ) ;
#43930 = CARTESIAN_POINT ( 'NONE',  ( -21.18000576974785787, -20.77541348745421246, 69.35450184739246993 ) ) ;
#43931 = EDGE_CURVE ( 'NONE', #7278, #39540, #14737, .T. ) ;
#43932 = VECTOR ( 'NONE', #6020, 1000.000000000000000 ) ;
#43933 = FACE_OUTER_BOUND ( 'NONE', #15220, .T. ) ;
#43934 =( BOUNDED_SURFACE ( )  B_SPLINE_SURFACE ( 3, 1, ( 
 ( #32291, #39907 ),
 ( #17488, #47061 ),
 ( #24174, #40156 ),
 ( #20225, #21200 ),
 ( #13779, #47546 ),
 ( #35237, #28099 ),
 ( #1512, #39177 ) ),
 .UNSPECIFIED., .T., .F., .F. ) 
 B_SPLINE_SURFACE_WITH_KNOTS ( ( 4, 3, 4 ),
 ( 2, 2 ),
 ( 0.000000000000000000, 0.5000000000000000000, 1.000000000000000000 ),
 ( 0.000000000000000000, 1.000000000000000000 ),
 .UNSPECIFIED. ) 
 GEOMETRIC_REPRESENTATION_ITEM ( )  RATIONAL_B_SPLINE_SURFACE ( (
 ( 1.000000000000000000, 1.000000000000000000),
 ( 0.3333333333333335369, 0.3333333333333330373),
 ( 0.3333333333333335369, 0.3333333333333330373),
 ( 1.000000000000000000, 1.000000000000000000),
 ( 0.3333333333333333703, 0.3333333333333333703),
 ( 0.3333333333333333703, 0.3333333333333333703),
 ( 1.000000000000000000, 1.000000000000000000) ) ) 
 REPRESENTATION_ITEM ( '' )  SURFACE ( )  );
#43935 = EDGE_CURVE ( 'NONE', #33529, #45391, #7603, .T. ) ;
#43936 = VECTOR ( 'NONE', #36530, 1000.000000000000000 ) ;
#43937 = CARTESIAN_POINT ( 'NONE',  ( -15.35760563471625595, -7.651489246766129071, 74.27259798395405710 ) ) ;
#43938 = FACE_OUTER_BOUND ( 'NONE', #21267, .T. ) ;
#43939 = EDGE_LOOP ( 'NONE', ( #4231, #16452, #22054, #4807 ) ) ;
#43941 = CARTESIAN_POINT ( 'NONE',  ( -19.36879887743637241, -22.00096660050156672, 58.71781517422923002 ) ) ;
#43940 = B_SPLINE_CURVE_WITH_KNOTS ( 'NONE', 1,
 ( #24288, #16867 ),
 .UNSPECIFIED., .F., .F.,
 ( 2, 2 ),
 ( 0.000000000000000000, 1.000000000000000000 ),
 .UNSPECIFIED. ) ;
#43942 = AXIS2_PLACEMENT_3D ( 'NONE', #26294, #451, #23101 ) ;
#43943 = EDGE_CURVE ( 'NONE', #24396, #12959, #41568, .T. ) ;
#43944 = VERTEX_POINT ( 'NONE', #33661 ) ;
#43945 = CARTESIAN_POINT ( 'NONE',  ( -13.52409385541304410, -9.359200813967568422, 50.49621490985803263 ) ) ;
#43946 = CYLINDRICAL_SURFACE ( 'NONE', #40078, 0.1499999999999973577 ) ;
#43947 = ORIENTED_EDGE ( 'NONE', *, *, #35992, .F. ) ;
#43948 = LINE ( 'NONE', #28901, #17342 ) ;
#43949 = CARTESIAN_POINT ( 'NONE',  ( -12.97364571557156232, -9.395203622806569399, 49.41430056510258595 ) ) ;
#43950 = CARTESIAN_POINT ( 'NONE',  ( -9.979298953853202647, -14.52750539432568289, 67.97987381442376886 ) ) ;
#43951 = ORIENTED_EDGE ( 'NONE', *, *, #45081, .T. ) ;
#43952 = CARTESIAN_POINT ( 'NONE',  ( -10.70366717127368084, -11.59369238842668359, 71.13214950009151494 ) ) ;
#43953 = LINE ( 'NONE', #44203, #32831 ) ;
#43954 = CARTESIAN_POINT ( 'NONE',  ( -21.50966673221228120, -17.12947588552333045, 49.52966884056655772 ) ) ;
#43955 = CARTESIAN_POINT ( 'NONE',  ( -24.10584592916820057, -12.56049825913868645, 73.24225570139947195 ) ) ;
#43956 = ORIENTED_EDGE ( 'NONE', *, *, #27691, .F. ) ;
#43957 = DIRECTION ( 'NONE',  ( 1.000000000000000000, 1.669677910507523057E-21, 6.493791346278465266E-22 ) ) ;
#43958 = CARTESIAN_POINT ( 'NONE',  ( -28.42409385541305511, -25.10920654474410441, 54.99999999999996447 ) ) ;
#43959 = CARTESIAN_POINT ( 'NONE',  ( -24.90891992605694227, -15.28604896337863472, 53.49999999999994316 ) ) ;
#43960 = DIRECTION ( 'NONE',  ( 0.9687793358424819923, -0.2479245821708680464, 0.000000000000000000 ) ) ;
#43961 = CARTESIAN_POINT ( 'NONE',  ( -15.41904748403203484, -7.634001509309876532, 74.19490257054667381 ) ) ;
#43962 = CARTESIAN_POINT ( 'NONE',  ( -16.19792114999740562, -7.866354181730329742, 60.48556343814865954 ) ) ;
#43963 = CARTESIAN_POINT ( 'NONE',  ( -24.69822986944709697, -13.19963441799314197, 59.54763197719577761 ) ) ;
#43964 = ORIENTED_EDGE ( 'NONE', *, *, #9469, .T. ) ;
#43965 = CARTESIAN_POINT ( 'NONE',  ( -14.92957361138602579, -21.82925975653312278, 65.22101252026929785 ) ) ;
#43966 = AXIS2_PLACEMENT_3D ( 'NONE', #15051, #3258, #25658 ) ;
#43967 = CARTESIAN_POINT ( 'NONE',  ( -12.98382639084827694, -18.07753951239978463, 53.69233794759168887 ) ) ;
#43968 = CARTESIAN_POINT ( 'NONE',  ( -13.38109212034142992, -20.52372131538385958, 58.34650125919424823 ) ) ;
#43969 = EDGE_CURVE ( 'NONE', #43790, #10474, #15433, .T. ) ;
#43970 = EDGE_LOOP ( 'NONE', ( #10348, #13922, #43180, #7551, #5182, #35119, #20063, #31395, #7592, #31835 ) ) ;
#43971 = CARTESIAN_POINT ( 'NONE',  ( -19.81318675137362462, -21.38895278651759568, 69.23482470049566473 ) ) ;
#43972 = AXIS2_PLACEMENT_3D ( 'NONE', #16241, #39402, #8892 ) ;
#43973 = AXIS2_PLACEMENT_3D ( 'NONE', #13783, #28596, #28359 ) ;
#43974 = ORIENTED_EDGE ( 'NONE', *, *, #41984, .F. ) ;
#43975 = EDGE_LOOP ( 'NONE', ( #34857, #34544, #38987, #5780 ) ) ;
#43976 = ORIENTED_EDGE ( 'NONE', *, *, #35710, .T. ) ;
#43977 = CARTESIAN_POINT ( 'NONE',  ( -18.47956468449850931, -19.37530592812942487, 52.02966884056656482 ) ) ;
#43978 = CIRCLE ( 'NONE', #44782, 2.000000000000001332 ) ;
#43979 = CARTESIAN_POINT ( 'NONE',  ( -12.90907418246050575, -8.883084357830009381, 67.55755565527715589 ) ) ;
#43980 =( BOUNDED_CURVE ( )  B_SPLINE_CURVE ( 3, ( #16682, #31722, #13470, #28516 ),
 .UNSPECIFIED., .F., .F. ) 
 B_SPLINE_CURVE_WITH_KNOTS ( ( 4, 4 ),
 ( 0.000000000000000000, 0.4074455897393656212 ),
 .UNSPECIFIED. ) 
 CURVE ( )  GEOMETRIC_REPRESENTATION_ITEM ( )  RATIONAL_B_SPLINE_CURVE ( ( 1.000000000000000000, 0.4567392136813311909, 0.3561768502900300448, 0.6983129098260966172 ) ) 
 REPRESENTATION_ITEM ( '' )  );
#43981 = FACE_OUTER_BOUND ( 'NONE', #19056, .T. ) ;
#43982 = CARTESIAN_POINT ( 'NONE',  ( -21.99284385759798965, -8.630756214087126565, 51.74842643355248129 ) ) ;
#43983 = VERTEX_POINT ( 'NONE', #30005 ) ;
#43984 = EDGE_LOOP ( 'NONE', ( #34072, #43207, #45409, #46557, #48661 ) ) ;
#43985 = CARTESIAN_POINT ( 'NONE',  ( -17.99909385650551741, -8.114302828567740988, 52.18300498402516041 ) ) ;
#43986 = EDGE_CURVE ( 'NONE', #20830, #5461, #3644, .T. ) ;
#43987 = CARTESIAN_POINT ( 'NONE',  ( -45.92409385541306222, -14.20920654474410760, 70.50000000000000000 ) ) ;
#43988 = DIRECTION ( 'NONE',  ( -5.888300610989836252E-06, -9.662809626516592716E-06, 0.9999999999359789893 ) ) ;
#43989 = EDGE_CURVE ( 'NONE', #33222, #45841, #31887, .T. ) ;
#43990 = CARTESIAN_POINT ( 'NONE',  ( -20.53034385650551386, -9.794322478646142471, 51.19202720610083901 ) ) ;
#43991 =( BOUNDED_CURVE ( )  B_SPLINE_CURVE ( 2, ( #40763, #18098, #7537, #36559, #29444, #36805, #33114, #22544, #40517 ),
 .UNSPECIFIED., .F., .F. ) 
 B_SPLINE_CURVE_WITH_KNOTS ( ( 3, 2, 2, 2, 3 ),
 ( 0.05114234498029770343, 0.05212596529054528555, 0.05310958560079286073, 0.05409320591104042897, 0.05507682622128801109 ),
 .UNSPECIFIED. ) 
 CURVE ( )  GEOMETRIC_REPRESENTATION_ITEM ( )  RATIONAL_B_SPLINE_CURVE ( ( 0.9999999999995229372, 0.9238795325117638013, 1.000000000000000000, 0.9238795325112867385, 1.000000000000000000, 0.9238795325112867385, 1.000000000000000000, 0.9238795325105971790, 1.000000000000689671 ) ) 
 REPRESENTATION_ITEM ( '' )  );
#43992 = ORIENTED_EDGE ( 'NONE', *, *, #34835, .F. ) ;
#43993 = EDGE_CURVE ( 'NONE', #17461, #42531, #13023, .T. ) ;
#43994 = CARTESIAN_POINT ( 'NONE',  ( -15.66808075433818992, -21.64011062311675815, 71.93086697972334775 ) ) ;
#43995 = AXIS2_PLACEMENT_3D ( 'NONE', #6816, #10279, #43773 ) ;
#43996 = CARTESIAN_POINT ( 'NONE',  ( -24.87424715294626054, -14.79413390388218374, 59.40333630874831528 ) ) ;
#43997 = EDGE_CURVE ( 'NONE', #5768, #22634, #21538, .T. ) ;
#43998 = ORIENTED_EDGE ( 'NONE', *, *, #39188, .F. ) ;
#43999 = CARTESIAN_POINT ( 'NONE',  ( -11.24765613265417841, -11.51409684124195998, 67.63481256405479769 ) ) ;
#44000 = AXIS2_PLACEMENT_3D ( 'NONE', #20944, #35944, #2221 ) ;
#44001 = AXIS2_PLACEMENT_3D ( 'NONE', #32390, #36058, #47412 ) ;
#44002 = ORIENTED_EDGE ( 'NONE', *, *, #16957, .T. ) ;
#44003 = CYLINDRICAL_SURFACE ( 'NONE', #17393, 0.1500000000000066835 ) ;
#44004 = CARTESIAN_POINT ( 'NONE',  ( -16.34000564509899078, -21.72481133989910163, 58.35873513796175160 ) ) ;
#44005 = CARTESIAN_POINT ( 'NONE',  ( -9.994167848590823411, -14.26249844466068772, 64.48829615640673296 ) ) ;
#44006 = EDGE_LOOP ( 'NONE', ( #37370, #37526, #16949, #15700, #6354 ) ) ;
#44007 = AXIS2_PLACEMENT_3D ( 'NONE', #20026, #37998, #42688 ) ;
#44008 = CARTESIAN_POINT ( 'NONE',  ( -14.72778380697173617, -21.32322314059157264, 58.16617885012794886 ) ) ;
#44009 = CARTESIAN_POINT ( 'NONE',  ( -17.06784385541249094, -9.357632978292226511, 49.97845033065324571 ) ) ;
#44010 = DIRECTION ( 'NONE',  ( -3.071710424422018668E-17, 6.404604876783312462E-16, 1.000000000000000000 ) ) ;
#44011 = ORIENTED_EDGE ( 'NONE', *, *, #320, .F. ) ;
#44012 = CARTESIAN_POINT ( 'NONE',  ( -21.92320759141193776, -20.24164808600927046, 62.32619241939052301 ) ) ;
#44013 = CARTESIAN_POINT ( 'NONE',  ( -23.88415220289344276, -17.63235127459526908, 62.62360984996717406 ) ) ;
#44014 = DIRECTION ( 'NONE',  ( 0.4468359692653126602, -0.01837434545035531233, 0.8944271909999156334 ) ) ;
#44015 = ADVANCED_FACE ( 'NONE', ( #3157 ), #36871, .T. ) ;
#44016 = ORIENTED_EDGE ( 'NONE', *, *, #19779, .T. ) ;
#44017 = FACE_OUTER_BOUND ( 'NONE', #29706, .T. ) ;
#44018 = ORIENTED_EDGE ( 'NONE', *, *, #20435, .T. ) ;
#44019 = CARTESIAN_POINT ( 'NONE',  ( -19.70296738327746056, -7.644578391088470148, 53.76227901944321275 ) ) ;
#44020 = CARTESIAN_POINT ( 'NONE',  ( -13.59294679993987565, -20.73687756253419678, 68.60058253670568718 ) ) ;
#44021 = CARTESIAN_POINT ( 'NONE',  ( -13.12596155740353154, -8.723179898376328012, 60.55294873703923031 ) ) ;
#44022 = CARTESIAN_POINT ( 'NONE',  ( -14.25068859620041017, -8.513811488652077486, 70.72957628655862550 ) ) ;
#44023 = ORIENTED_EDGE ( 'NONE', *, *, #15125, .T. ) ;
#44024 = DIRECTION ( 'NONE',  ( -0.1240347345892086062, 1.145860353393066553E-16, -0.9922778767136676281 ) ) ;
#44025 = UNCERTAINTY_MEASURE_WITH_UNIT (LENGTH_MEASURE( 1.000000000000000082E-05 ), #31009, 'distance_accuracy_value', 'NONE');
#44026 = CARTESIAN_POINT ( 'NONE',  ( -14.74982318541341364, -21.33234577674026156, 58.46617888512912486 ) ) ;
#44027 = EDGE_CURVE ( 'NONE', #15877, #45956, #35039, .T. ) ;
#44028 = CARTESIAN_POINT ( 'NONE',  ( -21.54693431995308828, -8.603789849366368259, 73.76162071728887781 ) ) ;
#44029 = VERTEX_POINT ( 'NONE', #37114 ) ;
#44030 = CARTESIAN_POINT ( 'NONE',  ( -7.424093855413048892, -25.10920654474410441, 56.99999999999997868 ) ) ;
#44031 = FACE_OUTER_BOUND ( 'NONE', #3309, .T. ) ;
#44032 = VERTEX_POINT ( 'NONE', #26067 ) ;
#44033 = ORIENTED_EDGE ( 'NONE', *, *, #36793, .T. ) ;
#44034 = DIRECTION ( 'NONE',  ( -3.071710424422018668E-17, 6.404604876783312462E-16, 1.000000000000000000 ) ) ;
#44036 = CARTESIAN_POINT ( 'NONE',  ( -13.12613471901881113, -20.89454346209081947, 58.16154795605982031 ) ) ;
#44035 = CIRCLE ( 'NONE', #3123, 0.09999999999999939493 ) ;
#44037 = B_SPLINE_CURVE_WITH_KNOTS ( 'NONE', 3,
 ( #28813, #10353, #25366, #29296, #47535, #21666, #44333, #6648, #17947, #36655 ),
 .UNSPECIFIED., .F., .F.,
 ( 4, 2, 2, 2, 4 ),
 ( 0.6272669072782339761, 0.7522669073001400086, 0.8772669073220461522, 1.002266907343952296, 1.127266907365858328 ),
 .UNSPECIFIED. ) ;
#44038 = DIRECTION ( 'NONE',  ( 0.9687793358424821033, -0.2479245821708677133, 0.000000000000000000 ) ) ;
#44039 = CARTESIAN_POINT ( 'NONE',  ( -23.89200535028185612, -11.11192396016905448, 70.07706043178237110 ) ) ;
#44040 = DIRECTION ( 'NONE',  ( -5.828394480008251615E-08, 1.590814170208496341E-07, 0.9999999999999855671 ) ) ;
#44041 = CARTESIAN_POINT ( 'NONE',  ( -13.04382658994076927, -9.348978013824847721, 67.45230756976776831 ) ) ;
#44042 = EDGE_CURVE ( 'NONE', #33165, #27092, #15197, .T. ) ;
#44043 = CARTESIAN_POINT ( 'NONE',  ( -14.80768872953871629, -21.78479300179184719, 61.81317360619090095 ) ) ;
#44044 = VECTOR ( 'NONE', #23865, 1000.000000000000227 ) ;
#44045 = ORIENTED_EDGE ( 'NONE', *, *, #72, .T. ) ;
#44046 = ORIENTED_EDGE ( 'NONE', *, *, #15111, .T. ) ;
#44047 = B_SPLINE_CURVE_WITH_KNOTS ( 'NONE', 1,
 ( #32575, #10181 ),
 .UNSPECIFIED., .F., .F.,
 ( 2, 2 ),
 ( 0.000000000000000000, 1.000000000000000000 ),
 .UNSPECIFIED. ) ;
#44048 = CYLINDRICAL_SURFACE ( 'NONE', #28898, 0.1500000000000047962 ) ;
#44049 = DIRECTION ( 'NONE',  ( 0.03181436478788692013, 0.9994937949748079475, 6.982004199025367595E-09 ) ) ;
#44050 = CARTESIAN_POINT ( 'NONE',  ( -13.07710726710083193, -16.59225537930583982, 49.52966884056655772 ) ) ;
#44051 = CIRCLE ( 'NONE', #22810, 1.999999999999999556 ) ;
#44052 = CARTESIAN_POINT ( 'NONE',  ( -10.38277322391999746, -14.45650603033957005, 67.86359899216145664 ) ) ;
#44053 = DIRECTION ( 'NONE',  ( 1.000000000000000000, 0.000000000000000000, 0.000000000000000000 ) ) ;
#44054 = CARTESIAN_POINT ( 'NONE',  ( -20.72409385650551883, -6.426201560718812544, 50.50509628382439331 ) ) ;
#44055 = VERTEX_POINT ( 'NONE', #18166 ) ;
#44056 = ADVANCED_FACE ( 'NONE', ( #48451 ), #7850, .T. ) ;
#44057 = CARTESIAN_POINT ( 'NONE',  ( -22.05923734882601295, -20.05472318235705131, 62.53439162613685909 ) ) ;
#44058 = DIRECTION ( 'NONE',  ( -0.9524241471993248886, 0.0009228828802128809673, -0.3047743298226214259 ) ) ;
#44059 = CIRCLE ( 'NONE', #24394, 4.686499999999998778 ) ;
#44060 = ADVANCED_FACE ( 'NONE', ( #37864 ), #29757, .T. ) ;
#44061 = DIRECTION ( 'NONE',  ( -3.071710424422018668E-17, 6.404604876783312462E-16, 1.000000000000000000 ) ) ;
#44062 = CARTESIAN_POINT ( 'NONE',  ( -11.21783165637758550, -18.93062460193366192, 64.93202459354702683 ) ) ;
#44063 = VERTEX_POINT ( 'NONE', #30500 ) ;
#44064 = CARTESIAN_POINT ( 'NONE',  ( -13.47381639519378105, -21.12577003491056260, 65.24274829841968426 ) ) ;
#44065 = AXIS2_PLACEMENT_3D ( 'NONE', #43019, #24075, #38838 ) ;
#44066 = DIRECTION ( 'NONE',  ( 1.000000000000000000, 2.866981220435666553E-17, 0.000000000000000000 ) ) ;
#44067 = AXIS2_PLACEMENT_3D ( 'NONE', #28667, #2794, #21758 ) ;
#44068 = EDGE_CURVE ( 'NONE', #1136, #8232, #39477, .T. ) ;
#44069 = CARTESIAN_POINT ( 'NONE',  ( -21.42336380182764088, -21.09487415076890215, 69.23945570945444672 ) ) ;
#44070 = ORIENTED_EDGE ( 'NONE', *, *, #37544, .F. ) ;
#44071 = DIRECTION ( 'NONE',  ( 0.4683180279402421875, -0.8835599723313410925, 4.589753183357165266E-08 ) ) ;
#44072 = CIRCLE ( 'NONE', #36922, 5.249999999999998224 ) ;
#44073 = EDGE_CURVE ( 'NONE', #19236, #38546, #11454, .T. ) ;
#44074 = ORIENTED_EDGE ( 'NONE', *, *, #9498, .T. ) ;
#44075 = LINE ( 'NONE', #13508, #14725 ) ;
#44076 = FACE_OUTER_BOUND ( 'NONE', #10492, .T. ) ;
#44077 = ORIENTED_EDGE ( 'NONE', *, *, #29778, .F. ) ;
#44078 = EDGE_CURVE ( 'NONE', #40518, #10306, #2488, .T. ) ;
#44079 = EDGE_CURVE ( 'NONE', #10723, #36414, #1160, .T. ) ;
#44080 = CARTESIAN_POINT ( 'NONE',  ( -13.49909385650551563, -8.114302828567740988, 52.18300498402516041 ) ) ;
#44081 = ORIENTED_EDGE ( 'NONE', *, *, #24633, .F. ) ;
#44082 = DIRECTION ( 'NONE',  ( 3.071710424422018668E-17, -6.404604876783312462E-16, -1.000000000000000000 ) ) ;
#44083 = AXIS2_PLACEMENT_3D ( 'NONE', #36071, #17597, #29665 ) ;
#44084 = LINE ( 'NONE', #10335, #21993 ) ;
#44085 = DIRECTION ( 'NONE',  ( -3.071710424422018668E-17, 6.404604876783312462E-16, 1.000000000000000000 ) ) ;
#44086 = VERTEX_POINT ( 'NONE', #9053 ) ;
#44087 = CARTESIAN_POINT ( 'NONE',  ( -24.23813412381375088, -12.99935709875259526, 66.31718868320673721 ) ) ;
#44088 = CARTESIAN_POINT ( 'NONE',  ( -17.11594671439511828, -7.315539529225058679, 53.49999999999994316 ) ) ;
#44089 = CARTESIAN_POINT ( 'NONE',  ( -23.08280660609100465, -10.60377317445056811, 59.61675562601556067 ) ) ;
#44090 = ORIENTED_EDGE ( 'NONE', *, *, #29312, .F. ) ;
#44091 = ORIENTED_EDGE ( 'NONE', *, *, #34000, .F. ) ;
#44092 = LINE ( 'NONE', #6882, #35340 ) ;
#44093 = CARTESIAN_POINT ( 'NONE',  ( -11.07857854458970692, -11.73724703412850623, 71.08860870961423473 ) ) ;
#44094 = ORIENTED_EDGE ( 'NONE', *, *, #14909, .T. ) ;
#44095 = B_SPLINE_CURVE_WITH_KNOTS ( 'NONE', 1,
 ( #26844, #27798 ),
 .UNSPECIFIED., .F., .F.,
 ( 2, 2 ),
 ( 0.000000000000000000, 1.000000000000000000 ),
 .UNSPECIFIED. ) ;
#44096 = CARTESIAN_POINT ( 'NONE',  ( -19.47262290702580501, -4.225005811476141737, 54.49999999999995026 ) ) ;
#44097 = CARTESIAN_POINT ( 'NONE',  ( -14.79284385759798859, -8.630756214087126565, 51.74842643355248129 ) ) ;
#44098 = CARTESIAN_POINT ( 'NONE',  ( -24.08907123645992243, -11.48026457312919391, 63.13713595337925000 ) ) ;
#44099 = CARTESIAN_POINT ( 'NONE',  ( -13.75915741662262270, -20.84105630778929097, 72.07040738930723478 ) ) ;
#44100 = CARTESIAN_POINT ( 'NONE',  ( -20.52989715560836714, -8.037455129638530593, 66.98092865364507986 ) ) ;
#44101 = DIRECTION ( 'NONE',  ( 0.000000000000000000, -1.000000000000000000, 0.000000000000000000 ) ) ;
#44102 = ORIENTED_EDGE ( 'NONE', *, *, #2376, .T. ) ;
#44103 = CARTESIAN_POINT ( 'NONE',  ( -21.96070222398937943, -20.20571033069026257, 59.06442882800701710 ) ) ;
#44104 = EDGE_CURVE ( 'NONE', #300, #28014, #23590, .T. ) ;
#44105 = CARTESIAN_POINT ( 'NONE',  ( -13.97628689860590079, -8.204186434626230096, 70.84302338899487950 ) ) ;
#44106 = AXIS2_PLACEMENT_3D ( 'NONE', #44365, #33480, #40643 ) ;
#44107 = LINE ( 'NONE', #10825, #3590 ) ;
#44108 = CARTESIAN_POINT ( 'NONE',  ( -50.42609385541305755, -14.80920654474426534, 72.98823529411762934 ) ) ;
#44109 = AXIS2_PLACEMENT_3D ( 'NONE', #15094, #42190, #34793 ) ;
#44110 = VERTEX_POINT ( 'NONE', #5112 ) ;
#44111 = ORIENTED_EDGE ( 'NONE', *, *, #8078, .T. ) ;
#44112 = CARTESIAN_POINT ( 'NONE',  ( -16.96883228653983267, -7.373121007882340372, 74.16007052498633811 ) ) ;
#44113 = CARTESIAN_POINT ( 'NONE',  ( -23.66704192603476287, -11.64274840793925136, 63.23752948021675735 ) ) ;
#44114 = FACE_OUTER_BOUND ( 'NONE', #45671, .T. ) ;
#44115 = CARTESIAN_POINT ( 'NONE',  ( -11.66853631837921057, -18.88083403034671193, 68.51129807381201431 ) ) ;
#44116 = VECTOR ( 'NONE', #17432, 1000.000000000000227 ) ;
#44117 =( BOUNDED_CURVE ( )  B_SPLINE_CURVE ( 3, ( #37832, #15405, #33631, #19126 ),
 .UNSPECIFIED., .F., .F. ) 
 B_SPLINE_CURVE_WITH_KNOTS ( ( 4, 4 ),
 ( 4.712388980384689674, 4.921828490623996188 ),
 .UNSPECIFIED. ) 
 CURVE ( )  GEOMETRIC_REPRESENTATION_ITEM ( )  RATIONAL_B_SPLINE_CURVE ( ( 1.000000000000000000, 0.9963479302455159337, 0.9963479302455159337, 1.000000000000000000 ) ) 
 REPRESENTATION_ITEM ( '' )  );
#44118 = ORIENTED_EDGE ( 'NONE', *, *, #8514, .F. ) ;
#44119 = DIRECTION ( 'NONE',  ( -0.6973657521612036669, 0.7167154300785205656, -1.015100525525034718E-08 ) ) ;
#44120 = CARTESIAN_POINT ( 'NONE',  ( -13.68776306357628236, -20.79195502325622158, 68.54805381681681808 ) ) ;
#44121 = AXIS2_PLACEMENT_3D ( 'NONE', #3578, #41993, #41497 ) ;
#44122 = ORIENTED_EDGE ( 'NONE', *, *, #13388, .F. ) ;
#44123 = DIRECTION ( 'NONE',  ( 0.9687793358424821033, -0.2479245821708680464, 0.000000000000000000 ) ) ;
#44124 = CARTESIAN_POINT ( 'NONE',  ( -19.70639647806698136, -21.90109437720271757, 65.57990800639531415 ) ) ;
#44125 = CARTESIAN_POINT ( 'NONE',  ( -16.80787187392568782, -21.83226421674134343, 68.99560634640492651 ) ) ;
#44126 = ORIENTED_EDGE ( 'NONE', *, *, #27739, .F. ) ;
#44127 =( BOUNDED_CURVE ( )  B_SPLINE_CURVE ( 3, ( #18951, #45311, #4190, #45559 ),
 .UNSPECIFIED., .F., .F. ) 
 B_SPLINE_CURVE_WITH_KNOTS ( ( 4, 4 ),
 ( 0.4074455897393688963, 0.5000000000000000000 ),
 .UNSPECIFIED. ) 
 CURVE ( )  GEOMETRIC_REPRESENTATION_ITEM ( )  RATIONAL_B_SPLINE_CURVE ( ( 0.6983129098261010581, 0.7760317562607195185, 0.8765941196520234957, 1.000000000000022871 ) ) 
 REPRESENTATION_ITEM ( '' )  );
#44128 = CARTESIAN_POINT ( 'NONE',  ( -19.45281838860202228, -9.697037067072804106, 54.07175714974879099 ) ) ;
#44129 = VERTEX_POINT ( 'NONE', #42782 ) ;
#44130 = CARTESIAN_POINT ( 'NONE',  ( -19.33060681123161828, -8.018134805169733426, 63.52269467617171728 ) ) ;
#44131 = CARTESIAN_POINT ( 'NONE',  ( -13.54822921233619226, -20.69819393533649077, 61.51646323540209949 ) ) ;
#44133 = CARTESIAN_POINT ( 'NONE',  ( -24.39889571797764845, -14.21434815047959255, 69.95275261040420389 ) ) ;
#44132 = AXIS2_PLACEMENT_3D ( 'NONE', #3889, #3382, #14673 ) ;
#44134 = EDGE_LOOP ( 'NONE', ( #40633, #31186, #47279, #43247, #14446 ) ) ;
#44135 = CARTESIAN_POINT ( 'NONE',  ( -24.17712593706266233, -17.95560904427356519, 59.19652577575318730 ) ) ;
#44136 = EDGE_CURVE ( 'NONE', #32972, #29603, #44804, .T. ) ;
#44137 = EDGE_CURVE ( 'NONE', #11451, #39638, #27029, .T. ) ;
#44138 = CARTESIAN_POINT ( 'NONE',  ( -24.47405849404658795, -12.40054206295432770, 73.28579645182460922 ) ) ;
#44139 = LINE ( 'NONE', #28377, #25781 ) ;
#44140 = AXIS2_PLACEMENT_3D ( 'NONE', #14699, #11056, #26079 ) ;
#44141 = CARTESIAN_POINT ( 'NONE',  ( -24.86251202286899442, -14.39255128295101471, 66.22646819999783929 ) ) ;
#44142 = LINE ( 'NONE', #10394, #37875 ) ;
#44143 = PLANE ( 'NONE',  #36051 ) ;
#44144 = ORIENTED_EDGE ( 'NONE', *, *, #45880, .T. ) ;
#44145 = CARTESIAN_POINT ( 'NONE',  ( -22.79734409636068904, -10.24514240368273477, 66.54182257473807738 ) ) ;
#44146 =( BOUNDED_CURVE ( )  B_SPLINE_CURVE ( 3, ( #31817, #23955, #9667, #28373 ),
 .UNSPECIFIED., .F., .F. ) 
 B_SPLINE_CURVE_WITH_KNOTS ( ( 4, 4 ),
 ( 0.000000000000000000, 0.4074455897393651216 ),
 .UNSPECIFIED. ) 
 CURVE ( )  GEOMETRIC_REPRESENTATION_ITEM ( )  RATIONAL_B_SPLINE_CURVE ( ( 1.000000000000000000, 0.4567392136813256953, 0.3561768502900279909, 0.6983129098261068313 ) ) 
 REPRESENTATION_ITEM ( '' )  );
#44147 = FACE_OUTER_BOUND ( 'NONE', #3884, .T. ) ;
#44148 = DIRECTION ( 'NONE',  ( -3.071710424422018668E-17, 6.404604876783312462E-16, 1.000000000000000000 ) ) ;
#44149 = EDGE_CURVE ( 'NONE', #20751, #32161, #2945, .T. ) ;
#44150 = EDGE_CURVE ( 'NONE', #44500, #48597, #42052, .T. ) ;
#44151 = CARTESIAN_POINT ( 'NONE',  ( -13.19650781164887832, -20.94374207671370058, 58.20683400836775689 ) ) ;
#44152 = CARTESIAN_POINT ( 'NONE',  ( -16.16379340615718618, -22.15191857530921382, 58.47080845268740035 ) ) ;
#44153 = CARTESIAN_POINT ( 'NONE',  ( -24.26463774145634034, -13.10332622516414069, 63.13264148103307605 ) ) ;
#44154 = EDGE_LOOP ( 'NONE', ( #46104, #36216, #14469, #43204, #31220 ) ) ;
#44155 = ORIENTED_EDGE ( 'NONE', *, *, #19631, .F. ) ;
#44156 = CARTESIAN_POINT ( 'NONE',  ( -11.46028008028683942, -18.56947564720590194, 61.56238700194530367 ) ) ;
#44157 = CARTESIAN_POINT ( 'NONE',  ( -10.47613650077225600, -13.59292889141194216, 74.88637490168683541 ) ) ;
#44158 = ORIENTED_EDGE ( 'NONE', *, *, #35349, .T. ) ;
#44160 = CARTESIAN_POINT ( 'NONE',  ( -17.07160637253920044, -10.12398423200249553, 52.02966884056656482 ) ) ;
#44159 = CARTESIAN_POINT ( 'NONE',  ( -23.99387123153590551, -11.29613222128559258, 66.46568589023691231 ) ) ;
#44161 = CARTESIAN_POINT ( 'NONE',  ( -24.19351354463141845, -13.02564601667185151, 66.31863419436056972 ) ) ;
#44162 = CARTESIAN_POINT ( 'NONE',  ( -11.77467277675836321, -9.951459619914194477, 64.14259051640634368 ) ) ;
#44163 = CARTESIAN_POINT ( 'NONE',  ( -12.15470796376391682, -20.07677110164151557, 61.51023378490003068 ) ) ;
#44164 = FACE_BOUND ( 'NONE', #29905, .T. ) ;
#44165 = FACE_BOUND ( 'NONE', #8302, .T. ) ;
#44166 = CARTESIAN_POINT ( 'NONE',  ( -24.82750195234013191, -13.97654432178796569, 73.30766915316792165 ) ) ;
#44167 = LINE ( 'NONE', #18009, #5119 ) ;
#44168 = CARTESIAN_POINT ( 'NONE',  ( -11.49500183448702906, -10.99442376238782515, 57.22375354680192316 ) ) ;
#44169 = EDGE_CURVE ( 'NONE', #40684, #25938, #38855, .T. ) ;
#44170 = VERTEX_POINT ( 'NONE', #35132 ) ;
#44171 = AXIS2_PLACEMENT_3D ( 'NONE', #8568, #23592, #39074 ) ;
#44172 = CARTESIAN_POINT ( 'NONE',  ( -50.42609385541305755, -14.80920654474413745, 60.91764705882351905 ) ) ;
#44173 = DIRECTION ( 'NONE',  ( 3.549360974554993999E-17, -6.371834667797928663E-18, -1.000000000000000000 ) ) ;
#44174 = DIRECTION ( 'NONE',  ( -2.083496777882594458E-06, 1.347747145367441676E-07, 0.9999999999978204102 ) ) ;
#44175 = CARTESIAN_POINT ( 'NONE',  ( -20.82683693055541596, -21.43676851416161355, 58.83813467579677337 ) ) ;
#44176 = CARTESIAN_POINT ( 'NONE',  ( -11.22470860480879118, -11.43539691024457206, 71.23293728648457090 ) ) ;
#44177 = CARTESIAN_POINT ( 'NONE',  ( -16.46055793053448113, -21.74386666130517298, 65.45394323774524992 ) ) ;
#44178 = ORIENTED_EDGE ( 'NONE', *, *, #30490, .F. ) ;
#44179 = EDGE_LOOP ( 'NONE', ( #30517, #28504, #8853, #41104, #23654 ) ) ;
#44180 = CARTESIAN_POINT ( 'NONE',  ( -19.14909385541304232, -8.112991634885936776, 51.74999426922421719 ) ) ;
#44181 = ORIENTED_EDGE ( 'NONE', *, *, #43252, .T. ) ;
#44182 = CARTESIAN_POINT ( 'NONE',  ( -17.13276323845814630, -21.80314153100133723, 72.35646425281650806 ) ) ;
#44183 = AXIS2_PLACEMENT_3D ( 'NONE', #587, #15582, #30645 ) ;
#44184 = CARTESIAN_POINT ( 'NONE',  ( -20.11563963094288354, -8.345964892081962461, 73.94926364880660685 ) ) ;
#44185 = B_SPLINE_CURVE_WITH_KNOTS ( 'NONE', 3,
 ( #29586, #298, #11125, #41396, #26381, #7688, #47, #10405, #48292, #2992 ),
 .UNSPECIFIED., .F., .F.,
 ( 4, 2, 2, 2, 4 ),
 ( 0.000000000000000000, 0.2500000000000000000, 0.5000000000000000000, 0.7500000000000000000, 1.000000000000000000 ),
 .UNSPECIFIED. ) ;
#44186 = CARTESIAN_POINT ( 'NONE',  ( -15.42576764927216892, -7.632088794545897947, 74.25798431274822065 ) ) ;
#44187 = DIRECTION ( 'NONE',  ( -3.071710424422018668E-17, 6.404604876783312462E-16, 1.000000000000000000 ) ) ;
#44188 = VERTEX_POINT ( 'NONE', #31447 ) ;
#44189 = APPLICATION_CONTEXT ( 'automotive_design' ) ;
#44190 = CARTESIAN_POINT ( 'NONE',  ( -19.37616851487812752, -21.99900361761337919, 58.71002773933979313 ) ) ;
#44191 = AXIS2_PLACEMENT_3D ( 'NONE', #33048, #21518, #48091 ) ;
#44192 = DIRECTION ( 'NONE',  ( -0.9687793358424819923, 0.2479245821708680464, 0.000000000000000000 ) ) ;
#44193 = VERTEX_POINT ( 'NONE', #23338 ) ;
#44194 = LINE ( 'NONE', #29143, #27300 ) ;
#44195 = CARTESIAN_POINT ( 'NONE',  ( -20.44284385541303095, -7.587656875400184298, 49.25157356644812268 ) ) ;
#44196 = ORIENTED_EDGE ( 'NONE', *, *, #27398, .F. ) ;
#44197 = CARTESIAN_POINT ( 'NONE',  ( -21.35412623182586955, -20.66579906811421452, 68.93961316870652922 ) ) ;
#44198 = DIRECTION ( 'NONE',  ( -1.069446448411283641E-06, 1.103879804260444988E-06, -0.9999999999988188337 ) ) ;
#44199 = ORIENTED_EDGE ( 'NONE', *, *, #32345, .F. ) ;
#44200 = CARTESIAN_POINT ( 'NONE',  ( -21.42170527289675164, -17.27794275993632667, 49.52966884056655772 ) ) ;
#44201 = EDGE_CURVE ( 'NONE', #34833, #42067, #26565, .T. ) ;
#44202 = CIRCLE ( 'NONE', #27653, 1.249999999999999334 ) ;
#44203 = CARTESIAN_POINT ( 'NONE',  ( -48.42409385541304800, -25.10920654474410441, 81.99999999999998579 ) ) ;
#44204 = CARTESIAN_POINT ( 'NONE',  ( -15.28291064399146215, -21.52618758091310980, 68.57592918174772478 ) ) ;
#44205 = ORIENTED_EDGE ( 'NONE', *, *, #33934, .F. ) ;
#44206 = DIRECTION ( 'NONE',  ( 0.9774082387306983755, -0.2113602016968848529, 7.903122840289807171E-08 ) ) ;
#44207 = CARTESIAN_POINT ( 'NONE',  ( -35.32409385541306079, -6.359206544744109735, 48.79999999999998295 ) ) ;
#44208 = CARTESIAN_POINT ( 'NONE',  ( -23.83043773139749533, -11.86620498678314561, 59.78235732590890450 ) ) ;
#44209 = EDGE_CURVE ( 'NONE', #20573, #13987, #42549, .T. ) ;
#44210 = VECTOR ( 'NONE', #48204, 1000.000000000000114 ) ;
#44211 = CARTESIAN_POINT ( 'NONE',  ( -11.73296596577226936, -10.64774513788296240, 74.72412863062541533 ) ) ;
#44212 = EDGE_CURVE ( 'NONE', #34242, #1270, #39072, .T. ) ;
#44213 = DIRECTION ( 'NONE',  ( -1.000000000000000000, -2.866981220435666553E-17, -0.000000000000000000 ) ) ;
#44214 = CARTESIAN_POINT ( 'NONE',  ( -12.05806040642128707, -10.23620046216302448, 67.51368956197082127 ) ) ;
#44215 = ORIENTED_EDGE ( 'NONE', *, *, #11515, .T. ) ;
#44216 = CARTESIAN_POINT ( 'NONE',  ( -15.03427660820159772, -21.44211488324610571, 65.12068745241758450 ) ) ;
#44217 = EDGE_CURVE ( 'NONE', #10695, #13075, #43345, .T. ) ;
#44218 = DIRECTION ( 'NONE',  ( -0.9893521221787096032, 0.1455416721783832079, 6.188545272020285247E-08 ) ) ;
#44219 = VERTEX_POINT ( 'NONE', #933 ) ;
#44220 = DIRECTION ( 'NONE',  ( 0.000000000000000000, 0.000000000000000000, 1.000000000000000000 ) ) ;
#44221 = ORIENTED_EDGE ( 'NONE', *, *, #30635, .F. ) ;
#44222 = VERTEX_POINT ( 'NONE', #19396 ) ;
#44223 = ORIENTED_EDGE ( 'NONE', *, *, #28098, .F. ) ;
#44224 = CARTESIAN_POINT ( 'NONE',  ( -16.19813999035177332, -21.75179513556690480, 58.28585572029249562 ) ) ;
#44225 = LINE ( 'NONE', #10704, #20052 ) ;
#44226 = DIRECTION ( 'NONE',  ( -3.827383491158052452E-06, 8.363078748037870009E-06, 0.9999999999577049437 ) ) ;
#44227 = CARTESIAN_POINT ( 'NONE',  ( -12.80657247161177814, -9.477853225175101315, 70.73436560138682694 ) ) ;
#44228 = ORIENTED_EDGE ( 'NONE', *, *, #3571, .T. ) ;
#44229 = ORIENTED_EDGE ( 'NONE', *, *, #28706, .T. ) ;
#44230 = CARTESIAN_POINT ( 'NONE',  ( -17.04284385650551670, -8.811426318492348031, 52.18089403414751359 ) ) ;
#44231 = DIRECTION ( 'NONE',  ( -0.9524241471993249997, -0.3047743298226212594, -0.0009228828802129952422 ) ) ;
#44232 = CYLINDRICAL_SURFACE ( 'NONE', #33915, 1.249999999999998668 ) ;
#44233 = CARTESIAN_POINT ( 'NONE',  ( -19.12409385650551741, -6.426201560718813433, 50.50509628382439331 ) ) ;
#44234 = ORIENTED_EDGE ( 'NONE', *, *, #28952, .T. ) ;
#44235 = CARTESIAN_POINT ( 'NONE',  ( -17.42409385541300892, -14.80920654474439324, 53.49899999999994549 ) ) ;
#44236 = CYLINDRICAL_SURFACE ( 'NONE', #30746, 0.1500000000000035749 ) ;
#44237 = DIRECTION ( 'NONE',  ( -2.872222159185455981E-06, 2.507089443456002334E-06, 0.9999999999927324801 ) ) ;
#44238 = EDGE_CURVE ( 'NONE', #32800, #2641, #1257, .T. ) ;
#44239 = ORIENTED_EDGE ( 'NONE', *, *, #47184, .T. ) ;
#44240 = CARTESIAN_POINT ( 'NONE',  ( -10.42334066387008029, -15.64104445138816324, 61.03789045260960933 ) ) ;
#44241 = EDGE_LOOP ( 'NONE', ( #10872, #32590, #44155, #9137 ) ) ;
#44242 = CARTESIAN_POINT ( 'NONE',  ( -20.83700022493356130, -19.12221826660257307, 53.49999999999995026 ) ) ;
#44243 = CARTESIAN_POINT ( 'NONE',  ( -15.12736045941317897, -21.89643407171298151, 68.69097498501147925 ) ) ;
#44244 = CARTESIAN_POINT ( 'NONE',  ( -24.42364817991657588, -14.92042613324309208, 59.52683630610148668 ) ) ;
#44245 = VERTEX_POINT ( 'NONE', #30740 ) ;
#44246 = CARTESIAN_POINT ( 'NONE',  ( -24.09823712565756182, -12.53788967028716783, 73.54225559392006062 ) ) ;
#44247 = CARTESIAN_POINT ( 'NONE',  ( -16.89909385541303877, -8.105421454601382081, 49.25000573077640098 ) ) ;
#44248 = LINE ( 'NONE', #22066, #23708 ) ;
#44249 = VERTEX_POINT ( 'NONE', #45767 ) ;
#44250 = CARTESIAN_POINT ( 'NONE',  ( -24.82559196212071484, -15.65839247127784972, 73.11029605187583513 ) ) ;
#44251 = CYLINDRICAL_SURFACE ( 'NONE', #3808, 0.1500000000000073774 ) ;
#44252 = CARTESIAN_POINT ( 'NONE',  ( -10.96921284960095377, -11.97350354382807680, 74.84368195529052059 ) ) ;
#44253 = ORIENTED_EDGE ( 'NONE', *, *, #31751, .F. ) ;
#44254 = CARTESIAN_POINT ( 'NONE',  ( -13.24006525392636391, -20.97423447465198976, 61.70301720779925603 ) ) ;
#44255 = VERTEX_POINT ( 'NONE', #5838 ) ;
#44256 = CARTESIAN_POINT ( 'NONE',  ( -12.40538999107997498, -20.31523868419091272, 68.52152871938794476 ) ) ;
#44257 = CARTESIAN_POINT ( 'NONE',  ( -13.77338061488629073, -21.30427811955188844, 68.56969753575143045 ) ) ;
#44258 = CARTESIAN_POINT ( 'NONE',  ( -24.42003622094757276, -14.56910621572103715, 62.99831180156633081 ) ) ;
#44259 = EDGE_CURVE ( 'NONE', #11465, #30525, #26950, .T. ) ;
#44260 = CARTESIAN_POINT ( 'NONE',  ( -9.424093855413051557, -25.10920654474410441, 78.99999999999998579 ) ) ;
#44261 = ORIENTED_EDGE ( 'NONE', *, *, #47231, .T. ) ;
#44262 = CARTESIAN_POINT ( 'NONE',  ( -24.18037252889021005, -17.94870914462638822, 59.18873732074431615 ) ) ;
#44263 = ADVANCED_FACE ( 'NONE', ( #21347 ), #9542, .T. ) ;
#44264 = CARTESIAN_POINT ( 'NONE',  ( -18.99427849551180358, -7.526545565697431606, 67.10060551660288297 ) ) ;
#44265 =( BOUNDED_CURVE ( )  B_SPLINE_CURVE ( 3, ( #11282, #19147, #33920, #34647 ),
 .UNSPECIFIED., .F., .F. ) 
 B_SPLINE_CURVE_WITH_KNOTS ( ( 4, 4 ),
 ( 0.000000000000000000, 0.4074455897393777226 ),
 .UNSPECIFIED. ) 
 CURVE ( )  GEOMETRIC_REPRESENTATION_ITEM ( )  RATIONAL_B_SPLINE_CURVE ( ( 1.000000000000000000, 0.4567392136813100967, 0.3561768502900222177, 0.6983129098261363632 ) ) 
 REPRESENTATION_ITEM ( '' )  );
#44266 = CARTESIAN_POINT ( 'NONE',  ( -15.35181094580836358, -7.653138554841501850, 74.12339718037890179 ) ) ;
#44267 = ORIENTED_EDGE ( 'NONE', *, *, #22073, .T. ) ;
#44268 = CARTESIAN_POINT ( 'NONE',  ( -10.37795889460693033, -14.56696403379599403, 68.14328054657653411 ) ) ;
#44269 = ADVANCED_FACE ( 'NONE', ( #9292 ), #29813, .T. ) ;
#44270 = CARTESIAN_POINT ( 'NONE',  ( -12.23301264461619553, -10.03852782535897958, 60.84446034103241630 ) ) ;
#44271 = EDGE_LOOP ( 'NONE', ( #40049, #12156, #41121, #938, #28689 ) ) ;
#44272 = VERTEX_POINT ( 'NONE', #32423 ) ;
#44273 = CARTESIAN_POINT ( 'NONE',  ( -14.99555751708010121, -21.85235056220836469, 65.14950770721691242 ) ) ;
#44274 = CARTESIAN_POINT ( 'NONE',  ( -19.88526120935579655, -21.36290167704760279, 72.68255599050156945 ) ) ;
#44275 = CARTESIAN_POINT ( 'NONE',  ( -15.82259855879412846, -7.533287975791289171, 67.25511890406325222 ) ) ;
#44277 = EDGE_CURVE ( 'NONE', #43233, #26444, #42302, .T. ) ;
#44276 = CARTESIAN_POINT ( 'NONE',  ( -23.89200535028185612, -11.11192396016905448, 70.07706043178237110 ) ) ;
#44278 = CARTESIAN_POINT ( 'NONE',  ( -24.23813412381375088, -12.99935709875259526, 66.31718868320673721 ) ) ;
#44279 = LINE ( 'NONE', #36369, #31064 ) ;
#44280 = CARTESIAN_POINT ( 'NONE',  ( -13.21784385759799108, -6.860780111191489006, 51.02154966934379132 ) ) ;
#44281 =( BOUNDED_SURFACE ( )  B_SPLINE_SURFACE ( 3, 1, ( 
 ( #4139, #442 ),
 ( #15417, #30486 ),
 ( #45499, #11757 ),
 ( #41801, #8082 ),
 ( #38083, #670 ),
 ( #19378, #31917 ),
 ( #39782, #43740 ) ),
 .UNSPECIFIED., .T., .F., .F. ) 
 B_SPLINE_SURFACE_WITH_KNOTS ( ( 4, 3, 4 ),
 ( 2, 2 ),
 ( 0.000000000000000000, 0.5000000000000000000, 1.000000000000000000 ),
 ( 0.000000000000000000, 1.000000000000000000 ),
 .UNSPECIFIED. ) 
 GEOMETRIC_REPRESENTATION_ITEM ( )  RATIONAL_B_SPLINE_SURFACE ( (
 ( 1.000000000000000000, 1.000000000000000000),
 ( 0.3333333333333335369, 0.3333333333333330373),
 ( 0.3333333333333335369, 0.3333333333333330373),
 ( 1.000000000000000000, 1.000000000000000000),
 ( 0.3333333333333333703, 0.3333333333333333703),
 ( 0.3333333333333333703, 0.3333333333333333703),
 ( 1.000000000000000000, 1.000000000000000000) ) ) 
 REPRESENTATION_ITEM ( '' )  SURFACE ( )  );
#44282 = ORIENTED_EDGE ( 'NONE', *, *, #1704, .F. ) ;
#44283 = EDGE_LOOP ( 'NONE', ( #5954, #12600, #27041, #12762 ) ) ;
#44284 = CARTESIAN_POINT ( 'NONE',  ( -13.43921731646364925, -8.993429882417945720, 60.43950277494440826 ) ) ;
#44285 = CARTESIAN_POINT ( 'NONE',  ( -17.32409385759798681, -9.359200813967568422, 50.49621490985803263 ) ) ;
#44286 = CARTESIAN_POINT ( 'NONE',  ( -23.76176040870155148, -11.71284927192775527, 66.51394613547601864 ) ) ;
#44287 = CARTESIAN_POINT ( 'NONE',  ( -13.88539965413766453, -8.253282245057402378, 74.34954655571560522 ) ) ;
#44288 = CARTESIAN_POINT ( 'NONE',  ( -13.17762867948185601, -11.72213130924974678, 49.52966884056655772 ) ) ;
#44289 = ORIENTED_EDGE ( 'NONE', *, *, #36200, .F. ) ;
#44290 = CARTESIAN_POINT ( 'NONE',  ( -18.86784385650551954, -6.428312510596451368, 51.20221977374900035 ) ) ;
#44291 = VERTEX_POINT ( 'NONE', #9780 ) ;
#44292 = CARTESIAN_POINT ( 'NONE',  ( -24.33858675457341292, -15.90816096490859088, 69.60477842452804964 ) ) ;
#44293 = CARTESIAN_POINT ( 'NONE',  ( -45.55409385541305767, -14.20920654474410760, 69.94787228701220272 ) ) ;
#44294 = AXIS2_PLACEMENT_3D ( 'NONE', #34834, #7787, #1106 ) ;
#44295 = PLANE ( 'NONE',  #22958 ) ;
#44296 = CARTESIAN_POINT ( 'NONE',  ( -11.17079691907060202, -18.85905423163385564, 64.90853625290334605 ) ) ;
#44297 = EDGE_CURVE ( 'NONE', #19689, #20521, #41528, .T. ) ;
#44298 = ORIENTED_EDGE ( 'NONE', *, *, #38227, .T. ) ;
#44299 = CARTESIAN_POINT ( 'NONE',  ( -24.72409385541305582, -14.80920654474426357, 72.98823529411762934 ) ) ;
#44300 = CARTESIAN_POINT ( 'NONE',  ( -23.85820194903862657, -17.69173191509663567, 62.48833042115954584 ) ) ;
#44301 = ORIENTED_EDGE ( 'NONE', *, *, #5603, .T. ) ;
#44302 = CARTESIAN_POINT ( 'NONE',  ( -24.20371252810814866, -12.87440185077122834, 66.58774614429587757 ) ) ;
#44303 = CARTESIAN_POINT ( 'NONE',  ( -21.34582024633207098, -20.66775256773563285, 72.67446429491059234 ) ) ;
#44304 = ORIENTED_EDGE ( 'NONE', *, *, #43461, .F. ) ;
#44305 = EDGE_CURVE ( 'NONE', #9970, #6766, #6067, .T. ) ;
#44306 = FACE_OUTER_BOUND ( 'NONE', #25755, .T. ) ;
#44307 = ORIENTED_EDGE ( 'NONE', *, *, #30238, .F. ) ;
#44308 = CARTESIAN_POINT ( 'NONE',  ( -21.71330648800491048, -9.209429688968461036, 70.43132803184890633 ) ) ;
#44309 = CARTESIAN_POINT ( 'NONE',  ( -24.31477923169101629, -16.30090137217950996, 59.40860294853779777 ) ) ;
#44310 = VERTEX_POINT ( 'NONE', #2130 ) ;
#44311 = CARTESIAN_POINT ( 'NONE',  ( -18.42425741750128765, -21.73782862702753249, 72.30127622548401689 ) ) ;
#44312 = CARTESIAN_POINT ( 'NONE',  ( -24.40650426928521100, -17.40698345136521752, 69.56339792804031674 ) ) ;
#44313 = EDGE_CURVE ( 'NONE', #32762, #44898, #2184, .T. ) ;
#44314 = ORIENTED_EDGE ( 'NONE', *, *, #13950, .T. ) ;
#44315 = CARTESIAN_POINT ( 'NONE',  ( -18.71756812234623979, -7.929749856837892352, 70.67068030594712980 ) ) ;
#44316 = CARTESIAN_POINT ( 'NONE',  ( -11.11213569393138023, -18.76700539655533362, 61.41564285493458897 ) ) ;
#44317 = CARTESIAN_POINT ( 'NONE',  ( -21.59705452237689371, -8.637577456526162933, 73.80139960705861313 ) ) ;
#44318 = ORIENTED_EDGE ( 'NONE', *, *, #6334, .F. ) ;
#44319 = CARTESIAN_POINT ( 'NONE',  ( -13.51260394713023416, -21.14978044785226530, 65.18617648760555028 ) ) ;
#44320 = EDGE_CURVE ( 'NONE', #19297, #32762, #8486, .T. ) ;
#44321 = DIRECTION ( 'NONE',  ( 0.8839923186919885767, -0.4675014229855998793, 2.842058574697910297E-08 ) ) ;
#44322 = LINE ( 'NONE', #25353, #22339 ) ;
#44323 = AXIS2_PLACEMENT_3D ( 'NONE', #6986, #44920, #17568 ) ;
#44324 = ORIENTED_EDGE ( 'NONE', *, *, #21760, .T. ) ;
#44325 = ORIENTED_EDGE ( 'NONE', *, *, #24068, .F. ) ;
#44326 = CARTESIAN_POINT ( 'NONE',  ( -22.57893663749957369, -9.999394138389963160, 73.49633153340955971 ) ) ;
#44327 = CARTESIAN_POINT ( 'NONE',  ( -16.93043456194158125, -7.826573929305837396, 74.24552922955767542 ) ) ;
#44328 = CARTESIAN_POINT ( 'NONE',  ( -11.44771684537310463, -11.06942230959719176, 57.50903181645943363 ) ) ;
#44329 = ADVANCED_FACE ( 'NONE', ( #17856 ), #32879, .T. ) ;
#44330 = CARTESIAN_POINT ( 'NONE',  ( -16.81784385759798894, -6.860780111191487229, 51.02154966934377001 ) ) ;
#44331 = CARTESIAN_POINT ( 'NONE',  ( -23.21283114448125673, -10.11939864774917908, 63.25681283445349123 ) ) ;
#44332 = CARTESIAN_POINT ( 'NONE',  ( -12.90227214125716237, -8.888328675545798419, 67.63588728319849963 ) ) ;
#44333 = CARTESIAN_POINT ( 'NONE',  ( -23.68746034620986762, -18.84317387556108514, 69.39348344656710310 ) ) ;
#44334 = DIRECTION ( 'NONE',  ( -5.517078746805382707E-07, -1.257343593493847808E-06, -0.9999999999990573096 ) ) ;
#44335 = ORIENTED_EDGE ( 'NONE', *, *, #27122, .F. ) ;
#44336 = DIRECTION ( 'NONE',  ( 2.696738943264045022E-06, 1.002714486673431828E-05, 0.9999999999460920108 ) ) ;
#44337 = CARTESIAN_POINT ( 'NONE',  ( -18.31357640787765462, -21.80286941108919763, 68.81514702304139064 ) ) ;
#44338 = CARTESIAN_POINT ( 'NONE',  ( -14.33701861991840154, -19.05567172067550530, 52.02966884056656482 ) ) ;
#44339 = EDGE_CURVE ( 'NONE', #20830, #21555, #36339, .T. ) ;
#44340 = ADVANCED_FACE ( 'NONE', ( #17621 ), #47200, .F. ) ;
#44341 = VERTEX_POINT ( 'NONE', #35614 ) ;
#44342 = EDGE_LOOP ( 'NONE', ( #46081, #12221, #25670, #45953 ) ) ;
#44343 = ADVANCED_FACE ( 'NONE', ( #31931 ), #39562, .T. ) ;
#44344 = FACE_OUTER_BOUND ( 'NONE', #48412, .T. ) ;
#44345 = SURFACE_STYLE_FILL_AREA ( #3202 ) ;
#44346 = CARTESIAN_POINT ( 'NONE',  ( -10.00655543316878493, -14.11314255069943258, 61.09538170931386958 ) ) ;
#44347 = CARTESIAN_POINT ( 'NONE',  ( -24.30515140815569097, -13.27439714384899183, 59.65708100345488418 ) ) ;
#44348 =( BOUNDED_CURVE ( )  B_SPLINE_CURVE ( 3, ( #3185, #6163, #21189, #29533 ),
 .UNSPECIFIED., .F., .F. ) 
 B_SPLINE_CURVE_WITH_KNOTS ( ( 4, 4 ),
 ( 0.9074455897393657322, 1.000000000000000000 ),
 .UNSPECIFIED. ) 
 CURVE ( )  GEOMETRIC_REPRESENTATION_ITEM ( )  RATIONAL_B_SPLINE_CURVE ( ( 0.6983129098260905110, 0.7760317562606959818, 0.8765941196519991818, 1.000000000000000000 ) ) 
 REPRESENTATION_ITEM ( '' )  );
#44349 = VERTEX_POINT ( 'NONE', #29209 ) ;
#44350 = CARTESIAN_POINT ( 'NONE',  ( -12.50766578132126838, -19.86205079821699471, 65.16674886870754335 ) ) ;
#44351 = FACE_OUTER_BOUND ( 'NONE', #28787, .T. ) ;
#44352 = CIRCLE ( 'NONE', #37252, 4.686499999999997002 ) ;
#44353 = ORIENTED_EDGE ( 'NONE', *, *, #23395, .T. ) ;
#44354 = DIRECTION ( 'NONE',  ( 2.775557561562888984E-15, 0.000000000000000000, -1.000000000000000000 ) ) ;
#44355 = CARTESIAN_POINT ( 'NONE',  ( -19.69975549639545420, -21.90326680182264596, 65.64298972507442897 ) ) ;
#44356 = CARTESIAN_POINT ( 'NONE',  ( -22.87867891474110849, -19.28048576922455837, 59.29899440274890310 ) ) ;
#44357 = VERTEX_POINT ( 'NONE', #48394 ) ;
#44358 = CARTESIAN_POINT ( 'NONE',  ( -28.42409385541305511, -25.10920654474410441, 47.99999999999997868 ) ) ;
#44359 = VERTEX_POINT ( 'NONE', #29947 ) ;
#44360 = CARTESIAN_POINT ( 'NONE',  ( -10.46561413896930581, -17.47044525196274734, 64.82728164928992953 ) ) ;
#44361 = CARTESIAN_POINT ( 'NONE',  ( -24.40217300928714650, -14.25566238011515274, 69.65275273531472067 ) ) ;
#44362 = ORIENTED_EDGE ( 'NONE', *, *, #12621, .F. ) ;
#44363 = CARTESIAN_POINT ( 'NONE',  ( -10.41336640449534734, -12.28884930470453085, 57.47857332146136855 ) ) ;
#44364 = CARTESIAN_POINT ( 'NONE',  ( -20.03165646395635591, -8.259115988876370551, 73.72096593878789861 ) ) ;
#44365 = CARTESIAN_POINT ( 'NONE',  ( -12.64995480627295521, -19.99670077279894898, 68.48657438322858582 ) ) ;
#44366 = CARTESIAN_POINT ( 'NONE',  ( -24.01844669341070926, -17.32505205508840262, 62.62928254837112974 ) ) ;
#44367 = CARTESIAN_POINT ( 'NONE',  ( -13.94909385759799214, -8.112991634885936776, 51.74999426922421719 ) ) ;
#44368 = DIRECTION ( 'NONE',  ( 0.9271861211590526342, 0.3746009833543293421, -1.005599061620490611E-08 ) ) ;
#44369 = ORIENTED_EDGE ( 'NONE', *, *, #16880, .F. ) ;
#44370 = B_SPLINE_CURVE_WITH_KNOTS ( 'NONE', 3,
 ( #46218, #8807, #23823, #5102, #9278, #20112, #35120, #39057, #1640, #16650 ),
 .UNSPECIFIED., .F., .F.,
 ( 4, 2, 2, 2, 4 ),
 ( 0.000000000000000000, 0.2500000000000000000, 0.5000000000000000000, 0.7500000000000000000, 1.000000000000000000 ),
 .UNSPECIFIED. ) ;
#44371 = DIRECTION ( 'NONE',  ( 0.9048399035850772654, 0.4257519804770707461, 1.330923649722295902E-08 ) ) ;
#44372 = DIRECTION ( 'NONE',  ( -0.9529680021988313765, 0.3030709269876716849, 3.918663088761644638E-08 ) ) ;
#44373 = DIRECTION ( 'NONE',  ( 3.071710424422018668E-17, -6.404604876783312462E-16, -1.000000000000000000 ) ) ;
#44374 = DIRECTION ( 'NONE',  ( -0.9893521221787096032, 0.1455416721783832079, 6.188545272020283923E-08 ) ) ;
#44375 = EDGE_CURVE ( 'NONE', #45181, #20101, #25508, .T. ) ;
#44376 = CARTESIAN_POINT ( 'NONE',  ( -13.35969120262891430, -20.57410711936033820, 61.60826610285024429 ) ) ;
#44377 = CARTESIAN_POINT ( 'NONE',  ( -13.02466918351366054, -9.790356719747981273, 49.88236859574130477 ) ) ;
#44378 = EDGE_LOOP ( 'NONE', ( #34531, #45641, #4359, #17155 ) ) ;
#44379 = VERTEX_POINT ( 'NONE', #14153 ) ;
#44380 = CARTESIAN_POINT ( 'NONE',  ( -21.39914427356725213, -17.29159580171668864, 52.02966884056656482 ) ) ;
#44381 = CARTESIAN_POINT ( 'NONE',  ( -9.974456273375457371, -14.72748566909688073, 71.51278126739182994 ) ) ;
#44382 = EDGE_LOOP ( 'NONE', ( #41709, #48056, #31600, #39410, #39115 ) ) ;
#44383 = CARTESIAN_POINT ( 'NONE',  ( -13.33034385650551812, -9.794322478646142471, 51.19202720610083901 ) ) ;
#44384 = CARTESIAN_POINT ( 'NONE',  ( -24.16575310113231012, -12.74704012323608104, 70.07243002239954421 ) ) ;
#44385 = FACE_OUTER_BOUND ( 'NONE', #2727, .T. ) ;
#44386 = FACE_BOUND ( 'NONE', #43553, .T. ) ;
#44387 = CARTESIAN_POINT ( 'NONE',  ( -24.82598972713961771, -13.96249193466810823, 73.26124986525175586 ) ) ;
#44388 = CARTESIAN_POINT ( 'NONE',  ( -10.42462062184586635, -14.89508117765250361, 75.09778901762284420 ) ) ;
#44389 = VECTOR ( 'NONE', #17822, 1000.000000000000227 ) ;
#44390 = ORIENTED_EDGE ( 'NONE', *, *, #44465, .F. ) ;
#44391 = VECTOR ( 'NONE', #10573, 1000.000000000000000 ) ;
#44392 = FACE_OUTER_BOUND ( 'NONE', #21582, .T. ) ;
#44393 = CARTESIAN_POINT ( 'NONE',  ( -12.72364920584387349, -9.064356868646193277, 49.69365772853683438 ) ) ;
#44394 = ADVANCED_BREP_SHAPE_REPRESENTATION ( '', ( #32048, #29031 ), #9367 ) ;
#44395 = CARTESIAN_POINT ( 'NONE',  ( -24.69822963474414479, -13.19963333263893190, 59.54763306486673713 ) ) ;
#44396 = DIRECTION ( 'NONE',  ( -0.3037135924646501839, 0.9527633776296273727, 2.170275161112374231E-08 ) ) ;
#44397 = CARTESIAN_POINT ( 'NONE',  ( -12.00790786851990610, -10.29148984397945377, 63.91425679989585973 ) ) ;
#44398 =( BOUNDED_CURVE ( )  B_SPLINE_CURVE ( 3, ( #9301, #42059, #42557, #27995 ),
 .UNSPECIFIED., .F., .F. ) 
 B_SPLINE_CURVE_WITH_KNOTS ( ( 4, 4 ),
 ( 0.9074455897393648440, 1.000000000000000000 ),
 .UNSPECIFIED. ) 
 CURVE ( )  GEOMETRIC_REPRESENTATION_ITEM ( )  RATIONAL_B_SPLINE_CURVE ( ( 0.6983129098260973944, 0.7760317562607019770, 0.8765941196520028456, 1.000000000000000000 ) ) 
 REPRESENTATION_ITEM ( '' )  );
#44399 = CARTESIAN_POINT ( 'NONE',  ( -14.66790711817407278, -21.29843871104708342, 58.18089935161520287 ) ) ;
#44400 = CARTESIAN_POINT ( 'NONE',  ( -16.59344411340201475, -21.75974756046277747, 65.22564390621562325 ) ) ;
#44402 = ORIENTED_EDGE ( 'NONE', *, *, #41307, .F. ) ;
#44401 = EDGE_CURVE ( 'NONE', #28413, #20803, #33603, .T. ) ;
#44403 = ORIENTED_EDGE ( 'NONE', *, *, #20671, .F. ) ;
#44404 = CARTESIAN_POINT ( 'NONE',  ( -15.26784385541304090, -9.357632978295830739, 49.97845033065684106 ) ) ;
#44405 = EDGE_LOOP ( 'NONE', ( #17719, #21087, #38440, #3755, #3271 ) ) ;
#44406 = ADVANCED_FACE ( 'NONE', ( #11462 ), #7302, .T. ) ;
#44407 = EDGE_CURVE ( 'NONE', #45657, #26697, #26005, .T. ) ;
#44408 = CARTESIAN_POINT ( 'NONE',  ( -17.43166586245951422, -7.359124596637800053, 67.13544155391683432 ) ) ;
#44409 = CARTESIAN_POINT ( 'NONE',  ( -18.85724798917316392, -7.906108138700305155, 67.18599644112759961 ) ) ;
#44410 =( BOUNDED_CURVE ( )  B_SPLINE_CURVE ( 3, ( #10111, #25132, #7397, #41115 ),
 .UNSPECIFIED., .F., .F. ) 
 B_SPLINE_CURVE_WITH_KNOTS ( ( 4, 4 ),
 ( 0.5000000000000000000, 0.9074455897393650661 ),
 .UNSPECIFIED. ) 
 CURVE ( )  GEOMETRIC_REPRESENTATION_ITEM ( )  RATIONAL_B_SPLINE_CURVE ( ( 1.000000000000001998, 0.4567392136813319681, 0.3561768502900288791, 0.6983129098260947298 ) ) 
 REPRESENTATION_ITEM ( '' )  );
#44411 = CARTESIAN_POINT ( 'NONE',  ( -17.42409385541299471, -14.80920654474435771, 49.52966884056655772 ) ) ;
#44412 = CARTESIAN_POINT ( 'NONE',  ( -12.96596534320165972, -9.347742485070138940, 70.84925352874383009 ) ) ;
#44413 = ORIENTED_EDGE ( 'NONE', *, *, #44679, .T. ) ;
#44414 = CARTESIAN_POINT ( 'NONE',  ( -13.65828898514496537, -20.76952646431350757, 65.00101022825411690 ) ) ;
#44415 = CYLINDRICAL_SURFACE ( 'NONE', #4479, 2.000000000000001332 ) ;
#44416 = ORIENTED_EDGE ( 'NONE', *, *, #39823, .F. ) ;
#44417 = CARTESIAN_POINT ( 'NONE',  ( -10.37185532365394813, -14.67000050818549184, 74.88959094244134462 ) ) ;
#44418 = DIRECTION ( 'NONE',  ( -3.071710424422018668E-17, 6.404604876783312462E-16, 1.000000000000000000 ) ) ;
#44419 =( BOUNDED_SURFACE ( )  B_SPLINE_SURFACE ( 3, 1, ( 
 ( #47322, #28600 ),
 ( #47068, #9887 ),
 ( #9408, #39186 ),
 ( #13554, #39675 ),
 ( #5476, #5947 ),
 ( #39440, #36442 ),
 ( #2244, #36211 ) ),
 .UNSPECIFIED., .T., .F., .F. ) 
 B_SPLINE_SURFACE_WITH_KNOTS ( ( 4, 3, 4 ),
 ( 2, 2 ),
 ( 0.000000000000000000, 0.5000000000000000000, 1.000000000000000000 ),
 ( 0.000000000000000000, 1.000000000000000000 ),
 .UNSPECIFIED. ) 
 GEOMETRIC_REPRESENTATION_ITEM ( )  RATIONAL_B_SPLINE_SURFACE ( (
 ( 1.000000000000000000, 1.000000000000000000),
 ( 0.3333333333333335369, 0.3333333333333330373),
 ( 0.3333333333333335369, 0.3333333333333330373),
 ( 1.000000000000000000, 1.000000000000000000),
 ( 0.3333333333333333703, 0.3333333333333333703),
 ( 0.3333333333333333703, 0.3333333333333333703),
 ( 1.000000000000000000, 1.000000000000000000) ) ) 
 REPRESENTATION_ITEM ( '' )  SURFACE ( )  );
#44420 = VECTOR ( 'NONE', #39169, 1000.000000000000000 ) ;
#44421 = ORIENTED_EDGE ( 'NONE', *, *, #35121, .T. ) ;
#44422 = CARTESIAN_POINT ( 'NONE',  ( -10.55151165865014384, -17.68520938540437371, 68.28217272534745064 ) ) ;
#44423 = CARTESIAN_POINT ( 'NONE',  ( -15.12990733413706224, -8.194132228790286021, 57.03926990816982112 ) ) ;
#44424 = CARTESIAN_POINT ( 'NONE',  ( -23.42631727757699878, -10.39480074052133141, 59.78858809748042091 ) ) ;
#44425 = ORIENTED_EDGE ( 'NONE', *, *, #6120, .T. ) ;
#44426 = DIRECTION ( 'NONE',  ( -3.071710424422018668E-17, 6.404604876783312462E-16, 1.000000000000000000 ) ) ;
#44427 = EDGE_CURVE ( 'NONE', #18572, #32337, #16855, .T. ) ;
#44428 = VECTOR ( 'NONE', #30694, 1000.000000000000227 ) ;
#44429 = DIRECTION ( 'NONE',  ( 3.071710424422018668E-17, -6.404604876783312462E-16, -1.000000000000000000 ) ) ;
#44430 = CARTESIAN_POINT ( 'NONE',  ( -19.50843993236927432, -21.96177808838975665, 62.11008241541560437 ) ) ;
#44431 = LINE ( 'NONE', #7250, #30838 ) ;
#44432 = ORIENTED_EDGE ( 'NONE', *, *, #6754, .T. ) ;
#44433 = B_SPLINE_CURVE_WITH_KNOTS ( 'NONE', 1,
 ( #42143, #8407 ),
 .UNSPECIFIED., .F., .F.,
 ( 2, 2 ),
 ( 0.000000000000000000, 1.000000000000000000 ),
 .UNSPECIFIED. ) ;
#44434 = B_SPLINE_CURVE_WITH_KNOTS ( 'NONE', 3,
 ( #17656, #43783, #28523, #2647, #36366, #6348, #21379, #4969, #17161, #10291 ),
 .UNSPECIFIED., .F., .F.,
 ( 4, 2, 2, 2, 4 ),
 ( 0.1272669073658063144, 0.2522669073463020273, 0.3772669073267977957, 0.5022669073072935086, 0.6272669072877892216 ),
 .UNSPECIFIED. ) ;
#44435 = CARTESIAN_POINT ( 'NONE',  ( -4.424093855413056886, -8.109206544744111511, 49.24999999999999289 ) ) ;
#44436 = CYLINDRICAL_SURFACE ( 'NONE', #22341, 0.1500000000000077383 ) ;
#44437 = CARTESIAN_POINT ( 'NONE',  ( -23.66220297886838964, -18.88224728823589160, 69.55017934013164904 ) ) ;
#44438 = CARTESIAN_POINT ( 'NONE',  ( -22.01784385650551812, -9.790100578890868377, 49.79778022625162492 ) ) ;
#44439 = ORIENTED_EDGE ( 'NONE', *, *, #31630, .T. ) ;
#44440 = CARTESIAN_POINT ( 'NONE',  ( -24.66692207690629246, -13.06418342283853562, 63.08910124536953390 ) ) ;
#44441 = ORIENTED_EDGE ( 'NONE', *, *, #16347, .F. ) ;
#44442 = CARTESIAN_POINT ( 'NONE',  ( -19.92409385541305511, -14.80920654474410725, 45.99899999999998101 ) ) ;
#44443 = DIRECTION ( 'NONE',  ( -3.071710424422018668E-17, 6.404604876783312462E-16, 1.000000000000000000 ) ) ;
#44444 = DIRECTION ( 'NONE',  ( 0.9979768094191903138, 0.06357898915123821881, 0.000000000000000000 ) ) ;
#44445 = ORIENTED_EDGE ( 'NONE', *, *, #29800, .T. ) ;
#44446 = CARTESIAN_POINT ( 'NONE',  ( -17.79909385541294142, -8.105421454601382081, 49.25000573077622334 ) ) ;
#44447 = ORIENTED_EDGE ( 'NONE', *, *, #27935, .F. ) ;
#44448 = EDGE_LOOP ( 'NONE', ( #24636, #5276, #11033, #39138, #34319 ) ) ;
#44449 = ORIENTED_EDGE ( 'NONE', *, *, #35898, .F. ) ;
#44450 = CARTESIAN_POINT ( 'NONE',  ( -19.93659385650551741, -6.915538690918074494, 49.31353937987644542 ) ) ;
#44451 = CARTESIAN_POINT ( 'NONE',  ( -18.78945352633789057, -7.485380791038083181, 70.57056797142773519 ) ) ;
#44452 = CARTESIAN_POINT ( 'NONE',  ( -15.93209805084403641, -7.970058305397211385, 63.77896932425708343 ) ) ;
#44453 = CARTESIAN_POINT ( 'NONE',  ( -22.63668070846305724, -10.06225679001389040, 70.30618742561198076 ) ) ;
#44454 = ORIENTED_EDGE ( 'NONE', *, *, #26599, .F. ) ;
#44455 = ORIENTED_EDGE ( 'NONE', *, *, #40850, .F. ) ;
#44456 = CARTESIAN_POINT ( 'NONE',  ( -13.61159385650551457, -6.922745924619793101, 51.69366785382590024 ) ) ;
#44457 = EDGE_CURVE ( 'NONE', #45033, #42114, #40520, .T. ) ;
#44458 = VECTOR ( 'NONE', #24532, 1000.000000000000114 ) ;
#44459 = CARTESIAN_POINT ( 'NONE',  ( -21.75868347184070473, -16.62218431696164345, 49.52966884056655772 ) ) ;
#44460 = CARTESIAN_POINT ( 'NONE',  ( -20.24909385650551386, -8.104110260919579645, 48.81699501597546487 ) ) ;
#44461 = EDGE_CURVE ( 'NONE', #2275, #31856, #6505, .T. ) ;
#44463 = ORIENTED_EDGE ( 'NONE', *, *, #6592, .T. ) ;
#44462 = EDGE_CURVE ( 'NONE', #19538, #1406, #25335, .T. ) ;
#44464 = CARTESIAN_POINT ( 'NONE',  ( -18.50517187854146783, -19.38160480531894336, 52.02966884056656482 ) ) ;
#44465 = EDGE_CURVE ( 'NONE', #16407, #73, #3093, .T. ) ;
#44466 = CARTESIAN_POINT ( 'NONE',  ( -22.21932263989193856, -19.98213852671348434, 69.26597955412674423 ) ) ;
#44467 = EDGE_CURVE ( 'NONE', #14528, #19458, #46455, .T. ) ;
#44468 = CARTESIAN_POINT ( 'NONE',  ( -23.59167324040609870, -11.49507535768466227, 70.00283877229584562 ) ) ;
#44469 = ORIENTED_EDGE ( 'NONE', *, *, #14129, .F. ) ;
#44470 = CARTESIAN_POINT ( 'NONE',  ( -18.92409385541305511, -15.80920654474410725, 47.99999999999997868 ) ) ;
#44471 = EDGE_LOOP ( 'NONE', ( #30801, #22318, #11740, #3902, #4883 ) ) ;
#44472 = CARTESIAN_POINT ( 'NONE',  ( -19.43034385541290732, -6.857644439847486950, 49.98602051094174215 ) ) ;
#44473 = DIRECTION ( 'NONE',  ( 0.3506977235573930929, -0.2775087506578172158, 0.8944271909999157444 ) ) ;
#44474 = CARTESIAN_POINT ( 'NONE',  ( -10.13751350317288669, -13.25697809452625009, 74.93463578866538910 ) ) ;
#44475 = CARTESIAN_POINT ( 'NONE',  ( -21.59170415179237423, -20.98450529054885649, 72.71720556543249359 ) ) ;
#44476 = EDGE_CURVE ( 'NONE', #12076, #21448, #44710, .T. ) ;
#44477 = ORIENTED_EDGE ( 'NONE', *, *, #9661, .T. ) ;
#44478 = CARTESIAN_POINT ( 'NONE',  ( -10.66137368835686416, -12.80659570974005668, 60.68364890423993785 ) ) ;
#44479 = CARTESIAN_POINT ( 'NONE',  ( -15.33343222186064914, -21.95989685909981404, 72.23913770967520520 ) ) ;
#44480 = B_SPLINE_CURVE_WITH_KNOTS ( 'NONE', 3,
 ( #32602, #37003, #10926, #40960, #3290, #18289, #13859, #40245, #33296, #6511 ),
 .UNSPECIFIED., .F., .F.,
 ( 4, 2, 2, 2, 4 ),
 ( 0.6272669072877791185, 0.7522669073073000590, 0.8772669073268208884, 1.002266907346341718, 1.127266907365862769 ),
 .UNSPECIFIED. ) ;
#44481 = CARTESIAN_POINT ( 'NONE',  ( -19.42260780150576949, -7.632255095345715112, 60.06118752816730222 ) ) ;
#44482 = CARTESIAN_POINT ( 'NONE',  ( -23.80321479583337307, -17.81075880182941873, 59.30378417737343710 ) ) ;
#44483 = ORIENTED_EDGE ( 'NONE', *, *, #40281, .T. ) ;
#44484 = CARTESIAN_POINT ( 'NONE',  ( -10.55151208239364635, -17.68521041179895548, 68.28217381303441869 ) ) ;
#44485 = CARTESIAN_POINT ( 'NONE',  ( -21.39967327233876304, -20.63170314183283693, 72.80974286114339122 ) ) ;
#44486 = CARTESIAN_POINT ( 'NONE',  ( -9.995738443926455830, -14.24059931954510816, 64.50308448303212572 ) ) ;
#44487 = ORIENTED_EDGE ( 'NONE', *, *, #29042, .F. ) ;
#44488 = AXIS2_PLACEMENT_3D ( 'NONE', #21731, #48079, #37456 ) ;
#44489 = FACE_BOUND ( 'NONE', #13190, .T. ) ;
#44490 = ORIENTED_EDGE ( 'NONE', *, *, #12413, .F. ) ;
#44491 = CARTESIAN_POINT ( 'NONE',  ( -18.24929096724884658, -21.81104555038653103, 68.82986815895560540 ) ) ;
#44492 = CARTESIAN_POINT ( 'NONE',  ( -50.42409385541304800, -25.10920654474410441, 79.99999999999998579 ) ) ;
#44493 = CARTESIAN_POINT ( 'NONE',  ( -24.42122182511307571, -14.60447249519721069, 62.71296493455815124 ) ) ;
#44494 = CARTESIAN_POINT ( 'NONE',  ( -10.02995815481606634, -13.89786978184575794, 57.63320425522585566 ) ) ;
#44495 = ORIENTED_EDGE ( 'NONE', *, *, #23751, .F. ) ;
#44496 = CARTESIAN_POINT ( 'NONE',  ( -23.83080496556880945, -17.75212211224490133, 59.28906343887996400 ) ) ;
#44497 = EDGE_LOOP ( 'NONE', ( #17071, #31613, #11855, #25045 ) ) ;
#44498 = CARTESIAN_POINT ( 'NONE',  ( -14.80966956416942004, -8.261851763560979833, 60.31996279529170835 ) ) ;
#44499 = CARTESIAN_POINT ( 'NONE',  ( -45.37196614242555626, -14.20920654474410760, 70.13000000000000966 ) ) ;
#44500 = VERTEX_POINT ( 'NONE', #45453 ) ;
#44501 = CARTESIAN_POINT ( 'NONE',  ( -11.21311628236200875, -18.92344944615173929, 64.85368745296808868 ) ) ;
#44502 = PLANE ( 'NONE',  #1515 ) ;
#44503 = ORIENTED_EDGE ( 'NONE', *, *, #34420, .F. ) ;
#44504 = ORIENTED_EDGE ( 'NONE', *, *, #47532, .T. ) ;
#44505 = DIRECTION ( 'NONE',  ( 1.000000000000000000, 0.000000000000000000, 1.927470528863119295E-16 ) ) ;
#44506 = DIRECTION ( 'NONE',  ( 0.1261685609230673022, 0.9920088176193797569, 5.058037262945178882E-08 ) ) ;
#44507 = CARTESIAN_POINT ( 'NONE',  ( -23.46741973463711872, -19.16603908095663655, 62.53902270128352825 ) ) ;
#44508 = CARTESIAN_POINT ( 'NONE',  ( -16.52316554273587101, -21.80170452179945073, 65.24036514508233608 ) ) ;
#44509 = EDGE_CURVE ( 'NONE', #18743, #13624, #43148, .T. ) ;
#44510 = CARTESIAN_POINT ( 'NONE',  ( -12.31054139703831041, -19.59141238940855700, 61.62508423592262119 ) ) ;
#44511 = CARTESIAN_POINT ( 'NONE',  ( -13.83484324388145481, -17.82260368047347043, 52.02966884056656482 ) ) ;
#44512 = CARTESIAN_POINT ( 'NONE',  ( -13.27409385759798965, -6.859212275519751323, 50.50378509014259265 ) ) ;
#44513 = VERTEX_POINT ( 'NONE', #16783 ) ;
#44514 = ORIENTED_EDGE ( 'NONE', *, *, #1090, .T. ) ;
#44515 = EDGE_CURVE ( 'NONE', #3477, #48343, #7115, .T. ) ;
#44516 = CARTESIAN_POINT ( 'NONE',  ( -10.18401502636761968, -13.05277926903019470, 71.32333192088977114 ) ) ;
#44517 = DIRECTION ( 'NONE',  ( -0.9687793358424819923, 0.2479245821708680464, 0.000000000000000000 ) ) ;
#44518 = DIRECTION ( 'NONE',  ( 0.9243256318339804212, -0.3816046728418208134, 8.614662760012533852E-09 ) ) ;
#44519 = CARTESIAN_POINT ( 'NONE',  ( -23.00454255336054743, -10.50046069577333441, 59.88731295783226471 ) ) ;
#44520 = ORIENTED_EDGE ( 'NONE', *, *, #35624, .F. ) ;
#44521 = CARTESIAN_POINT ( 'NONE',  ( -17.68659385650551741, -9.302874398569244363, 51.68646062012417985 ) ) ;
#44522 = CIRCLE ( 'NONE', #485, 5.249999999999998224 ) ;
#44523 = EDGE_LOOP ( 'NONE', ( #44432, #29436, #26433, #20458 ) ) ;
#44524 = DIRECTION ( 'NONE',  ( -0.2479245821708678799, -0.9687793358424819923, -2.626836608253746575E-18 ) ) ;
#44525 = CARTESIAN_POINT ( 'NONE',  ( -17.82409385541305724, -14.80920654474411080, 47.99999999999997868 ) ) ;
#44526 = ADVANCED_FACE ( 'NONE', ( #9422 ), #19334, .T. ) ;
#44527 = CARTESIAN_POINT ( 'NONE',  ( -15.55648817577099585, -8.010769314271311003, 74.09457776258329886 ) ) ;
#44528 = EDGE_CURVE ( 'NONE', #45590, #13240, #9179, .T. ) ;
#44529 = ORIENTED_EDGE ( 'NONE', *, *, #7835, .T. ) ;
#44530 = ADVANCED_FACE ( 'NONE', ( #31579 ), #5959, .T. ) ;
#44531 = CARTESIAN_POINT ( 'NONE',  ( -23.04367355717579713, -10.55211556811382678, 59.90203429191419104 ) ) ;
#44532 = CARTESIAN_POINT ( 'NONE',  ( -21.53458130032788986, -9.143176798465843191, 66.77035947577643071 ) ) ;
#44533 = VERTEX_POINT ( 'NONE', #15627 ) ;
#44534 = DIRECTION ( 'NONE',  ( -3.964551025433374905E-06, -2.747358590626761473E-07, 0.9999999999921033167 ) ) ;
#44535 = EDGE_CURVE ( 'NONE', #10306, #7586, #22363, .T. ) ;
#44536 =( BOUNDED_CURVE ( )  B_SPLINE_CURVE ( 3, ( #26741, #37064, #22550, #3345 ),
 .UNSPECIFIED., .F., .F. ) 
 B_SPLINE_CURVE_WITH_KNOTS ( ( 4, 4 ),
 ( 0.4074455897393638448, 0.5000000000000000000 ),
 .UNSPECIFIED. ) 
 CURVE ( )  GEOMETRIC_REPRESENTATION_ITEM ( )  RATIONAL_B_SPLINE_CURVE ( ( 0.6983129098260937306, 0.7760317562607014219, 0.8765941196520041778, 1.000000000000003997 ) ) 
 REPRESENTATION_ITEM ( '' )  );
#44537 = FACE_OUTER_BOUND ( 'NONE', #15940, .T. ) ;
#44538 = ORIENTED_EDGE ( 'NONE', *, *, #2927, .F. ) ;
#44539 = CARTESIAN_POINT ( 'NONE',  ( -11.15769964539508941, -11.68856008149023218, 71.10477494218005745 ) ) ;
#44540 = ORIENTED_EDGE ( 'NONE', *, *, #17044, .T. ) ;
#44541 = CARTESIAN_POINT ( 'NONE',  ( -43.17409385541305511, -14.90920654474410512, 56.99999999999998579 ) ) ;
#44542 = VERTEX_POINT ( 'NONE', #27879 ) ;
#44543 = DIRECTION ( 'NONE',  ( 1.000000000000000000, 2.866981220435666553E-17, 0.000000000000000000 ) ) ;
#44544 = CARTESIAN_POINT ( 'NONE',  ( -11.43475638805646710, -10.37850985603223286, 74.54546699258546028 ) ) ;
#44545 = ORIENTED_EDGE ( 'NONE', *, *, #19448, .F. ) ;
#44546 = FACE_OUTER_BOUND ( 'NONE', #23352, .T. ) ;
#44547 = CARTESIAN_POINT ( 'NONE',  ( -19.70639753248355319, -21.90109403227812379, 65.57990909513159750 ) ) ;
#44548 = CARTESIAN_POINT ( 'NONE',  ( -13.43921408130402817, -8.993432070331126127, 60.73950277491898220 ) ) ;
#44549 = ORIENTED_EDGE ( 'NONE', *, *, #28391, .F. ) ;
#44550 = CARTESIAN_POINT ( 'NONE',  ( -19.89102460414330054, -21.83908858431354716, 69.09628976311167037 ) ) ;
#44551 =( BOUNDED_CURVE ( )  B_SPLINE_CURVE ( 3, ( #45669, #23248, #19298, #4772 ),
 .UNSPECIFIED., .F., .F. ) 
 B_SPLINE_CURVE_WITH_KNOTS ( ( 4, 4 ),
 ( 0.9074455897393679527, 1.000000000000000000 ),
 .UNSPECIFIED. ) 
 CURVE ( )  GEOMETRIC_REPRESENTATION_ITEM ( )  RATIONAL_B_SPLINE_CURVE ( ( 0.6983129098260973944, 0.7760317562607019770, 0.8765941196520028456, 1.000000000000000000 ) ) 
 REPRESENTATION_ITEM ( '' )  );
#44552 = CIRCLE ( 'NONE', #33471, 4.686499999999998778 ) ;
#44553 = CARTESIAN_POINT ( 'NONE',  ( -18.59487950719992000, -7.451777622494494047, 73.99064398808116039 ) ) ;
#44554 = CARTESIAN_POINT ( 'NONE',  ( 18.46573386768564973, 1.644457370994424572, 49.30478444670940519 ) ) ;
#44555 = ORIENTED_EDGE ( 'NONE', *, *, #15590, .T. ) ;
#44556 = VERTEX_POINT ( 'NONE', #5236 ) ;
#44557 = CARTESIAN_POINT ( 'NONE',  ( -22.79960313759534074, -9.650943445293346912, 73.66656413195866548 ) ) ;
#44558 = FACE_OUTER_BOUND ( 'NONE', #31597, .T. ) ;
#44559 = CARTESIAN_POINT ( 'NONE',  ( -17.78823904182716120, -7.818684512505932993, 60.38060768393231825 ) ) ;
#44560 = CARTESIAN_POINT ( 'NONE',  ( -16.59284385759799108, -8.630756214087126565, 51.74842643355248129 ) ) ;
#44561 = CARTESIAN_POINT ( 'NONE',  ( -10.78898398081525301, -17.19290454168847404, 61.44271037915215317 ) ) ;
#44562 = EDGE_CURVE ( 'NONE', #25852, #36933, #47054, .T. ) ;
#44563 = FACE_OUTER_BOUND ( 'NONE', #33392, .T. ) ;
#44564 = DIRECTION ( 'NONE',  ( 0.09332174201254204993, 0.9956360040033428449, 0.000000000000000000 ) ) ;
#44565 = CYLINDRICAL_SURFACE ( 'NONE', #47321, 2.000000000000003109 ) ;
#44566 = ORIENTED_EDGE ( 'NONE', *, *, #25240, .F. ) ;
#44567 = CARTESIAN_POINT ( 'NONE',  ( -20.88289085685542545, -8.210692395643533814, 59.88479313977884289 ) ) ;
#44568 = DIRECTION ( 'NONE',  ( 0.000000000000000000, 0.000000000000000000, 1.000000000000000000 ) ) ;
#44569 = CARTESIAN_POINT ( 'NONE',  ( -24.47304815678895196, -15.04811744431364140, 59.65788834854969735 ) ) ;
#44570 = CARTESIAN_POINT ( 'NONE',  ( -23.74619254753875808, -11.68933987248222550, 63.10218278636759237 ) ) ;
#44571 = ORIENTED_EDGE ( 'NONE', *, *, #22040, .F. ) ;
#44572 = ORIENTED_EDGE ( 'NONE', *, *, #46365, .F. ) ;
#44573 = CARTESIAN_POINT ( 'NONE',  ( -17.72634082312590920, -21.85272461445201486, 58.40553378267873796 ) ) ;
#44574 =( NAMED_UNIT ( * ) PLANE_ANGLE_UNIT ( ) SI_UNIT ( $, .RADIAN. ) );
#44575 = EDGE_CURVE ( 'NONE', #6612, #47792, #20250, .T. ) ;
#44576 = CARTESIAN_POINT ( 'NONE',  ( -10.72552546848295485, -12.61109793159036485, 61.09853568372136579 ) ) ;
#44577 = DIRECTION ( 'NONE',  ( -1.371991812172399310E-08, 1.272593380608347342E-06, -0.9999999999991900923 ) ) ;
#44578 = EDGE_CURVE ( 'NONE', #10249, #38900, #26591, .T. ) ;
#44579 = ORIENTED_EDGE ( 'NONE', *, *, #5790, .T. ) ;
#44580 = CARTESIAN_POINT ( 'NONE',  ( -24.46903964301072421, -12.38562919627177727, 73.38079058079814843 ) ) ;
#44581 = AXIS2_PLACEMENT_3D ( 'NONE', #46975, #13220, #42081 ) ;
#44582 = AXIS2_PLACEMENT_3D ( 'NONE', #2561, #32819, #44192 ) ;
#44583 = EDGE_CURVE ( 'NONE', #35456, #46448, #15375, .T. ) ;
#44584 = CARTESIAN_POINT ( 'NONE',  ( -12.63291411399994146, -9.103221862242449447, 74.50578369661835154 ) ) ;
#44585 = ORIENTED_EDGE ( 'NONE', *, *, #46463, .T. ) ;
#44586 = CARTESIAN_POINT ( 'NONE',  ( -22.38400238879419391, -20.36826089713532895, 62.41934470639706944 ) ) ;
#44587 = EDGE_CURVE ( 'NONE', #20159, #34400, #46236, .T. ) ;
#44588 = AXIS2_PLACEMENT_3D ( 'NONE', #2076, #39267, #1337 ) ;
#44589 = LINE ( 'NONE', #37164, #15486 ) ;
#44590 = CARTESIAN_POINT ( 'NONE',  ( -24.77697371742066679, -16.00871596996390167, 66.10678971410503380 ) ) ;
#44591 = VERTEX_POINT ( 'NONE', #26739 ) ;
#44592 = LINE ( 'NONE', #21929, #7895 ) ;
#44593 = VERTEX_POINT ( 'NONE', #46840 ) ;
#44594 = CARTESIAN_POINT ( 'NONE',  ( -23.81233663663554978, -10.97605585942814344, 73.46219060175555171 ) ) ;
#44595 = CYLINDRICAL_SURFACE ( 'NONE', #42296, 0.1500000000000022704 ) ;
#44596 = ORIENTED_EDGE ( 'NONE', *, *, #31850, .F. ) ;
#44597 = CARTESIAN_POINT ( 'NONE',  ( -21.36284794767689377, -21.13297080501056513, 69.16954792666395235 ) ) ;
#44598 = CARTESIAN_POINT ( 'NONE',  ( -10.31379496977684340, -12.58270390103710668, 64.45491433821949556 ) ) ;
#44599 = B_SPLINE_CURVE_WITH_KNOTS ( 'NONE', 1,
 ( #28381, #35264 ),
 .UNSPECIFIED., .F., .F.,
 ( 2, 2 ),
 ( 0.000000000000000000, 1.000000000000000000 ),
 .UNSPECIFIED. ) ;
#44600 = CARTESIAN_POINT ( 'NONE',  ( -22.55534385650551954, -7.417179338643134834, 52.18511593390279302 ) ) ;
#44601 = CARTESIAN_POINT ( 'NONE',  ( -14.37840813110883254, -8.506458304712115392, 67.27477558708663707 ) ) ;
#44602 = EDGE_CURVE ( 'NONE', #10578, #11221, #41758, .T. ) ;
#44603 = CARTESIAN_POINT ( 'NONE',  ( -10.56879219357104915, -13.14797678187891528, 74.97817813415294097 ) ) ;
#44604 = CARTESIAN_POINT ( 'NONE',  ( -48.17409385541305511, -15.81020654474410847, 61.49999999999999289 ) ) ;
#44605 = DIRECTION ( 'NONE',  ( 1.487365700889503844E-06, -6.376425446390537491E-07, -0.9999999999986906030 ) ) ;
#44606 = B_SPLINE_CURVE_WITH_KNOTS ( 'NONE', 1,
 ( #17139, #32433 ),
 .UNSPECIFIED., .F., .F.,
 ( 2, 2 ),
 ( 0.000000000000000000, 1.000000000000000000 ),
 .UNSPECIFIED. ) ;
#44607 = ORIENTED_EDGE ( 'NONE', *, *, #41030, .F. ) ;
#44608 = CARTESIAN_POINT ( 'NONE',  ( -46.38423044223897307, -13.72754205882879042, 70.13000000000000966 ) ) ;
#44609 = ADVANCED_FACE ( 'NONE', ( #36455 ), #1772, .T. ) ;
#44610 = DIRECTION ( 'NONE',  ( -0.9410372374137780938, -0.3383029970317210644, -1.029646047569396398E-09 ) ) ;
#44611 = DIRECTION ( 'NONE',  ( -0.9687793358424822143, 0.2479245821708672415, 0.000000000000000000 ) ) ;
#44612 = CARTESIAN_POINT ( 'NONE',  ( -24.83132749654373939, -14.01209333255521727, 73.27271506205273965 ) ) ;
#44613 = CARTESIAN_POINT ( 'NONE',  ( -16.09495291808068274, -22.13976250616876840, 58.54231521589509413 ) ) ;
#44614 = CARTESIAN_POINT ( 'NONE',  ( -22.79960237261627398, -9.650942640399760464, 73.66656521964461035 ) ) ;
#44615 = ORIENTED_EDGE ( 'NONE', *, *, #44401, .T. ) ;
#44616 = ORIENTED_EDGE ( 'NONE', *, *, #41302, .T. ) ;
#44617 = LINE ( 'NONE', #29842, #20420 ) ;
#44618 = CARTESIAN_POINT ( 'NONE',  ( -9.974839262372155346, -14.70319952471188074, 71.52771478739579436 ) ) ;
#44619 = ORIENTED_EDGE ( 'NONE', *, *, #38739, .T. ) ;
#44621 = CARTESIAN_POINT ( 'NONE',  ( -11.77456497187086093, -18.94253032688613914, 71.98685932465902226 ) ) ;
#44620 = CARTESIAN_POINT ( 'NONE',  ( -16.31151605585062825, -19.37404237808139484, 52.02966884056656482 ) ) ;
#44622 = CARTESIAN_POINT ( 'NONE',  ( -11.36794959886231915, -18.31963617796164812, 57.80714594517343841 ) ) ;
#44623 = CARTESIAN_POINT ( 'NONE',  ( -11.59701759869595072, -18.68823990753973163, 65.04707024129098158 ) ) ;
#44624 = CARTESIAN_POINT ( 'NONE',  ( -12.10487669921564446, -20.02548830339394925, 61.44032727821130635 ) ) ;
#44625 = CARTESIAN_POINT ( 'NONE',  ( -11.20995753719673438, -18.14677381299707548, 58.10714798773844336 ) ) ;
#44626 = CARTESIAN_POINT ( 'NONE',  ( -24.82596573341765733, -13.96226896445660515, 73.28304862000281616 ) ) ;
#44627 = VECTOR ( 'NONE', #28343, 1000.000000000000000 ) ;
#44628 = DIRECTION ( 'NONE',  ( 5.215802034766747424E-06, -6.671378398269898551E-06, -0.9999999999641441262 ) ) ;
#44629 = AXIS2_PLACEMENT_3D ( 'NONE', #42895, #24183, #38708 ) ;
#44630 = CARTESIAN_POINT ( 'NONE',  ( -42.29394679658953038, -14.90920654474417972, 64.04117647058822627 ) ) ;
#44631 = ORIENTED_EDGE ( 'NONE', *, *, #37906, .T. ) ;
#44632 = CARTESIAN_POINT ( 'NONE',  ( -20.37299714182665866, -8.405577154986387356, 67.08104082189564110 ) ) ;
#44633 = CARTESIAN_POINT ( 'NONE',  ( -12.77466994470616690, -9.357823239324572384, 50.04128243944182231 ) ) ;
#44634 = CARTESIAN_POINT ( 'NONE',  ( 18.51825960693461681, 3.132802701810887935, 50.36638420821972062 ) ) ;
#44635 = VECTOR ( 'NONE', #24737, 1000.000000000000114 ) ;
#44636 = CARTESIAN_POINT ( 'NONE',  ( -11.06319317263454849, -11.76086512588999256, 67.82684465229463910 ) ) ;
#44637 = DIRECTION ( 'NONE',  ( -1.504942875245327186E-06, 3.061075853171912725E-06, -0.9999999999941825424 ) ) ;
#44638 = CARTESIAN_POINT ( 'NONE',  ( -14.60635853056651001, -21.70587488938233278, 58.20971981907628390 ) ) ;
#44639 = FACE_OUTER_BOUND ( 'NONE', #46113, .T. ) ;
#44640 = ORIENTED_EDGE ( 'NONE', *, *, #11876, .T. ) ;
#44641 = ORIENTED_EDGE ( 'NONE', *, *, #33378, .F. ) ;
#44642 = B_SPLINE_CURVE_WITH_KNOTS ( 'NONE', 3,
 ( #41178, #15056, #48312, #18267, #4918, #48560, #67, #971, #7218, #30114 ),
 .UNSPECIFIED., .F., .F.,
 ( 4, 2, 2, 2, 4 ),
 ( 0.000000000000000000, 0.2500000000000000000, 0.5000000000000000000, 0.7500000000000000000, 1.000000000000000000 ),
 .UNSPECIFIED. ) ;
#44643 = CARTESIAN_POINT ( 'NONE',  ( -14.03034385541304374, -6.857644439848014528, 49.98602051094140819 ) ) ;
#44644 = ORIENTED_EDGE ( 'NONE', *, *, #47253, .F. ) ;
#44645 = FACE_OUTER_BOUND ( 'NONE', #4810, .T. ) ;
#44646 = CARTESIAN_POINT ( 'NONE',  ( -24.72409385541305582, -14.80920654474416764, 63.03529411764704804 ) ) ;
#44647 = EDGE_CURVE ( 'NONE', #3049, #48304, #21468, .T. ) ;
#44648 = CARTESIAN_POINT ( 'NONE',  ( -18.34560609025200861, -9.386954687716537293, 54.07175714974878389 ) ) ;
#44649 = CARTESIAN_POINT ( 'NONE',  ( -16.16221656818315466, -22.15164012088281709, 58.32939616168999208 ) ) ;
#44650 = ORIENTED_EDGE ( 'NONE', *, *, #48088, .T. ) ;
#44651 = EDGE_CURVE ( 'NONE', #828, #40875, #30122, .T. ) ;
#44652 = CARTESIAN_POINT ( 'NONE',  ( -24.37710591498809265, -15.61986392179586147, 73.00303784453015510 ) ) ;
#44653 = VECTOR ( 'NONE', #48388, 1000.000000000000000 ) ;
#44654 = CARTESIAN_POINT ( 'NONE',  ( -12.45873566688477929, -9.804017486950373339, 57.10407583662104258 ) ) ;
#44655 = ORIENTED_EDGE ( 'NONE', *, *, #35548, .T. ) ;
#44656 = CARTESIAN_POINT ( 'NONE',  ( -22.31965859069846658, -20.42511761535959636, 62.37405793546869148 ) ) ;
#44657 = DIRECTION ( 'NONE',  ( -0.8356905716187447153, 0.5492005722024784209, 7.728900804118605128E-08 ) ) ;
#44658 = AXIS2_PLACEMENT_3D ( 'NONE', #11077, #8358, #45310 ) ;
#44659 = VECTOR ( 'NONE', #44981, 1000.000000000000000 ) ;
#44660 = ORIENTED_EDGE ( 'NONE', *, *, #32280, .T. ) ;
#44661 = CARTESIAN_POINT ( 'NONE',  ( -19.57699507595987143, -21.94144279212693860, 62.17998934563075153 ) ) ;
#44662 = PLANE ( 'NONE',  #34619 ) ;
#44663 = CARTESIAN_POINT ( 'NONE',  ( -13.06813783877040791, -9.265530354883376063, 67.66470656304637998 ) ) ;
#44664 = VERTEX_POINT ( 'NONE', #47797 ) ;
#44665 = DIRECTION ( 'NONE',  ( -3.071710424422018668E-17, 6.404604876783312462E-16, 1.000000000000000000 ) ) ;
#44666 = DIRECTION ( 'NONE',  ( 0.000000000000000000, -0.9999954153791273948, -0.003028072113819838245 ) ) ;
#44667 = VECTOR ( 'NONE', #37074, 1000.000000000000114 ) ;
#44668 = ADVANCED_FACE ( 'NONE', ( #20978 ), #28233, .T. ) ;
#44669 = CARTESIAN_POINT ( 'NONE',  ( -15.03805483313293756, -21.39046390026760847, 65.38980090007645174 ) ) ;
#44670 = CARTESIAN_POINT ( 'NONE',  ( -10.57818832626110250, -17.74982580657420428, 68.21066696669559803 ) ) ;
#44671 = ORIENTED_EDGE ( 'NONE', *, *, #36790, .F. ) ;
#44672 = CARTESIAN_POINT ( 'NONE',  ( -24.66733291767277692, -16.55538881886969804, 59.30987817879385915 ) ) ;
#44673 = DIRECTION ( 'NONE',  ( -0.1240347345892086062, 1.145860353393066553E-16, -0.9922778767136676281 ) ) ;
#44674 = VECTOR ( 'NONE', #11312, 1000.000000000000000 ) ;
#44675 = CARTESIAN_POINT ( 'NONE',  ( -15.40901097238366546, -21.51335240779075875, 72.32958917352875972 ) ) ;
#44676 = EDGE_CURVE ( 'NONE', #26011, #17474, #24118, .T. ) ;
#44677 = CARTESIAN_POINT ( 'NONE',  ( -18.05298600948144028, -21.78095894789524678, 61.94824011654481666 ) ) ;
#44678 = EDGE_CURVE ( 'NONE', #545, #40496, #6798, .T. ) ;
#44679 = EDGE_CURVE ( 'NONE', #24975, #25942, #11846, .T. ) ;
#44680 = CARTESIAN_POINT ( 'NONE',  ( -11.89466307818281798, -10.43082414681992276, 74.85374085024349711 ) ) ;
#44681 = EDGE_CURVE ( 'NONE', #12464, #3912, #36938, .T. ) ;
#44682 = ORIENTED_EDGE ( 'NONE', *, *, #18299, .T. ) ;
#44683 = CARTESIAN_POINT ( 'NONE',  ( -17.70776835051902864, -22.25388969026799657, 58.52057945155585372 ) ) ;
#44684 = CARTESIAN_POINT ( 'NONE',  ( -14.66630222544868900, -8.320656262913127321, 63.80450889863892172 ) ) ;
#44685 = ORIENTED_EDGE ( 'NONE', *, *, #44509, .F. ) ;
#44686 = FACE_OUTER_BOUND ( 'NONE', #31177, .T. ) ;
#44687 = CARTESIAN_POINT ( 'NONE',  ( -22.59024966566153125, -10.08387632041895188, 73.55331295946989201 ) ) ;
#44688 = CARTESIAN_POINT ( 'NONE',  ( -17.19811928533322387, -9.313850733363548073, 53.49899999999994549 ) ) ;
#44689 =( BOUNDED_SURFACE ( )  B_SPLINE_SURFACE ( 3, 1, ( 
 ( #301, #19000 ),
 ( #15773, #30345 ),
 ( #45842, #12098 ),
 ( #27110, #42139 ),
 ( #38424, #4713 ),
 ( #1017, #47037 ),
 ( #46573, #38679 ) ),
 .UNSPECIFIED., .T., .F., .F. ) 
 B_SPLINE_SURFACE_WITH_KNOTS ( ( 4, 3, 4 ),
 ( 2, 2 ),
 ( 0.000000000000000000, 0.5000000000000000000, 1.000000000000000000 ),
 ( 0.000000000000000000, 1.000000000000000000 ),
 .UNSPECIFIED. ) 
 GEOMETRIC_REPRESENTATION_ITEM ( )  RATIONAL_B_SPLINE_SURFACE ( (
 ( 1.000000000000000000, 1.000000000000000000),
 ( 0.3333333333333335369, 0.3333333333333330373),
 ( 0.3333333333333335369, 0.3333333333333330373),
 ( 1.000000000000000000, 1.000000000000000000),
 ( 0.3333333333333333703, 0.3333333333333333703),
 ( 0.3333333333333333703, 0.3333333333333333703),
 ( 1.000000000000000000, 1.000000000000000000) ) ) 
 REPRESENTATION_ITEM ( '' )  SURFACE ( )  );
#44690 = ORIENTED_EDGE ( 'NONE', *, *, #31833, .T. ) ;
#44691 = CARTESIAN_POINT ( 'NONE',  ( -10.05751352497363271, -15.92131473292516119, 64.70045725156860783 ) ) ;
#44692 = CARTESIAN_POINT ( 'NONE',  ( -18.40644494809068377, -22.19428016187509911, 68.93701928270169788 ) ) ;
#44693 = ORIENTED_EDGE ( 'NONE', *, *, #47895, .F. ) ;
#44694 = VERTEX_POINT ( 'NONE', #17268 ) ;
#44695 = CARTESIAN_POINT ( 'NONE',  ( -16.28034385650551741, -6.424090610841176385, 49.80797279389977916 ) ) ;
#44696 = AXIS2_PLACEMENT_3D ( 'NONE', #46670, #43957, #2328 ) ;
#44697 = CARTESIAN_POINT ( 'NONE',  ( -18.83586040784625126, -7.494106175837369044, 70.48572642001049360 ) ) ;
#44698 = DIRECTION ( 'NONE',  ( -0.4439273849576848563, -0.8960627639203804229, 9.143653603063735118E-17 ) ) ;
#44699 = CARTESIAN_POINT ( 'NONE',  ( -14.03247011961845203, -8.175865378139491213, 70.85144881067481037 ) ) ;
#44700 = DIRECTION ( 'NONE',  ( 4.556087729312554466E-06, -5.696494005668992306E-06, 0.9999999999733959477 ) ) ;
#44701 =( BOUNDED_CURVE ( )  B_SPLINE_CURVE ( 3, ( #25585, #11063, #48230, #19858 ),
 .UNSPECIFIED., .F., .F. ) 
 B_SPLINE_CURVE_WITH_KNOTS ( ( 4, 4 ),
 ( 0.9074455897393648440, 1.000000000000000000 ),
 .UNSPECIFIED. ) 
 CURVE ( )  GEOMETRIC_REPRESENTATION_ITEM ( )  RATIONAL_B_SPLINE_CURVE ( ( 0.6983129098261178225, 0.7760317562607195185, 0.8765941196520136147, 1.000000000000000000 ) ) 
 REPRESENTATION_ITEM ( '' )  );
#44702 = AXIS2_PLACEMENT_3D ( 'NONE', #939, #24321, #23596 ) ;
#44703 = ORIENTED_EDGE ( 'NONE', *, *, #11375, .F. ) ;
#44704 = EDGE_LOOP ( 'NONE', ( #10122, #391, #3910, #19017, #8838, #9258, #40058, #27731, #9935, #36092, #45058 ) ) ;
#44705 = CARTESIAN_POINT ( 'NONE',  ( -15.24284385650551776, -8.811426318492348031, 52.18089403414752070 ) ) ;
#44706 = EDGE_CURVE ( 'NONE', #46361, #25757, #39989, .T. ) ;
#44707 = CARTESIAN_POINT ( 'NONE',  ( -17.42409385541299471, -14.80920654474434883, 62.02966884056656482 ) ) ;
#44708 = CARTESIAN_POINT ( 'NONE',  ( -11.33665496402021411, -18.36534999539612301, 58.10714572920461052 ) ) ;
#44709 = CARTESIAN_POINT ( 'NONE',  ( -14.96159385650551776, -9.295667164867525756, 49.30633214617472504 ) ) ;
#44710 = B_SPLINE_CURVE_WITH_KNOTS ( 'NONE', 3,
 ( #41502, #7792, #40767, #22063, #7051, #42908, #20503, #13085, #28120, #46612 ),
 .UNSPECIFIED., .F., .F.,
 ( 4, 2, 2, 2, 4 ),
 ( 0.000000000000000000, 0.2500000000000000000, 0.5000000000000000000, 0.7500000000000000000, 1.000000000000000000 ),
 .UNSPECIFIED. ) ;
#44711 =( BOUNDED_CURVE ( )  B_SPLINE_CURVE ( 2, ( #31489, #43314, #12776, #24603, #16205, #24107, #27792, #39601, #9094 ),
 .UNSPECIFIED., .F., .F. ) 
 B_SPLINE_CURVE_WITH_KNOTS ( ( 3, 2, 2, 2, 3 ),
 ( 0.003933667230126343395, 0.004917278694326980212, 0.005900890158527617030, 0.006884501622728254715, 0.007868113086928890665 ),
 .UNSPECIFIED. ) 
 CURVE ( )  GEOMETRIC_REPRESENTATION_ITEM ( )  RATIONAL_B_SPLINE_CURVE ( ( 1.000000000000037526, 0.9238795325112491019, 1.000000000000000000, 0.9238795325112867385, 1.000000000000000000, 0.9238795325112867385, 1.000000000000000000, 0.9238795325090227717, 1.000000000002263967 ) ) 
 REPRESENTATION_ITEM ( '' )  );
#44712 = ORIENTED_EDGE ( 'NONE', *, *, #38457, .T. ) ;
#44713 = DIRECTION ( 'NONE',  ( 0.5088156898428700670, 0.8608754809899750171, 5.922709712265242817E-08 ) ) ;
#44714 = ADVANCED_FACE ( 'NONE', ( #41883 ), #26615, .T. ) ;
#44715 = CARTESIAN_POINT ( 'NONE',  ( -23.83043768205027035, -11.86620487761972420, 59.63235732590894855 ) ) ;
#44716 = CARTESIAN_POINT ( 'NONE',  ( -23.58371748462962714, -11.48100147700675855, 70.12040655271316325 ) ) ;
#44717 = ORIENTED_EDGE ( 'NONE', *, *, #23675, .T. ) ;
#44718 = CARTESIAN_POINT ( 'NONE',  ( -23.05949083151958590, -18.96177719399141282, 62.35406924025621578 ) ) ;
#44719 = ORIENTED_EDGE ( 'NONE', *, *, #16093, .F. ) ;
#44720 = CYLINDRICAL_SURFACE ( 'NONE', #47300, 5.249999999999998224 ) ;
#44721 = CARTESIAN_POINT ( 'NONE',  ( -17.42409385541299471, -14.80920654474434883, 62.02966884056656482 ) ) ;
#44722 = CARTESIAN_POINT ( 'NONE',  ( -10.57818832626110250, -17.74982580657420428, 68.21066696669559803 ) ) ;
#44723 = CARTESIAN_POINT ( 'NONE',  ( -11.38156967460460223, -11.17705904596687105, 60.68445599065120177 ) ) ;
#44724 = ORIENTED_EDGE ( 'NONE', *, *, #15006, .T. ) ;
#44725 = CARTESIAN_POINT ( 'NONE',  ( -18.94833620235381133, -7.977059930319036596, 67.20071832652779165 ) ) ;
#44726 = CARTESIAN_POINT ( 'NONE',  ( -22.77174232103692830, -19.99646445987193388, 72.80547028276266985 ) ) ;
#44727 = MECHANICAL_DESIGN_GEOMETRIC_PRESENTATION_REPRESENTATION (  '', ( #3018 ), #2247 ) ;
#44728 = CYLINDRICAL_SURFACE ( 'NONE', #23513, 0.1500000000000013267 ) ;
#44729 = CARTESIAN_POINT ( 'NONE',  ( -21.34582186320181307, -20.66775149956831115, 72.82446429489806405 ) ) ;
#44730 = EDGE_LOOP ( 'NONE', ( #34158, #42373 ) ) ;
#44731 = CARTESIAN_POINT ( 'NONE',  ( -17.56322643164902431, -15.18422937902243142, 47.99999999999994316 ) ) ;
#44732 = CARTESIAN_POINT ( 'NONE',  ( -17.14371526033637849, -7.364357988229939700, 70.66752758873944629 ) ) ;
#44733 = AXIS2_PLACEMENT_3D ( 'NONE', #15947, #39337, #13211 ) ;
#44735 = CARTESIAN_POINT ( 'NONE',  ( -12.64043014238784046, -19.91972699092798038, 65.09348316439465520 ) ) ;
#44734 = AXIS2_PLACEMENT_3D ( 'NONE', #1291, #2270, #17276 ) ;
#44736 = ORIENTED_EDGE ( 'NONE', *, *, #25568, .T. ) ;
#44737 = FACE_BOUND ( 'NONE', #15690, .T. ) ;
#44738 = VERTEX_POINT ( 'NONE', #11841 ) ;
#44739 = EDGE_CURVE ( 'NONE', #17093, #25305, #9701, .T. ) ;
#44740 = ADVANCED_FACE ( 'NONE', ( #18980 ), #3716, .F. ) ;
#44741 = CARTESIAN_POINT ( 'NONE',  ( -22.09027712961677636, -20.02729522806141915, 62.23439146821721124 ) ) ;
#44742 = FACE_OUTER_BOUND ( 'NONE', #24453, .T. ) ;
#44743 = DIRECTION ( 'NONE',  ( 3.071710424422018668E-17, -6.404604876783312462E-16, -1.000000000000000000 ) ) ;
#44744 = DIRECTION ( 'NONE',  ( 2.866981220435666553E-17, -1.000000000000000000, -1.190614954331866791E-16 ) ) ;
#44745 = VERTEX_POINT ( 'NONE', #44853 ) ;
#44746 = CARTESIAN_POINT ( 'NONE',  ( -18.53202070066404161, -7.846807721809618386, 73.84064401782792686 ) ) ;
#44747 = VECTOR ( 'NONE', #25946, 1000.000000000000000 ) ;
#44748 = VERTEX_POINT ( 'NONE', #15754 ) ;
#44749 = LINE ( 'NONE', #11481, #43140 ) ;
#44750 = CARTESIAN_POINT ( 'NONE',  ( -14.91432061146141663, -8.212540298998538546, 63.93411529719415398 ) ) ;
#44751 = ORIENTED_EDGE ( 'NONE', *, *, #18895, .F. ) ;
#44752 = CARTESIAN_POINT ( 'NONE',  ( -21.65613231742964473, -20.94137680209911423, 72.63791026777079196 ) ) ;
#44753 = EDGE_CURVE ( 'NONE', #11637, #3920, #33985, .T. ) ;
#44754 = ADVANCED_FACE ( 'NONE', ( #30808 ), #30325, .T. ) ;
#44755 = CARTESIAN_POINT ( 'NONE',  ( -10.98359684359402699, -17.55162065409421501, 68.11224428658677255 ) ) ;
#44756 = ORIENTED_EDGE ( 'NONE', *, *, #42686, .F. ) ;
#44757 = ORIENTED_EDGE ( 'NONE', *, *, #10091, .T. ) ;
#44758 = CARTESIAN_POINT ( 'NONE',  ( -22.60969001043771698, -13.98939405582217255, 52.02966884056656482 ) ) ;
#44759 = CARTESIAN_POINT ( 'NONE',  ( -22.23802305151986403, -19.89335697136803205, 69.36344962027256145 ) ) ;
#44760 = CARTESIAN_POINT ( 'NONE',  ( -13.05029276218966672, -20.34859559109395377, 71.96220867596423432 ) ) ;
#44761 = FACE_OUTER_BOUND ( 'NONE', #5286, .T. ) ;
#44762 = B_SPLINE_CURVE_WITH_KNOTS ( 'NONE', 3,
 ( #41840, #48727, #14966, #45060, #26319, #22632, #33943, #15216, #37628, #30277 ),
 .UNSPECIFIED., .F., .F.,
 ( 4, 2, 2, 2, 4 ),
 ( 0.1272669073658116712, 0.2522669073463083000, 0.3772669073268050122, 0.5022669073073016133, 0.6272669072877983254 ),
 .UNSPECIFIED. ) ;
#44763 = DIRECTION ( 'NONE',  ( 3.811252424767960347E-06, 6.838859004561632622E-06, 0.9999999999693520714 ) ) ;
#44764 = CARTESIAN_POINT ( 'NONE',  ( -14.23114467316514897, -8.578028860463618344, 74.31027642345760853 ) ) ;
#44765 = CARTESIAN_POINT ( 'NONE',  ( -22.28538024775887294, -19.92612572838908491, 72.78833238834644703 ) ) ;
#44766 = ORIENTED_EDGE ( 'NONE', *, *, #28770, .F. ) ;
#44767 = ORIENTED_EDGE ( 'NONE', *, *, #5176, .T. ) ;
#44768 = CARTESIAN_POINT ( 'NONE',  ( -12.08372859862091708, -10.28366800835667760, 64.13800404418488199 ) ) ;
#44769 = EDGE_CURVE ( 'NONE', #5353, #33324, #38271, .T. ) ;
#44770 = CARTESIAN_POINT ( 'NONE',  ( -23.12535539932854078, -10.01343808792704237, 66.65686846082743955 ) ) ;
#44771 = CIRCLE ( 'NONE', #40041, 1.999999999999999112 ) ;
#44772 = CARTESIAN_POINT ( 'NONE',  ( -28.42409385541305511, -25.10920654474410441, 47.99999999999997868 ) ) ;
#44773 = CARTESIAN_POINT ( 'NONE',  ( -10.38360249164154325, -14.43747963625415309, 67.87272197508832505 ) ) ;
#44774 = CARTESIAN_POINT ( 'NONE',  ( -14.99706828511980916, -21.85287925006270626, 65.29092110561946072 ) ) ;
#44775 = ORIENTED_EDGE ( 'NONE', *, *, #48198, .F. ) ;
#44776 = CARTESIAN_POINT ( 'NONE',  ( -19.37409385650551741, -9.792211528768504536, 50.49490371617623197 ) ) ;
#44777 = AXIS2_PLACEMENT_3D ( 'NONE', #22695, #26881, #769 ) ;
#44778 = ORIENTED_EDGE ( 'NONE', *, *, #36631, .T. ) ;
#44779 = CARTESIAN_POINT ( 'NONE',  ( -24.35706328060247827, -15.77560928887050373, 69.53307488759497801 ) ) ;
#44780 = CARTESIAN_POINT ( 'NONE',  ( -13.60238447927381777, -8.884931327198675177, 57.11967755504965538 ) ) ;
#44781 = LINE ( 'NONE', #7595, #11867 ) ;
#44782 = AXIS2_PLACEMENT_3D ( 'NONE', #28380, #40181, #5961 ) ;
#44783 = ORIENTED_EDGE ( 'NONE', *, *, #14831, .F. ) ;
#44784 = CARTESIAN_POINT ( 'NONE',  ( -15.87557675045462169, -7.931373007531637320, 67.29007279016111909 ) ) ;
#44785 = DIRECTION ( 'NONE',  ( -1.070267892829395584E-05, -6.715522050485540099E-06, 0.9999999999201771850 ) ) ;
#44786 = EDGE_LOOP ( 'NONE', ( #39987, #21174, #15436, #21694, #20399 ) ) ;
#44787 = CARTESIAN_POINT ( 'NONE',  ( -15.18490717705548398, -21.44146708918249544, 65.12099149998387304 ) ) ;
#44788 = CARTESIAN_POINT ( 'NONE',  ( -10.13086764262007655, -16.32976185473646424, 71.55412051275166618 ) ) ;
#44789 = EDGE_LOOP ( 'NONE', ( #5751, #41976, #16167 ) ) ;
#44790 = DIRECTION ( 'NONE',  ( -3.071710424422018668E-17, 6.404604876783312462E-16, 1.000000000000000000 ) ) ;
#44791 = VERTEX_POINT ( 'NONE', #19222 ) ;
#44792 = CARTESIAN_POINT ( 'NONE',  ( -10.31364510401727053, -17.03300888149450998, 57.80265138661536639 ) ) ;
#44793 = CARTESIAN_POINT ( 'NONE',  ( -17.56717507065399531, -7.360494836047319467, 63.73552460944732445 ) ) ;
#44794 = VERTEX_POINT ( 'NONE', #15501 ) ;
#44795 = ADVANCED_FACE ( 'NONE', ( #26129 ), #29825, .T. ) ;
#44796 = CARTESIAN_POINT ( 'NONE',  ( -45.90212350580859635, -14.19714313411900264, 69.94185769334995939 ) ) ;
#44797 = CARTESIAN_POINT ( 'NONE',  ( -10.44916082259175916, -15.83527127794237188, 64.80771589743309846 ) ) ;
#44798 = VECTOR ( 'NONE', #38952, 1000.000000000000000 ) ;
#44799 = ORIENTED_EDGE ( 'NONE', *, *, #1094, .T. ) ;
#44800 = CARTESIAN_POINT ( 'NONE',  ( -22.67171275331017810, -14.65110561991362381, 50.77966884056655772 ) ) ;
#44801 = DIRECTION ( 'NONE',  ( -0.9294853595766571219, -0.3688590060343552857, 0.000000000000000000 ) ) ;
#44802 = CARTESIAN_POINT ( 'NONE',  ( -23.89200535028185612, -11.11192396016905448, 70.07706043178237110 ) ) ;
#44803 = ORIENTED_EDGE ( 'NONE', *, *, #1578, .T. ) ;
#44804 = B_SPLINE_CURVE_WITH_KNOTS ( 'NONE', 3,
 ( #16164, #15686, #12248, #27270, #1398, #8326, #4877, #19888, #20125, #34891 ),
 .UNSPECIFIED., .F., .F.,
 ( 4, 2, 2, 2, 4 ),
 ( 0.000000000000000000, 0.2500000000000000000, 0.5000000000000000000, 0.7500000000000000000, 1.000000000000000000 ),
 .UNSPECIFIED. ) ;
#44805 = CARTESIAN_POINT ( 'NONE',  ( -23.08487763607990928, -19.01185175973044039, 62.36879011380454330 ) ) ;
#44806 = VECTOR ( 'NONE', #36654, 1000.000000000000114 ) ;
#44807 = EDGE_CURVE ( 'NONE', #11839, #27248, #34403, .T. ) ;
#44808 = CARTESIAN_POINT ( 'NONE',  ( -20.66848101912799862, -8.549761622307149977, 60.12653141481577990 ) ) ;
#44809 = CARTESIAN_POINT ( 'NONE',  ( -44.67409385541305511, -17.80920654474411435, 70.50000000000000000 ) ) ;
#44810 = VERTEX_POINT ( 'NONE', #41379 ) ;
#44811 = EDGE_LOOP ( 'NONE', ( #30381, #33786, #23812, #12368 ) ) ;
#44812 = ADVANCED_FACE ( 'NONE', ( #8156 ), #4443, .T. ) ;
#44813 = CARTESIAN_POINT ( 'NONE',  ( -23.38410589725464916, -10.33907962427212190, 59.71708035543083071 ) ) ;
#44814 = CARTESIAN_POINT ( 'NONE',  ( -24.68310392741195258, -16.48564297948346891, 59.37978378043003147 ) ) ;
#44815 = FACE_OUTER_BOUND ( 'NONE', #8347, .T. ) ;
#44816 = CIRCLE ( 'NONE', #32960, 5.249999999999998224 ) ;
#44817 = CARTESIAN_POINT ( 'NONE',  ( -16.93034385759798965, -6.857644439848013640, 49.98602051094139398 ) ) ;
#44818 = ADVANCED_FACE ( 'NONE', ( #760 ), #37175, .T. ) ;
#44819 = CARTESIAN_POINT ( 'NONE',  ( -7.433578433745469560, -16.27641334846635246, 54.54971261817296835 ) ) ;
#44820 = FACE_OUTER_BOUND ( 'NONE', #2346, .T. ) ;
#44821 = CARTESIAN_POINT ( 'NONE',  ( -16.94458633259734270, -7.374567983260779336, 74.14513688882354359 ) ) ;
#44822 = CARTESIAN_POINT ( 'NONE',  ( -17.75227477277866939, -19.48420168222600068, 49.52966884056656482 ) ) ;
#44823 = ORIENTED_EDGE ( 'NONE', *, *, #35977, .F. ) ;
#44824 = CARTESIAN_POINT ( 'NONE',  ( -19.66559402580761784, -10.06176755239059695, 52.02966884056656482 ) ) ;
#44825 = CARTESIAN_POINT ( 'NONE',  ( -40.92409385541305511, -14.80920654474410725, 74.99999999999998579 ) ) ;
#44826 = VECTOR ( 'NONE', #37372, 1000.000000000000000 ) ;
#44827 = CARTESIAN_POINT ( 'NONE',  ( -10.20197030601470090, -12.78660143320473175, 53.49999999999994316 ) ) ;
#44828 = ORIENTED_EDGE ( 'NONE', *, *, #31564, .T. ) ;
#44829 = VERTEX_POINT ( 'NONE', #48518 ) ;
#44830 = DIRECTION ( 'NONE',  ( -1.000000000000000000, 0.000000000000000000, 3.652049423109068320E-16 ) ) ;
#44831 = CARTESIAN_POINT ( 'NONE',  ( -21.13535303541994281, -18.52256826949110646, 50.77966884056655772 ) ) ;
#44832 = VECTOR ( 'NONE', #2905, 1000.000000000000114 ) ;
#44833 = DIRECTION ( 'NONE',  ( -0.9687793358424819923, 0.2479245821708680464, 0.000000000000000000 ) ) ;
#44834 = CARTESIAN_POINT ( 'NONE',  ( -13.83108299072750391, -21.33561835983412891, 72.04112301026525245 ) ) ;
#44835 =( BOUNDED_CURVE ( )  B_SPLINE_CURVE ( 3, ( #33594, #26728, #18337, #11222 ),
 .UNSPECIFIED., .F., .F. ) 
 B_SPLINE_CURVE_WITH_KNOTS ( ( 4, 4 ),
 ( 0.5000000000000000000, 0.9074455897393695070 ),
 .UNSPECIFIED. ) 
 CURVE ( )  GEOMETRIC_REPRESENTATION_ITEM ( )  RATIONAL_B_SPLINE_CURVE ( ( 0.9999999999999745759, 0.4567392136813185344, 0.3561768502900429789, 0.6983129098261203760 ) ) 
 REPRESENTATION_ITEM ( '' )  );
#44836 = ORIENTED_EDGE ( 'NONE', *, *, #7063, .F. ) ;
#44837 = AXIS2_PLACEMENT_3D ( 'NONE', #19129, #48428, #22843 ) ;
#44838 = CARTESIAN_POINT ( 'NONE',  ( -24.64621740481133116, -16.83181165628401033, 54.27966884056654351 ) ) ;
#44839 = DIRECTION ( 'NONE',  ( 0.9562635972186041000, -0.2925062950340273638, 4.666065131241568958E-08 ) ) ;
#44840 = ORIENTED_EDGE ( 'NONE', *, *, #11876, .F. ) ;
#44841 = CARTESIAN_POINT ( 'NONE',  ( -22.78678303852979070, -9.565966637465479039, 47.99999999999994316 ) ) ;
#44842 = VECTOR ( 'NONE', #39860, 1000.000000000000000 ) ;
#44843 = CARTESIAN_POINT ( 'NONE',  ( -14.60689764421331738, -8.346551857622413806, 63.78978840692985131 ) ) ;
#44844 = CARTESIAN_POINT ( 'NONE',  ( -14.07539681412750987, -8.605278097683306981, 74.49954655214880006 ) ) ;
#44845 = EDGE_CURVE ( 'NONE', #19358, #24660, #14753, .T. ) ;
#44846 = ORIENTED_EDGE ( 'NONE', *, *, #41314, .T. ) ;
#44847 = CARTESIAN_POINT ( 'NONE',  ( -28.42409385541305511, -6.359206544744109735, 52.99999999999997158 ) ) ;
#44848 =( BOUNDED_CURVE ( )  B_SPLINE_CURVE ( 3, ( #4263, #3772, #23466, #34278 ),
 .UNSPECIFIED., .F., .F. ) 
 B_SPLINE_CURVE_WITH_KNOTS ( ( 4, 4 ),
 ( 0.000000000000000000, 0.4074455897393673975 ),
 .UNSPECIFIED. ) 
 CURVE ( )  GEOMETRIC_REPRESENTATION_ITEM ( )  RATIONAL_B_SPLINE_CURVE ( ( 1.000000000000000000, 0.4567392136813307468, 0.3561768502900298783, 0.6983129098260973944 ) ) 
 REPRESENTATION_ITEM ( '' )  );
#44849 = ORIENTED_EDGE ( 'NONE', *, *, #13606, .T. ) ;
#44850 = CARTESIAN_POINT ( 'NONE',  ( -19.57699507595987143, -21.94144279212693860, 62.17998934563075153 ) ) ;
#44851 = DIRECTION ( 'NONE',  ( 0.9687793358424813261, -0.2479245821708705166, 1.273414158200120423E-16 ) ) ;
#44852 = VERTEX_POINT ( 'NONE', #18719 ) ;
#44853 = CARTESIAN_POINT ( 'NONE',  ( -11.25989433568915032, -11.38792842781904469, 64.44882039367774951 ) ) ;
#44854 = CARTESIAN_POINT ( 'NONE',  ( -21.20534385650551812, -8.801233750844183135, 48.81488406609782515 ) ) ;
#44855 = CARTESIAN_POINT ( 'NONE',  ( -45.98959949296581584, -14.20920654474410760, 71.05212771298751306 ) ) ;
#44856 = CARTESIAN_POINT ( 'NONE',  ( -24.86969121598721344, -14.53217971827670496, 66.36947994509128534 ) ) ;
#44857 = CARTESIAN_POINT ( 'NONE',  ( -35.32409385541306079, -6.359206544744109735, 52.29999999999998295 ) ) ;
#44858 = B_SPLINE_CURVE_WITH_KNOTS ( 'NONE', 3,
 ( #2923, #10807, #17466, #44550, #14704, #32950, #48470, #2689, #9852, #40365 ),
 .UNSPECIFIED., .F., .F.,
 ( 4, 2, 2, 2, 4 ),
 ( 0.1272669073658279915, 0.2522669073463119638, 0.3772669073267959083, 0.5022669073072799639, 0.6272669072877639085 ),
 .UNSPECIFIED. ) ;
#44859 = CARTESIAN_POINT ( 'NONE',  ( -24.18470913683765389, -12.80901137141652768, 69.78715111652664405 ) ) ;
#44860 = ORIENTED_EDGE ( 'NONE', *, *, #33297, .T. ) ;
#44861 = DIRECTION ( 'NONE',  ( -3.071710424422018668E-17, 6.404604876783312462E-16, 1.000000000000000000 ) ) ;
#44862 = CARTESIAN_POINT ( 'NONE',  ( -22.65122085952885556, -20.11767465994831738, 69.27443734771573247 ) ) ;
#44863 = FACE_OUTER_BOUND ( 'NONE', #6089, .T. ) ;
#44864 = B_SPLINE_CURVE_WITH_KNOTS ( 'NONE', 1,
 ( #4267, #95 ),
 .UNSPECIFIED., .F., .F.,
 ( 2, 2 ),
 ( 0.000000000000000000, 1.000000000000000000 ),
 .UNSPECIFIED. ) ;
#44865 = FACE_OUTER_BOUND ( 'NONE', #148, .T. ) ;
#44866 = CARTESIAN_POINT ( 'NONE',  ( -23.76916757952739090, -18.71361706205413000, 72.88651372856567434 ) ) ;
#44867 = VERTEX_POINT ( 'NONE', #33733 ) ;
#44868 = VERTEX_POINT ( 'NONE', #30 ) ;
#44869 = EDGE_CURVE ( 'NONE', #16178, #23498, #5377, .T. ) ;
#44870 = VECTOR ( 'NONE', #37067, 1000.000000000000227 ) ;
#44871 = CARTESIAN_POINT ( 'NONE',  ( -36.42409385541304800, -9.359200813967566646, 50.49621490985803263 ) ) ;
#44872 = CARTESIAN_POINT ( 'NONE',  ( -6.424093855413055110, -25.10920654474410441, 47.99999999999998579 ) ) ;
#44873 = VERTEX_POINT ( 'NONE', #16959 ) ;
#44875 = DIRECTION ( 'NONE',  ( 0.3668819201507681482, -0.9245033139891514207, 0.1033986416233890204 ) ) ;
#44874 = CYLINDRICAL_SURFACE ( 'NONE', #24339, 0.1500000000000050460 ) ;
#44876 = DIRECTION ( 'NONE',  ( -5.731567514496413899E-31, -1.020425574103664789E-16, -1.000000000000000000 ) ) ;
#44877 = CARTESIAN_POINT ( 'NONE',  ( -20.71604796063133591, -8.125966986502412226, 63.41097886120039817 ) ) ;
#44878 = EDGE_CURVE ( 'NONE', #7346, #38535, #611, .T. ) ;
#44879 = CARTESIAN_POINT ( 'NONE',  ( -24.72409385541305582, -14.90920654474411577, 58.00588235294116402 ) ) ;
#44880 = CYLINDRICAL_SURFACE ( 'NONE', #4685, 7.000000000000000888 ) ;
#44881 = FACE_OUTER_BOUND ( 'NONE', #31416, .T. ) ;
#44882 = AXIS2_PLACEMENT_3D ( 'NONE', #24721, #43924, #33037 ) ;
#44883 = CARTESIAN_POINT ( 'NONE',  ( -10.42413885153580644, -14.85581157485834503, 74.79778936448731486 ) ) ;
#44884 = PRODUCT_DEFINITION_SHAPE ( 'NONE', 'NONE',  #48736 ) ;
#44885 = EDGE_CURVE ( 'NONE', #26170, #4590, #24136, .T. ) ;
#44886 = CARTESIAN_POINT ( 'NONE',  ( -16.65537394168718421, -21.76815631184664213, 68.92390547312155036 ) ) ;
#44887 = EDGE_LOOP ( 'NONE', ( #22885, #33640, #27378, #13948, #17870 ) ) ;
#44888 = LINE ( 'NONE', #33508, #39242 ) ;
#44889 = CARTESIAN_POINT ( 'NONE',  ( -10.38752013045322009, -14.36951432065623813, 64.67331771650336236 ) ) ;
#44890 = AXIS2_PLACEMENT_3D ( 'NONE', #35774, #27677, #20044 ) ;
#44891 = CARTESIAN_POINT ( 'NONE',  ( 23.62590614458706639, 1.890747609047893185, 50.53028072113869484 ) ) ;
#44892 = CARTESIAN_POINT ( 'NONE',  ( -17.92193066645248578, -21.84160715981037981, 62.02535923543162966 ) ) ;
#44893 = DIRECTION ( 'NONE',  ( -3.361323641615342917E-32, -0.9999954153791273948, -0.003028072113822189229 ) ) ;
#44894 = ADVANCED_FACE ( 'NONE', ( #42365 ), #20331, .T. ) ;
#44895 = CARTESIAN_POINT ( 'NONE',  ( -21.65914559189701194, -18.31838547852702703, 54.07175714974879099 ) ) ;
#44896 = CYLINDRICAL_SURFACE ( 'NONE', #23697, 1.250000000000001110 ) ;
#44897 = ORIENTED_EDGE ( 'NONE', *, *, #6264, .F. ) ;
#44898 = VERTEX_POINT ( 'NONE', #4946 ) ;
#44899 = CARTESIAN_POINT ( 'NONE',  ( -13.32679657360227488, -8.507250439495127381, 49.03377012338315666 ) ) ;
#44900 = ORIENTED_EDGE ( 'NONE', *, *, #23477, .F. ) ;
#44901 = CARTESIAN_POINT ( 'NONE',  ( -15.97409385759799072, -6.859212275519751323, 50.50378509014259265 ) ) ;
#44902 = LINE ( 'NONE', #18774, #22129 ) ;
#44903 = AXIS2_PLACEMENT_3D ( 'NONE', #9762, #27736, #9039 ) ;
#44904 = CARTESIAN_POINT ( 'NONE',  ( -15.37363155966973061, -7.646927905176254647, 74.27974431700636160 ) ) ;
#44905 = DIRECTION ( 'NONE',  ( -0.1240347345892086200, 1.145860353393066553E-16, -0.9922778767136676281 ) ) ;
#44906 = ORIENTED_EDGE ( 'NONE', *, *, #10542, .T. ) ;
#44907 = CIRCLE ( 'NONE', #33877, 5.249999999999998224 ) ;
#44908 = FACE_OUTER_BOUND ( 'NONE', #3757, .T. ) ;
#44909 = CARTESIAN_POINT ( 'NONE',  ( -17.56717507065399531, -7.360494836047319467, 63.73552460944732445 ) ) ;
#44910 = ORIENTED_EDGE ( 'NONE', *, *, #27926, .T. ) ;
#44911 = CARTESIAN_POINT ( 'NONE',  ( -14.97035482569482312, -21.41873484682592377, 61.92128389535452015 ) ) ;
#44912 = EDGE_CURVE ( 'NONE', #5348, #36746, #41117, .T. ) ;
#44913 = AXIS2_PLACEMENT_3D ( 'NONE', #12664, #42226, #614 ) ;
#44914 = DIRECTION ( 'NONE',  ( 0.2465957053274518418, 0.9635866743705491233, 0.1033986416233889788 ) ) ;
#44915 = ORIENTED_EDGE ( 'NONE', *, *, #31712, .F. ) ;
#44916 = CARTESIAN_POINT ( 'NONE',  ( -17.95491883169589542, -21.84291603085813804, 58.40553388833760096 ) ) ;
#44917 = DIRECTION ( 'NONE',  ( 0.9687793358424821033, -0.2479245821708679909, 0.000000000000000000 ) ) ;
#44918 = CARTESIAN_POINT ( 'NONE',  ( -13.71338950266841294, -20.80363499509022773, 64.98628881289567971 ) ) ;
#44919 = VERTEX_POINT ( 'NONE', #1468 ) ;
#44920 = DIRECTION ( 'NONE',  ( 0.04287186434519785205, 0.9990805789562555717, -2.806673972535357682E-09 ) ) ;
#44921 = CARTESIAN_POINT ( 'NONE',  ( -24.73385245812551503, -16.24793116159999684, 62.74328673523763200 ) ) ;
#44922 = AXIS2_PLACEMENT_3D ( 'NONE', #37716, #4006, #7956 ) ;
#44923 = B_SPLINE_CURVE_WITH_KNOTS ( 'NONE', 1,
 ( #14459, #32259 ),
 .UNSPECIFIED., .F., .F.,
 ( 2, 2 ),
 ( 0.000000000000000000, 1.000000000000000000 ),
 .UNSPECIFIED. ) ;
#44924 = LINE ( 'NONE', #14103, #36067 ) ;
#44925 = CARTESIAN_POINT ( 'NONE',  ( -10.52422472645684870, -17.61911478008853749, 68.21226617000660042 ) ) ;
#44926 = EDGE_LOOP ( 'NONE', ( #21312, #11195, #12848, #27211 ) ) ;
#44927 = CARTESIAN_POINT ( 'NONE',  ( -24.69816866750256779, -16.41902046076232935, 59.16686479676427979 ) ) ;
#44928 = DIRECTION ( 'NONE',  ( -1.000000000000000000, 0.000000000000000000, 0.000000000000000000 ) ) ;
#44929 = EDGE_CURVE ( 'NONE', #20972, #40656, #32071, .T. ) ;
#44930 = DIRECTION ( 'NONE',  ( -0.8507615431891571989, 0.5255518971808581519, 6.876821558984484920E-08 ) ) ;
#44931 = CARTESIAN_POINT ( 'NONE',  ( -21.76886496386750736, -13.05243499865792067, 49.52966884056655772 ) ) ;
#44932 = CARTESIAN_POINT ( 'NONE',  ( -19.03659385650551528, -6.915538690918074494, 49.31353937987644542 ) ) ;
#44933 = ORIENTED_EDGE ( 'NONE', *, *, #13658, .T. ) ;
#44934 = DIRECTION ( 'NONE',  ( -0.1464579420318390668, 0.9892168979631277281, 7.284849527811297202E-08 ) ) ;
#44935 = CARTESIAN_POINT ( 'NONE',  ( -21.31784385759798184, -6.860780111191487229, 51.02154966934377001 ) ) ;
#44936 = EDGE_LOOP ( 'NONE', ( #592, #7687, #25358, #25314, #40851 ) ) ;
#44937 = CARTESIAN_POINT ( 'NONE',  ( -17.42409385541300892, -14.80920654474439679, 47.99999999999994316 ) ) ;
#44938 =( BOUNDED_CURVE ( )  B_SPLINE_CURVE ( 3, ( #42397, #8666, #38690, #4973 ),
 .UNSPECIFIED., .F., .T. ) 
 B_SPLINE_CURVE_WITH_KNOTS ( ( 4, 4 ),
 ( 0.4074455897393651216, 0.5000000000000000000 ),
 .UNSPECIFIED. ) 
 CURVE ( )  GEOMETRIC_REPRESENTATION_ITEM ( )  RATIONAL_B_SPLINE_CURVE ( ( 0.6983129098261068313, 0.7760317562606926511, 0.8765941196519854151, 0.9999999999999723554 ) ) 
 REPRESENTATION_ITEM ( '' )  );
#44939 = CARTESIAN_POINT ( 'NONE',  ( -15.43373621257565276, -8.098073005819149017, 74.09488064067743096 ) ) ;
#44940 = DIRECTION ( 'NONE',  ( -3.071710424422018668E-17, 6.404604876783312462E-16, 1.000000000000000000 ) ) ;
#44941 = ORIENTED_EDGE ( 'NONE', *, *, #35110, .F. ) ;
#44942 = CARTESIAN_POINT ( 'NONE',  ( -10.37569183047413723, -14.65229009179183883, 71.33342454697773860 ) ) ;
#44943 = ADVANCED_FACE ( 'NONE', ( #19954 ), #34726, .T. ) ;
#44944 = CARTESIAN_POINT ( 'NONE',  ( -17.42409385541299471, -14.80920654474435594, 52.02966884056656482 ) ) ;
#44945 = ORIENTED_EDGE ( 'NONE', *, *, #24280, .T. ) ;
#44946 = ORIENTED_EDGE ( 'NONE', *, *, #22764, .T. ) ;
#44947 = CARTESIAN_POINT ( 'NONE',  ( -15.26784385650551989, -6.428312510596451368, 51.20221977374900035 ) ) ;
#44948 = ADVANCED_FACE ( 'NONE', ( #1958 ), #12559, .T. ) ;
#44949 = EDGE_CURVE ( 'NONE', #31311, #3912, #15264, .T. ) ;
#44950 = CARTESIAN_POINT ( 'NONE',  ( -18.84272689959381353, -7.495397202044052243, 70.54880819107169998 ) ) ;
#44951 = CARTESIAN_POINT ( 'NONE',  ( -21.76243611580424897, -17.76577320756515022, 52.02966884056656482 ) ) ;
#44952 = CARTESIAN_POINT ( 'NONE',  ( -15.62222905942472018, -7.993050613273783966, 70.89517703929612935 ) ) ;
#44953 = CARTESIAN_POINT ( 'NONE',  ( -13.60894707410760240, -8.877133421815647907, 60.85439169328856934 ) ) ;
#44954 = VECTOR ( 'NONE', #17123, 1000.000000000000000 ) ;
#44955 = ORIENTED_EDGE ( 'NONE', *, *, #40561, .T. ) ;
#44956 = ORIENTED_EDGE ( 'NONE', *, *, #43986, .T. ) ;
#44957 = CARTESIAN_POINT ( 'NONE',  ( -15.74909385650551386, -8.104110260919579645, 48.81699501597546487 ) ) ;
#44958 = CARTESIAN_POINT ( 'NONE',  ( -10.44647900978708321, -14.24909228104994696, 60.99109301640115177 ) ) ;
#44959 = AXIS2_PLACEMENT_3D ( 'NONE', #39371, #42102, #42345 ) ;
#44960 = CARTESIAN_POINT ( 'NONE',  ( -36.42409385541304800, -8.109206544743658540, 50.50000000000030553 ) ) ;
#44962 = EDGE_CURVE ( 'NONE', #4699, #4476, #31273, .T. ) ;
#44961 = CARTESIAN_POINT ( 'NONE',  ( -16.19909385650551670, -8.114302828567740988, 52.18300498402516041 ) ) ;
#44963 = EDGE_CURVE ( 'NONE', #45424, #39489, #35675, .T. ) ;
#44964 = EDGE_LOOP ( 'NONE', ( #26103, #27823, #1860, #26144, #28075, #22313, #35795, #41689, #15514, #46623, #41299, #33082, #29346, #1148 ) ) ;
#44965 = EDGE_CURVE ( 'NONE', #46955, #47542, #18431, .T. ) ;
#44966 = EDGE_CURVE ( 'NONE', #10001, #656, #42872, .T. ) ;
#44967 = LINE ( 'NONE', #41007, #4189 ) ;
#44968 = AXIS2_PLACEMENT_3D ( 'NONE', #38722, #819, #1286 ) ;
#44969 = CARTESIAN_POINT ( 'NONE',  ( -18.76338093351206382, -7.938521699473153781, 67.00957693643654522 ) ) ;
#44970 = CARTESIAN_POINT ( 'NONE',  ( -24.38756562526642213, -15.91227465074932290, 66.34852784166324113 ) ) ;
#44971 = ORIENTED_EDGE ( 'NONE', *, *, #10402, .T. ) ;
#44972 = PLANE ( 'NONE',  #43005 ) ;
#44973 = ORIENTED_EDGE ( 'NONE', *, *, #35384, .F. ) ;
#44974 = AXIS2_PLACEMENT_3D ( 'NONE', #16651, #2608, #17609 ) ;
#44975 = DIRECTION ( 'NONE',  ( -2.866981220435666553E-17, 1.000000000000000000, 1.190614954331866791E-16 ) ) ;
#44976 = CARTESIAN_POINT ( 'NONE',  ( -18.26831436342312287, -21.75822329804466904, 69.11514735239036611 ) ) ;
#44977 = CARTESIAN_POINT ( 'NONE',  ( -24.40169278593617008, -17.41991595014878769, 69.51365538212004935 ) ) ;
#44978 = CARTESIAN_POINT ( 'NONE',  ( -13.43773910423563400, -20.62433115109003268, 58.33177939114180788 ) ) ;
#44979 = AXIS2_PLACEMENT_3D ( 'NONE', #45072, #48241, #48011 ) ;
#44980 = ORIENTED_EDGE ( 'NONE', *, *, #34215, .F. ) ;
#44981 = DIRECTION ( 'NONE',  ( -2.866981220435666553E-17, 1.000000000000000000, 1.190614954331866791E-16 ) ) ;
#44982 =( BOUNDED_CURVE ( )  B_SPLINE_CURVE ( 3, ( #19241, #15520, #34243, #34004 ),
 .UNSPECIFIED., .F., .F. ) 
 B_SPLINE_CURVE_WITH_KNOTS ( ( 4, 4 ),
 ( 0.9074455897393650661, 1.000000000000000000 ),
 .UNSPECIFIED. ) 
 CURVE ( )  GEOMETRIC_REPRESENTATION_ITEM ( )  RATIONAL_B_SPLINE_CURVE ( ( 0.6983129098260931755, 0.7760317562606983133, 0.8765941196520006251, 1.000000000000000000 ) ) 
 REPRESENTATION_ITEM ( '' )  );
#44983 = DIRECTION ( 'NONE',  ( 0.9757441136919974278, 0.2189141945955501434, 0.000000000000000000 ) ) ;
#44984 = FACE_OUTER_BOUND ( 'NONE', #16101, .T. ) ;
#44985 = ORIENTED_EDGE ( 'NONE', *, *, #8873, .F. ) ;
#44986 = CARTESIAN_POINT ( 'NONE',  ( -22.27409385759798965, -6.859212275519751323, 50.50378509014259265 ) ) ;
#44987 = CARTESIAN_POINT ( 'NONE',  ( -17.22281210278579167, -7.361840297529252730, 70.60540404266352255 ) ) ;
#44988 = CARTESIAN_POINT ( 'NONE',  ( -10.74028706782022269, -11.51804935604180358, 71.25007375637602536 ) ) ;
#44989 = FACE_BOUND ( 'NONE', #9895, .T. ) ;
#44990 = ORIENTED_EDGE ( 'NONE', *, *, #28274, .T. ) ;
#44991 = CARTESIAN_POINT ( 'NONE',  ( -10.56492523587830235, -13.18000265412059058, 71.35828586226037373 ) ) ;
#44993 = EDGE_CURVE ( 'NONE', #36884, #16630, #11641, .T. ) ;
#44992 = CARTESIAN_POINT ( 'NONE',  ( -10.81230840161673967, -17.25685697075765646, 64.64211442681141762 ) ) ;
#44994 = CARTESIAN_POINT ( 'NONE',  ( -24.41709716369935990, -14.49630903675724625, 62.82182603900851348 ) ) ;
#44995 = CARTESIAN_POINT ( 'NONE',  ( -14.59284385541304907, -8.630756214087124789, 51.74842643355248129 ) ) ;
#44996 = ORIENTED_EDGE ( 'NONE', *, *, #43793, .F. ) ;
#44997 = DIRECTION ( 'NONE',  ( 2.866981220435666553E-17, -1.000000000000000000, -1.190614954331866791E-16 ) ) ;
#44998 = VECTOR ( 'NONE', #39852, 999.9999999999998863 ) ;
#44999 = ORIENTED_EDGE ( 'NONE', *, *, #17162, .T. ) ;
#45000 = CARTESIAN_POINT ( 'NONE',  ( -12.69197368675297355, -9.055053595461757254, 70.95587035088203720 ) ) ;
#45001 = CARTESIAN_POINT ( 'NONE',  ( -15.48261606618132546, -10.53062973237824096, 49.52966884056655772 ) ) ;
#45002 = DIRECTION ( 'NONE',  ( 0.9811758422909349076, 0.1931164583992469319, 7.863147543881890502E-08 ) ) ;
#45003 = ORIENTED_EDGE ( 'NONE', *, *, #37886, .T. ) ;
#45004 = CARTESIAN_POINT ( 'NONE',  ( -16.14077005943513399, -22.14785303186519627, 58.38561932509040986 ) ) ;
#45005 =( BOUNDED_SURFACE ( )  B_SPLINE_SURFACE ( 3, 1, ( 
 ( #2372, #20617 ),
 ( #47441, #5605 ),
 ( #47674, #32180 ),
 ( #24067, #13439 ),
 ( #28487, #35375 ),
 ( #46716, #9778 ),
 ( #12958, #27986 ) ),
 .UNSPECIFIED., .T., .F., .F. ) 
 B_SPLINE_SURFACE_WITH_KNOTS ( ( 4, 3, 4 ),
 ( 2, 2 ),
 ( 0.000000000000000000, 0.5000000000000000000, 1.000000000000000000 ),
 ( 0.000000000000000000, 1.000000000000000000 ),
 .UNSPECIFIED. ) 
 GEOMETRIC_REPRESENTATION_ITEM ( )  RATIONAL_B_SPLINE_SURFACE ( (
 ( 1.000000000000000000, 1.000000000000000000),
 ( 0.3333333333333335369, 0.3333333333333330373),
 ( 0.3333333333333335369, 0.3333333333333330373),
 ( 1.000000000000000000, 1.000000000000000000),
 ( 0.3333333333333333703, 0.3333333333333333703),
 ( 0.3333333333333333703, 0.3333333333333333703),
 ( 1.000000000000000000, 1.000000000000000000) ) ) 
 REPRESENTATION_ITEM ( '' )  SURFACE ( )  );
#45006 = CARTESIAN_POINT ( 'NONE',  ( -11.01240199294250033, -17.61815787592479055, 68.20608059829778824 ) ) ;
#45007 = EDGE_CURVE ( 'NONE', #38000, #28514, #7021, .T. ) ;
#45008 = ORIENTED_EDGE ( 'NONE', *, *, #7572, .T. ) ;
#45009 = VERTEX_POINT ( 'NONE', #47512 ) ;
#45010 = ORIENTED_EDGE ( 'NONE', *, *, #19691, .F. ) ;
#45011 = DIRECTION ( 'NONE',  ( 1.000000000000000000, 0.000000000000000000, 0.000000000000000000 ) ) ;
#45012 = CARTESIAN_POINT ( 'NONE',  ( -24.00901317767523935, -17.32824147414624960, 69.42811846502259243 ) ) ;
#45013 = CARTESIAN_POINT ( 'NONE',  ( -19.35357574399719027, -22.00502143967494817, 58.62483747956095215 ) ) ;
#45014 = CARTESIAN_POINT ( 'NONE',  ( -10.57910656192517784, -13.34370627372683416, 74.67817676091868861 ) ) ;
#45015 = CARTESIAN_POINT ( 'NONE',  ( -10.37567211895962060, -17.22253062098360488, 61.28026218318612450 ) ) ;
#45016 = CARTESIAN_POINT ( 'NONE',  ( -24.72409385541305582, -14.90920654474413709, 60.01764705882352047 ) ) ;
#45017 = VERTEX_POINT ( 'NONE', #17925 ) ;
#45018 = EDGE_LOOP ( 'NONE', ( #33375, #38251, #39728, #7770, #32518 ) ) ;
#45019 = CARTESIAN_POINT ( 'NONE',  ( -16.16063032598464133, -7.467038112641824377, 60.38523865926408263 ) ) ;
#45020 = TOROIDAL_SURFACE ( 'NONE', #13513, 2.000000000000001776, 1.249999999999999334 ) ;
#45021 = CARTESIAN_POINT ( 'NONE',  ( -10.38752013045322009, -14.36951432065623635, 64.67331771650336236 ) ) ;
#45022 = CARTESIAN_POINT ( 'NONE',  ( -24.29232294273250758, -16.16103065725259214, 62.59328677063434299 ) ) ;
#45023 = ORIENTED_EDGE ( 'NONE', *, *, #27266, .T. ) ;
#45024 = CARTESIAN_POINT ( 'NONE',  ( -16.39284385650552167, -7.406986770994973490, 48.81910596585309747 ) ) ;
#45025 = EDGE_CURVE ( 'NONE', #30144, #748, #9972, .T. ) ;
#45026 = ORIENTED_EDGE ( 'NONE', *, *, #1889, .F. ) ;
#45027 = EDGE_CURVE ( 'NONE', #41560, #17399, #13745, .T. ) ;
#45028 = EDGE_CURVE ( 'NONE', #15971, #33162, #23515, .T. ) ;
#45029 = CARTESIAN_POINT ( 'NONE',  ( -17.56322643164902431, -15.18422937902243142, 54.49999999999994316 ) ) ;
#45030 = CARTESIAN_POINT ( 'NONE',  ( -22.19874839824752044, -20.52805027805738902, 58.91442897818879487 ) ) ;
#45031 = DIRECTION ( 'NONE',  ( 0.9687793358424823253, -0.2479245821708663811, 0.000000000000000000 ) ) ;
#45032 = B_SPLINE_CURVE_WITH_KNOTS ( 'NONE', 3,
 ( #35260, #23475, #13086, #46613, #34787, #34533, #38962, #814, #39203, #19780 ),
 .UNSPECIFIED., .F., .F.,
 ( 4, 2, 2, 2, 4 ),
 ( 0.6272669072878143126, 0.7522669073073209312, 0.8772669073268274387, 1.002266907346333946, 1.127266907365840565 ),
 .UNSPECIFIED. ) ;
#45033 = VERTEX_POINT ( 'NONE', #43827 ) ;
#45034 = DIRECTION ( 'NONE',  ( 0.000000000000000000, 0.000000000000000000, 1.000000000000000000 ) ) ;
#45035 = ADVANCED_FACE ( 'NONE', ( #47740 ), #32485, .T. ) ;
#45036 = EDGE_CURVE ( 'NONE', #12877, #43417, #40355, .T. ) ;
#45037 = CARTESIAN_POINT ( 'NONE',  ( -21.79028809537168243, -9.273590339475653366, 63.47681654923867711 ) ) ;
#45038 = CARTESIAN_POINT ( 'NONE',  ( -10.47425521701617157, -17.49314416303823450, 64.81234701634230078 ) ) ;
#45039 = B_SPLINE_CURVE_WITH_KNOTS ( 'NONE', 3,
 ( #29770, #14231, #29283, #44316, #14701, #36886, #14460, #29519, #10804, #37126 ),
 .UNSPECIFIED., .F., .F.,
 ( 4, 2, 2, 2, 4 ),
 ( 0.6272669072877813390, 0.7522669073072901780, 0.8772669073267991280, 1.002266907346307967, 1.127266907365816806 ),
 .UNSPECIFIED. ) ;
#45040 = ORIENTED_EDGE ( 'NONE', *, *, #559, .F. ) ;
#45041 = CARTESIAN_POINT ( 'NONE',  ( -18.68183629324915174, -7.872155521403883860, 70.66508205815506471 ) ) ;
#45042 = DIRECTION ( 'NONE',  ( -5.408674110437222193E-06, 4.460197095916123975E-06, 0.9999999999754265456 ) ) ;
#45043 = CARTESIAN_POINT ( 'NONE',  ( -23.98503169607928953, -17.39005800936845603, 66.22885190747201989 ) ) ;
#45044 = ORIENTED_EDGE ( 'NONE', *, *, #40294, .F. ) ;
#45045 = CARTESIAN_POINT ( 'NONE',  ( -16.03473429733671196, -7.489776097686932310, 63.79294168612747740 ) ) ;
#45046 = VERTEX_POINT ( 'NONE', #17204 ) ;
#45047 = PLANE ( 'NONE',  #39937 ) ;
#45048 = CARTESIAN_POINT ( 'NONE',  ( -12.41315146567208139, -9.850077947585075933, 57.08935532239182464 ) ) ;
#45049 = ORIENTED_EDGE ( 'NONE', *, *, #36374, .F. ) ;
#45050 = CARTESIAN_POINT ( 'NONE',  ( -45.98959949296318683, -14.20920654474410760, 69.94787228701220272 ) ) ;
#45052 = ADVANCED_FACE ( 'NONE', ( #6385 ), #6144, .T. ) ;
#45051 = PLANE ( 'NONE',  #2710 ) ;
#45053 = DIRECTION ( 'NONE',  ( -5.731567514496413899E-31, -1.020425574103664789E-16, -1.000000000000000000 ) ) ;
#45054 = ORIENTED_EDGE ( 'NONE', *, *, #43570, .F. ) ;
#45055 = CARTESIAN_POINT ( 'NONE',  ( -22.09234508783963236, -20.09219152016766685, 62.38439162497947166 ) ) ;
#45056 = CARTESIAN_POINT ( 'NONE',  ( -10.61330258792943226, -12.98832159324075874, 68.03832347271723791 ) ) ;
#45057 = CARTESIAN_POINT ( 'NONE',  ( -21.99649211598757859, -13.72812852161587038, 49.52966884056655772 ) ) ;
#45058 = ORIENTED_EDGE ( 'NONE', *, *, #7604, .T. ) ;
#45059 = CARTESIAN_POINT ( 'NONE',  ( -12.64905295888074299, -9.611711778639854487, 57.23368232919959553 ) ) ;
#45060 = CARTESIAN_POINT ( 'NONE',  ( -21.80063255203189243, -8.780035963955921119, 70.29279082220594432 ) ) ;
#45061 = CARTESIAN_POINT ( 'NONE',  ( -24.38497043871102576, -15.94922339405466971, 62.80148391248476258 ) ) ;
#45062 = ORIENTED_EDGE ( 'NONE', *, *, #22335, .F. ) ;
#45063 = ORIENTED_EDGE ( 'NONE', *, *, #38998, .T. ) ;
#45064 = DIRECTION ( 'NONE',  ( 1.277734862359329272E-05, 2.482875502418557358E-06, 0.9999999999152874297 ) ) ;
#45065 = CARTESIAN_POINT ( 'NONE',  ( -24.72409385541305582, -14.80920654474419962, 66.05294117647058272 ) ) ;
#45066 = CARTESIAN_POINT ( 'NONE',  ( -50.42609385541305755, -14.80920654474410902, 57.89999999999999147 ) ) ;
#45067 = ORIENTED_EDGE ( 'NONE', *, *, #36443, .T. ) ;
#45068 = CARTESIAN_POINT ( 'NONE',  ( -13.94909385759799214, -8.112991634885936776, 51.74999426922421719 ) ) ;
#45069 = CARTESIAN_POINT ( 'NONE',  ( -24.82002243867330549, -13.90704071453223456, 73.23616177064057808 ) ) ;
#45070 = CARTESIAN_POINT ( 'NONE',  ( -11.82099675438171005, -9.899106633794131582, 64.21409753874590365 ) ) ;
#45071 = CARTESIAN_POINT ( 'NONE',  ( -17.36459502086233186, -7.755746116514760757, 63.55057029956871872 ) ) ;
#45072 = CARTESIAN_POINT ( 'NONE',  ( -15.28291115335697192, -21.52618774670101232, 68.72592918174676413 ) ) ;
#45073 = VERTEX_POINT ( 'NONE', #29026 ) ;
#45074 = FACE_OUTER_BOUND ( 'NONE', #4978, .T. ) ;
#45075 =( NAMED_UNIT ( * ) PLANE_ANGLE_UNIT ( ) SI_UNIT ( $, .RADIAN. ) );
#45076 = AXIS2_PLACEMENT_3D ( 'NONE', #8200, #42168, #41681 ) ;
#45077 = CARTESIAN_POINT ( 'NONE',  ( -12.10599200002982556, -20.02663609087960239, 61.58174067880212021 ) ) ;
#45078 = DIRECTION ( 'NONE',  ( -3.071710424422018668E-17, 6.404604876783312462E-16, 1.000000000000000000 ) ) ;
#45079 = ORIENTED_EDGE ( 'NONE', *, *, #43863, .F. ) ;
#45080 = ORIENTED_EDGE ( 'NONE', *, *, #21330, .F. ) ;
#45081 = EDGE_CURVE ( 'NONE', #34284, #18372, #31685, .T. ) ;
#45082 = DIRECTION ( 'NONE',  ( 0.000000000000000000, -0.9999954153791273948, -0.003028072113819838245 ) ) ;
#45083 = CYLINDRICAL_SURFACE ( 'NONE', #14213, 0.1499999999999979128 ) ;
#45084 = EDGE_LOOP ( 'NONE', ( #2314, #7740, #19443, #22401, #44650, #39010 ) ) ;
#45085 = CARTESIAN_POINT ( 'NONE',  ( -23.59267638082966201, -11.50008196526012760, 66.42214495376651939 ) ) ;
#45086 = EDGE_CURVE ( 'NONE', #19297, #44898, #25076, .T. ) ;
#45087 = EDGE_CURVE ( 'NONE', #17746, #7006, #21644, .T. ) ;
#45088 = ORIENTED_EDGE ( 'NONE', *, *, #46911, .T. ) ;
#45089 = EDGE_CURVE ( 'NONE', #25765, #39405, #25805, .T. ) ;
#45090 = CARTESIAN_POINT ( 'NONE',  ( -24.49635653881819408, -12.46679777644911447, 73.35730153580948354 ) ) ;
#45091 = ADVANCED_FACE ( 'NONE', ( #26309 ), #48643, .T. ) ;
#45092 = CARTESIAN_POINT ( 'NONE',  ( -10.86812116641377557, -17.26293110649939777, 64.62739382021851497 ) ) ;
#45093 = ORIENTED_EDGE ( 'NONE', *, *, #12273, .T. ) ;
#45094 = CARTESIAN_POINT ( 'NONE',  ( -21.68606078249201730, -9.256083098098587314, 66.96150029160082795 ) ) ;
#45095 = ORIENTED_EDGE ( 'NONE', *, *, #19931, .F. ) ;
#45096 = CARTESIAN_POINT ( 'NONE',  ( -11.93762650184002538, -19.84916447049328170, 58.07682373525275921 ) ) ;
#45097 = FACE_OUTER_BOUND ( 'NONE', #36461, .T. ) ;
#45098 = ORIENTED_EDGE ( 'NONE', *, *, #20553, .F. ) ;
#45099 = PLANE ( 'NONE',  #18346 ) ;
#45100 = DIRECTION ( 'NONE',  ( -0.6205284308219133349, -0.7841839494287637935, 8.002013567987292236E-17 ) ) ;
#45101 = EDGE_CURVE ( 'NONE', #19390, #9114, #29752, .T. ) ;
#45102 = CIRCLE ( 'NONE', #16768, 4.686499999999999666 ) ;
#45103 = CARTESIAN_POINT ( 'NONE',  ( -21.09284385650552096, -7.406986770994972602, 48.81910596585309747 ) ) ;
#45104 = CARTESIAN_POINT ( 'NONE',  ( -21.36284794767689377, -21.13297080501056513, 69.16954792666395235 ) ) ;
#45105 = CARTESIAN_POINT ( 'NONE',  ( -45.92409385541306222, -14.20920654474410760, 70.50000000000000000 ) ) ;
#45106 = CARTESIAN_POINT ( 'NONE',  ( -24.43617438265181008, -15.54086213135836303, 73.29743941331763324 ) ) ;
#45107 = CARTESIAN_POINT ( 'NONE',  ( -13.42200550436094453, -8.525284928264134976, 57.09250892727150273 ) ) ;
#45108 = EDGE_LOOP ( 'NONE', ( #46950, #33893, #9783, #42538 ) ) ;
#45109 = CARTESIAN_POINT ( 'NONE',  ( -19.09646890170684230, -21.60781482332639314, 58.59677732982556364 ) ) ;
#45110 = CARTESIAN_POINT ( 'NONE',  ( -15.47038452772150663, -21.58309165278561537, 72.04575460769355288 ) ) ;
#45111 = CARTESIAN_POINT ( 'NONE',  ( -18.24819606216845358, -21.76058716088148515, 65.41820204848704634 ) ) ;
#45112 = CARTESIAN_POINT ( 'NONE',  ( -17.42409385541300892, -14.80920654474439324, 56.49999999999994316 ) ) ;
#45113 = CARTESIAN_POINT ( 'NONE',  ( -17.42409385541299471, -14.80920654474435594, 52.02966884056656482 ) ) ;
#45114 = CARTESIAN_POINT ( 'NONE',  ( -42.29525584636328972, -14.90920654474419038, 64.03070407239817996 ) ) ;
#45115 = EDGE_LOOP ( 'NONE', ( #41953, #33535, #11310, #41426, #5592 ) ) ;
#45116 = VERTEX_POINT ( 'NONE', #41577 ) ;
#45117 = CARTESIAN_POINT ( 'NONE',  ( -23.99312320239454976, -11.29471777418100231, 66.60709819448160829 ) ) ;
#45118 = LINE ( 'NONE', #40659, #6904 ) ;
#45119 = ORIENTED_EDGE ( 'NONE', *, *, #31017, .F. ) ;
#45120 = CARTESIAN_POINT ( 'NONE',  ( -24.02536246799019892, -17.13931026604683083, 72.89952639825732206 ) ) ;
#45121 = DIRECTION ( 'NONE',  ( 0.9687793358424821033, -0.2479245821708679909, 0.000000000000000000 ) ) ;
#45122 = CARTESIAN_POINT ( 'NONE',  ( -12.74909871793134997, -15.13738746211001285, 52.02966884056656482 ) ) ;
#45123 = CARTESIAN_POINT ( 'NONE',  ( -17.24064286951094616, -7.811500644630894108, 70.79035835121598552 ) ) ;
#45124 =( BOUNDED_SURFACE ( )  B_SPLINE_SURFACE ( 3, 1, ( 
 ( #43537, #18127 ),
 ( #35871, #33142 ),
 ( #17647, #32443 ),
 ( #40315, #32675 ),
 ( #9801, #47697 ),
 ( #24814, #6585 ),
 ( #13702, #2871 ) ),
 .UNSPECIFIED., .T., .F., .F. ) 
 B_SPLINE_SURFACE_WITH_KNOTS ( ( 4, 3, 4 ),
 ( 2, 2 ),
 ( 0.000000000000000000, 0.5000000000000000000, 1.000000000000000000 ),
 ( 0.000000000000000000, 1.000000000000000000 ),
 .UNSPECIFIED. ) 
 GEOMETRIC_REPRESENTATION_ITEM ( )  RATIONAL_B_SPLINE_SURFACE ( (
 ( 1.000000000000000000, 1.000000000000000000),
 ( 0.3333333333333335369, 0.3333333333333330373),
 ( 0.3333333333333335369, 0.3333333333333330373),
 ( 1.000000000000000000, 1.000000000000000000),
 ( 0.3333333333333333703, 0.3333333333333333703),
 ( 0.3333333333333333703, 0.3333333333333333703),
 ( 1.000000000000000000, 1.000000000000000000) ) ) 
 REPRESENTATION_ITEM ( '' )  SURFACE ( )  );
#45125 = CARTESIAN_POINT ( 'NONE',  ( -17.92193035392797285, -21.84160718002658541, 61.87535923543196503 ) ) ;
#45126 = CARTESIAN_POINT ( 'NONE',  ( -23.59048307761029761, -18.99011851117282390, 66.00106286486899876 ) ) ;
#45127 = CARTESIAN_POINT ( 'NONE',  ( -15.55171133418867235, -7.598245370416885969, 70.79485226425863686 ) ) ;
#45128 = CARTESIAN_POINT ( 'NONE',  ( -16.78865592400587659, -21.78030535593112305, 68.99560651886281448 ) ) ;
#45129 = FACE_OUTER_BOUND ( 'NONE', #40978, .T. ) ;
#45130 = CARTESIAN_POINT ( 'NONE',  ( -17.56717507065399531, -7.360494836047319467, 63.73552460944732445 ) ) ;
#45131 = FACE_OUTER_BOUND ( 'NONE', #37813, .T. ) ;
#45132 = CARTESIAN_POINT ( 'NONE',  ( -15.65211633649168554, -8.035537180803068225, 74.26912783389062156 ) ) ;
#45133 = CARTESIAN_POINT ( 'NONE',  ( -24.28250172495594228, -13.40621956664827152, 59.64651430442704338 ) ) ;
#45134 = CARTESIAN_POINT ( 'NONE',  ( -22.96375064570672819, -10.44813988596692589, 63.08658113699938497 ) ) ;
#45135 = ADVANCED_FACE ( 'NONE', ( #30265 ), #45530, .T. ) ;
#45136 = DIRECTION ( 'NONE',  ( 1.000000000000000000, -4.164305804376849172E-17, 1.614929280266638808E-16 ) ) ;
#45137 =( BOUNDED_CURVE ( )  B_SPLINE_CURVE ( 3, ( #23653, #34216, #19212, #23161 ),
 .UNSPECIFIED., .F., .F. ) 
 B_SPLINE_CURVE_WITH_KNOTS ( ( 4, 4 ),
 ( 0.9074455897393668424, 1.000000000000000000 ),
 .UNSPECIFIED. ) 
 CURVE ( )  GEOMETRIC_REPRESENTATION_ITEM ( )  RATIONAL_B_SPLINE_CURVE ( ( 0.6983129098261089407, 0.7760317562607119690, 0.8765941196520089518, 1.000000000000000000 ) ) 
 REPRESENTATION_ITEM ( '' )  );
#45138 = CARTESIAN_POINT ( 'NONE',  ( -10.68602809008750576, -16.88409676349039046, 57.70232650191087487 ) ) ;
#45139 =( BOUNDED_CURVE ( )  B_SPLINE_CURVE ( 3, ( #36381, #13725, #36616, #40566 ),
 .UNSPECIFIED., .F., .F. ) 
 B_SPLINE_CURVE_WITH_KNOTS ( ( 4, 4 ),
 ( 0.9074455897393658432, 1.000000000000000000 ),
 .UNSPECIFIED. ) 
 CURVE ( )  GEOMETRIC_REPRESENTATION_ITEM ( )  RATIONAL_B_SPLINE_CURVE ( ( 0.6983129098260822953, 0.7760317562606889874, 0.8765941196519948519, 1.000000000000000000 ) ) 
 REPRESENTATION_ITEM ( '' )  );
#45140 = ORIENTED_EDGE ( 'NONE', *, *, #34363, .F. ) ;
#45141 = ORIENTED_EDGE ( 'NONE', *, *, #25022, .F. ) ;
#45142 = CARTESIAN_POINT ( 'NONE',  ( -13.58034385541304445, -9.360768649639302552, 51.01397948905922419 ) ) ;
#45143 = ORIENTED_EDGE ( 'NONE', *, *, #25441, .F. ) ;
#45144 = EDGE_CURVE ( 'NONE', #9318, #3630, #36671, .T. ) ;
#45145 = CARTESIAN_POINT ( 'NONE',  ( -16.30697390535036106, -7.848126388226943639, 60.20588296999211764 ) ) ;
#45146 = DIRECTION ( 'NONE',  ( 1.522745436688331916E-06, -7.096186242782870827E-06, 0.9999999999736625123 ) ) ;
#45147 =( BOUNDED_CURVE ( )  B_SPLINE_CURVE ( 3, ( #20564, #36033, #9480, #17069 ),
 .UNSPECIFIED., .F., .F. ) 
 B_SPLINE_CURVE_WITH_KNOTS ( ( 4, 4 ),
 ( 4.712388980384690562, 4.921828490624010399 ),
 .UNSPECIFIED. ) 
 CURVE ( )  GEOMETRIC_REPRESENTATION_ITEM ( )  RATIONAL_B_SPLINE_CURVE ( ( 1.000000000000000000, 0.9963479302455154896, 0.9963479302455154896, 1.000000000000000000 ) ) 
 REPRESENTATION_ITEM ( '' )  );
#45148 = CARTESIAN_POINT ( 'NONE',  ( -10.39147815561416621, -17.41829018061022438, 53.49999999999995026 ) ) ;
#45149 = CARTESIAN_POINT ( 'NONE',  ( -17.85555652284939043, -7.772123375420258107, 60.09532845646905486 ) ) ;
#45150 = ORIENTED_EDGE ( 'NONE', *, *, #26873, .T. ) ;
#45151 = EDGE_CURVE ( 'NONE', #6217, #29130, #25361, .T. ) ;
#45152 = CARTESIAN_POINT ( 'NONE',  ( -24.37280380791617418, -15.65865402563598430, 73.01920416708826167 ) ) ;
#45153 = CARTESIAN_POINT ( 'NONE',  ( -18.57721099958938282, -7.853998799284704013, 73.84624222578358399 ) ) ;
#45154 = EDGE_CURVE ( 'NONE', #39323, #42977, #3515, .T. ) ;
#45155 = VERTEX_POINT ( 'NONE', #48461 ) ;
#45156 = CARTESIAN_POINT ( 'NONE',  ( -17.09591293804728807, -10.13421140726271297, 49.52966884056655772 ) ) ;
#45157 = DIRECTION ( 'NONE',  ( 0.000000000000000000, 1.000000000000000000, -0.000000000000000000 ) ) ;
#45158 = ORIENTED_EDGE ( 'NONE', *, *, #18900, .T. ) ;
#45159 = EDGE_CURVE ( 'NONE', #1846, #6762, #14957, .T. ) ;
#45160 = CYLINDRICAL_SURFACE ( 'NONE', #21304, 1.999999999999999556 ) ;
#45161 = CARTESIAN_POINT ( 'NONE',  ( -14.98927377128279126, -8.246306944878790901, 56.84999999999994458 ) ) ;
#45162 = CARTESIAN_POINT ( 'NONE',  ( -23.37999588001404661, -18.58199455739222827, 69.57899840282863124 ) ) ;
#45163 = EDGE_LOOP ( 'NONE', ( #39429, #37504, #29369, #25862, #16028 ) ) ;
#45164 = CARTESIAN_POINT ( 'NONE',  ( -23.20805662353657439, -10.11344718840461887, 63.24902867775850268 ) ) ;
#45165 = FACE_OUTER_BOUND ( 'NONE', #1016, .T. ) ;
#45166 = EDGE_CURVE ( 'NONE', #15515, #16073, #14763, .T. ) ;
#45167 = CARTESIAN_POINT ( 'NONE',  ( -10.74628672884880132, -17.07053172313825939, 61.17215199736627795 ) ) ;
#45168 = CARTESIAN_POINT ( 'NONE',  ( -21.68495691188242702, -20.43592993620880804, 58.90875877921045145 ) ) ;
#45169 = EDGE_LOOP ( 'NONE', ( #44253, #11702, #17753, #19857, #6640 ) ) ;
#45170 = CARTESIAN_POINT ( 'NONE',  ( -10.91133513969588087, -12.10202850713728218, 74.44351760842475585 ) ) ;
#45171 = DIRECTION ( 'NONE',  ( -0.000000000000000000, 1.000000000000000000, -0.000000000000000000 ) ) ;
#45172 = FACE_OUTER_BOUND ( 'NONE', #42884, .T. ) ;
#45173 = CYLINDRICAL_SURFACE ( 'NONE', #47077, 1.999999999999999556 ) ;
#45174 = VECTOR ( 'NONE', #24405, 1000.000000000000000 ) ;
#45175 = CARTESIAN_POINT ( 'NONE',  ( -45.92409385541305511, -17.80920654474410370, 69.24999999999998579 ) ) ;
#45176 = CARTESIAN_POINT ( 'NONE',  ( -19.31784385650551528, -9.790100578890868377, 49.79778022625163203 ) ) ;
#45177 = TOROIDAL_SURFACE ( 'NONE', #12118, 2.000000000000001776, 1.249999999999999334 ) ;
#45178 = ORIENTED_EDGE ( 'NONE', *, *, #16958, .F. ) ;
#45179 = CARTESIAN_POINT ( 'NONE',  ( -17.42409385541300892, -14.80920654474439679, 47.99999999999994316 ) ) ;
#45180 = CARTESIAN_POINT ( 'NONE',  ( -14.41574869888453136, -7.993524183322376686, 63.83332938139840707 ) ) ;
#45181 = VERTEX_POINT ( 'NONE', #14696 ) ;
#45182 = CARTESIAN_POINT ( 'NONE',  ( -24.41553149706675896, -15.71832598455623398, 69.81835354388927328 ) ) ;
#45183 = CARTESIAN_POINT ( 'NONE',  ( -22.59024963249656182, -10.08387628509608192, 73.70990895709888946 ) ) ;
#45184 = ORIENTED_EDGE ( 'NONE', *, *, #38937, .T. ) ;
#45185 = FACE_OUTER_BOUND ( 'NONE', #34096, .T. ) ;
#45186 = PLANE ( 'NONE',  #2883 ) ;
#45187 = CARTESIAN_POINT ( 'NONE',  ( -10.42334078895570926, -15.64104556165006521, 61.18789045260545834 ) ) ;
#45188 = EDGE_LOOP ( 'NONE', ( #22587, #16920, #47315, #22996, #4600 ) ) ;
#45189 = CARTESIAN_POINT ( 'NONE',  ( -14.53659385650551705, -6.915538690918075382, 49.31353937987644542 ) ) ;
#45190 = CARTESIAN_POINT ( 'NONE',  ( -11.46310342473229049, -11.03940158154180651, 61.09374645412970750 ) ) ;
#45191 = DIRECTION ( 'NONE',  ( 0.000000000000000000, -0.9999954153791273948, -0.003028072113819838245 ) ) ;
#45192 = EDGE_CURVE ( 'NONE', #3562, #30487, #16573, .T. ) ;
#45193 = CARTESIAN_POINT ( 'NONE',  ( -14.03870967672415304, -8.172720116890397790, 70.91453050697840865 ) ) ;
#45194 = CARTESIAN_POINT ( 'NONE',  ( -23.19916440516392697, -19.59445054535707698, 53.49999999999994316 ) ) ;
#45195 = ORIENTED_EDGE ( 'NONE', *, *, #20267, .T. ) ;
#45196 = ORIENTED_EDGE ( 'NONE', *, *, #8380, .F. ) ;
#45197 = CARTESIAN_POINT ( 'NONE',  ( -15.69284385650551172, -7.406986770994973490, 48.81910596585309747 ) ) ;
#45198 = CARTESIAN_POINT ( 'NONE',  ( -17.42409385541299471, -14.80920654474435771, 49.52966884056655772 ) ) ;
#45199 = CARTESIAN_POINT ( 'NONE',  ( -16.08659385650551599, -9.302874398569244363, 51.68646062012417985 ) ) ;
#45200 = VECTOR ( 'NONE', #36105, 1000.000000000000114 ) ;
#45201 = CARTESIAN_POINT ( 'NONE',  ( -10.81484442788029376, -17.11524687497682251, 61.45743118925498294 ) ) ;
#45202 = CARTESIAN_POINT ( 'NONE',  ( -10.52668521080748398, -13.31230368787681506, 67.89399308012602319 ) ) ;
#45203 = AXIS2_PLACEMENT_3D ( 'NONE', #3661, #30522, #37375 ) ;
#45204 = EDGE_CURVE ( 'NONE', #20983, #30760, #652, .T. ) ;
#45205 = CARTESIAN_POINT ( 'NONE',  ( -13.85534475943383370, -8.269504983759647487, 74.24308752109034515 ) ) ;
#45206 = CARTESIAN_POINT ( 'NONE',  ( -24.77697371742066679, -16.00871596996390167, 66.10678971410503380 ) ) ;
#45207 = ORIENTED_EDGE ( 'NONE', *, *, #27570, .F. ) ;
#45208 = PLANE ( 'NONE',  #36716 ) ;
#45209 = ORIENTED_EDGE ( 'NONE', *, *, #42837, .F. ) ;
#45210 = ADVANCED_FACE ( 'NONE', ( #41087 ), #22373, .T. ) ;
#45211 = CARTESIAN_POINT ( 'NONE',  ( -12.59088559871646673, -9.139540839424896035, 74.45889665379543487 ) ) ;
#45212 = CARTESIAN_POINT ( 'NONE',  ( -24.72409385541305582, -14.90920654474411577, 58.00588235294116402 ) ) ;
#45213 = DIRECTION ( 'NONE',  ( 0.7700094066334511878, 0.6380325334150290795, 0.000000000000000000 ) ) ;
#45214 = CARTESIAN_POINT ( 'NONE',  ( -18.10866925340710409, -22.22785503003063212, 65.50678672671764957 ) ) ;
#45215 = ORIENTED_EDGE ( 'NONE', *, *, #19245, .F. ) ;
#45216 = B_SPLINE_CURVE_WITH_KNOTS ( 'NONE', 3,
 ( #26291, #33168, #10781, #209 ),
 .UNSPECIFIED., .F., .F.,
 ( 4, 4 ),
 ( 0.000000000000000000, 0.0006999999967409871416 ),
 .UNSPECIFIED. ) ;
#45217 = CARTESIAN_POINT ( 'NONE',  ( -17.71668947275567874, -21.85613660542494685, 62.29024590482070778 ) ) ;
#45218 = CARTESIAN_POINT ( 'NONE',  ( -15.31785298361350378, -21.95540353714732618, 72.16858574460090381 ) ) ;
#45219 =( BOUNDED_SURFACE ( )  B_SPLINE_SURFACE ( 3, 1, ( 
 ( #26940, #20033 ),
 ( #19059, #357 ),
 ( #15341, #30400 ),
 ( #8002, #23019 ),
 ( #39475, #20759 ),
 ( #43667, #17536 ),
 ( #5509, #39712 ) ),
 .UNSPECIFIED., .T., .F., .F. ) 
 B_SPLINE_SURFACE_WITH_KNOTS ( ( 4, 3, 4 ),
 ( 2, 2 ),
 ( 0.000000000000000000, 0.5000000000000000000, 1.000000000000000000 ),
 ( 0.000000000000000000, 1.000000000000000000 ),
 .UNSPECIFIED. ) 
 GEOMETRIC_REPRESENTATION_ITEM ( )  RATIONAL_B_SPLINE_SURFACE ( (
 ( 1.000000000000000000, 1.000000000000000000),
 ( 0.3333333333333335369, 0.3333333333333330373),
 ( 0.3333333333333335369, 0.3333333333333330373),
 ( 1.000000000000000000, 1.000000000000000000),
 ( 0.3333333333333333703, 0.3333333333333333703),
 ( 0.3333333333333333703, 0.3333333333333333703),
 ( 1.000000000000000000, 1.000000000000000000) ) ) 
 REPRESENTATION_ITEM ( '' )  SURFACE ( )  );
#45220 = EDGE_CURVE ( 'NONE', #9377, #20130, #1169, .T. ) ;
#45221 = CARTESIAN_POINT ( 'NONE',  ( -20.13458775212509266, -8.355142810065961712, 70.25100345207583530 ) ) ;
#45222 = FACE_OUTER_BOUND ( 'NONE', #39934, .T. ) ;
#45223 = VERTEX_POINT ( 'NONE', #15696 ) ;
#45224 = CARTESIAN_POINT ( 'NONE',  ( -10.52713468165226374, -17.62616329503903856, 68.20447774248857797 ) ) ;
#45225 = CARTESIAN_POINT ( 'NONE',  ( -19.82409385541304303, -9.359200813967568422, 50.49621490985803263 ) ) ;
#45226 = CARTESIAN_POINT ( 'NONE',  ( -12.65141607933757051, -19.92990444307418230, 65.05778175411948894 ) ) ;
#45227 = FACE_BOUND ( 'NONE', #25157, .T. ) ;
#45228 = APPLICATION_PROTOCOL_DEFINITION ( 'draft international standard', 'automotive_design', 1998, #39119 ) ;
#45229 = ORIENTED_EDGE ( 'NONE', *, *, #37330, .T. ) ;
#45230 = CARTESIAN_POINT ( 'NONE',  ( 18.57132275349405148, 1.979029260061309081, 49.27200896079489922 ) ) ;
#45231 = FACE_OUTER_BOUND ( 'NONE', #29489, .T. ) ;
#45232 = DIRECTION ( 'NONE',  ( 1.000000000000000000, -4.164305804376849172E-17, 1.614929280266638808E-16 ) ) ;
#45233 = CARTESIAN_POINT ( 'NONE',  ( -24.47432067347917695, -14.77756146504815327, 59.52828185648635184 ) ) ;
#45234 = ORIENTED_EDGE ( 'NONE', *, *, #347, .T. ) ;
#45235 = CARTESIAN_POINT ( 'NONE',  ( -19.20714268997449281, -19.15619313305651161, 52.02966884056656482 ) ) ;
#45236 = ORIENTED_EDGE ( 'NONE', *, *, #10810, .T. ) ;
#45237 = CARTESIAN_POINT ( 'NONE',  ( -44.67409385541305511, -14.80920654474410725, 70.50000000000000000 ) ) ;
#45238 = CARTESIAN_POINT ( 'NONE',  ( -23.52949419687348964, -11.28347464189849525, 70.17738639980606763 ) ) ;
#45240 = EDGE_CURVE ( 'NONE', #11480, #30462, #39330, .T. ) ;
#45239 = CARTESIAN_POINT ( 'NONE',  ( -14.92957361138602579, -21.82925975653312278, 65.22101252026929785 ) ) ;
#45241 = ORIENTED_EDGE ( 'NONE', *, *, #5460, .F. ) ;
#45242 = ADVANCED_FACE ( 'NONE', ( #35387 ), #12258, .T. ) ;
#45243 = VECTOR ( 'NONE', #7947, 1000.000000000000000 ) ;
#45244 = CARTESIAN_POINT ( 'NONE',  ( -23.08280660609100110, -10.60377317445056811, 59.61675562601556067 ) ) ;
#45245 = ORIENTED_EDGE ( 'NONE', *, *, #17267, .T. ) ;
#45246 = EDGE_CURVE ( 'NONE', #2100, #48493, #27998, .T. ) ;
#45247 = EDGE_LOOP ( 'NONE', ( #23285, #31950, #34615, #41216 ) ) ;
#45248 = VERTEX_POINT ( 'NONE', #4887 ) ;
#45249 = CARTESIAN_POINT ( 'NONE',  ( -20.38226146016681994, -7.971588334861294811, 70.36604906519886526 ) ) ;
#45250 = CARTESIAN_POINT ( 'NONE',  ( -20.55988796755815073, -8.491641294495202885, 67.19592733635545301 ) ) ;
#45251 = CARTESIAN_POINT ( 'NONE',  ( -19.36787201549275750, -22.00121347418323481, 58.63169058443503445 ) ) ;
#45252 = CARTESIAN_POINT ( 'NONE',  ( -20.75918656682226171, -8.147304802054664563, 63.42626204841099735 ) ) ;
#45253 = CARTESIAN_POINT ( 'NONE',  ( -14.90085577400961014, -10.20532018813695707, 50.77966884056655772 ) ) ;
#45254 = DIRECTION ( 'NONE',  ( -3.071710424422018668E-17, 6.404604876783312462E-16, 1.000000000000000000 ) ) ;
#45255 = CARTESIAN_POINT ( 'NONE',  ( -20.16159385541303095, -7.228003583438104229, 51.38655588711987576 ) ) ;
#45256 = ORIENTED_EDGE ( 'NONE', *, *, #34052, .T. ) ;
#45257 = VERTEX_POINT ( 'NONE', #16670 ) ;
#45258 = CARTESIAN_POINT ( 'NONE',  ( -16.19792114999740562, -7.866354181730329742, 60.48556343814865954 ) ) ;
#45259 = CARTESIAN_POINT ( 'NONE',  ( -13.89449342130350473, -8.248373700058229119, 74.39965851202151725 ) ) ;
#45260 = DIRECTION ( 'NONE',  ( 1.000000000000000000, 0.000000000000000000, 0.000000000000000000 ) ) ;
#45261 = CARTESIAN_POINT ( 'NONE',  ( -36.42409385541304800, -9.359200813967566646, 50.49621490985803263 ) ) ;
#45262 = ORIENTED_EDGE ( 'NONE', *, *, #24334, .T. ) ;
#45263 = CARTESIAN_POINT ( 'NONE',  ( -17.18034385650552309, -6.424090610841176385, 49.80797279389977916 ) ) ;
#45264 = ORIENTED_EDGE ( 'NONE', *, *, #13543, .T. ) ;
#45265 = DIRECTION ( 'NONE',  ( 1.053901171194056067E-05, -6.708308827411335869E-06, 0.9999999999219638669 ) ) ;
#45266 = FACE_OUTER_BOUND ( 'NONE', #27526, .T. ) ;
#45267 =( BOUNDED_CURVE ( )  B_SPLINE_CURVE ( 2, ( #11262, #3882, #7576 ),
 .UNSPECIFIED., .F., .T. ) 
 B_SPLINE_CURVE_WITH_KNOTS ( ( 3, 3 ),
 ( 0.08654929933941044040, 0.08742189555105450705 ),
 .UNSPECIFIED. ) 
 CURVE ( )  GEOMETRIC_REPRESENTATION_ITEM ( )  RATIONAL_B_SPLINE_CURVE ( ( 0.9999999999999626965, 0.9324910878627294952, 0.9847253504145836445 ) ) 
 REPRESENTATION_ITEM ( '' )  );
#45268 = ORIENTED_EDGE ( 'NONE', *, *, #21648, .T. ) ;
#45269 = CARTESIAN_POINT ( 'NONE',  ( -20.37436612178944273, -7.968217454415653656, 70.44438632422075841 ) ) ;
#45270 = VECTOR ( 'NONE', #22968, 1000.000000000000114 ) ;
#45271 = EDGE_CURVE ( 'NONE', #20133, #6106, #18159, .T. ) ;
#45272 = CARTESIAN_POINT ( 'NONE',  ( -14.58503208334058421, -8.356083477664656201, 64.08978844553014653 ) ) ;
#45273 = ADVANCED_FACE ( 'NONE', ( #8576 ), #24787, .T. ) ;
#45274 = ORIENTED_EDGE ( 'NONE', *, *, #6819, .T. ) ;
#45275 = CARTESIAN_POINT ( 'NONE',  ( -24.40658449907488148, -15.78251210865724907, 69.53307488410803217 ) ) ;
#45276 = CARTESIAN_POINT ( 'NONE',  ( -10.45859239952313224, -15.89938452881993847, 64.79299464097340433 ) ) ;
#45277 = DIRECTION ( 'NONE',  ( -4.924618307954601745E-06, -4.007739941247756836E-06, -0.9999999999798431238 ) ) ;
#45278 = ORIENTED_EDGE ( 'NONE', *, *, #16424, .T. ) ;
#45279 = CARTESIAN_POINT ( 'NONE',  ( -24.69683998333984576, -16.42489649515229289, 59.31606561861987359 ) ) ;
#45280 =( BOUNDED_CURVE ( )  B_SPLINE_CURVE ( 3, ( #11840, #8155, #30807, #45335 ),
 .UNSPECIFIED., .F., .F. ) 
 B_SPLINE_CURVE_WITH_KNOTS ( ( 4, 4 ),
 ( 0.4074455897393619574, 0.5000000000000000000 ),
 .UNSPECIFIED. ) 
 CURVE ( )  GEOMETRIC_REPRESENTATION_ITEM ( )  RATIONAL_B_SPLINE_CURVE ( ( 0.6983129098260852929, 0.7760317562606940944, 0.8765941196519998480, 1.000000000000004219 ) ) 
 REPRESENTATION_ITEM ( '' )  );
#45281 = VERTEX_POINT ( 'NONE', #8830 ) ;
#45282 = CARTESIAN_POINT ( 'NONE',  ( -17.72634082312590920, -21.85272461445201486, 58.40553378267872375 ) ) ;
#45283 = CARTESIAN_POINT ( 'NONE',  ( -24.74075702715665770, -16.21285080831185965, 62.77823949964436423 ) ) ;
#45284 = ORIENTED_EDGE ( 'NONE', *, *, #2535, .F. ) ;
#45285 = CARTESIAN_POINT ( 'NONE',  ( -50.42609385541305755, -14.90920654474428630, 74.99999999999998579 ) ) ;
#45286 = CARTESIAN_POINT ( 'NONE',  ( -24.10556926794565413, -12.55028678686139898, 69.65754220287278997 ) ) ;
#45287 = CARTESIAN_POINT ( 'NONE',  ( -12.57408663618378952, -9.687461344359430626, 57.38935503166064933 ) ) ;
#45288 = ORIENTED_EDGE ( 'NONE', *, *, #20909, .F. ) ;
#45289 = FACE_OUTER_BOUND ( 'NONE', #9815, .T. ) ;
#45290 = CARTESIAN_POINT ( 'NONE',  ( -22.31195342450015318, -19.82007762202811918, 65.89524982080033055 ) ) ;
#45291 = CARTESIAN_POINT ( 'NONE',  ( -11.50273595086851763, -11.07590776185467263, 57.20903212540526539 ) ) ;
#45292 = ORIENTED_EDGE ( 'NONE', *, *, #13189, .F. ) ;
#45293 = CARTESIAN_POINT ( 'NONE',  ( -18.47409385541327964, -6.859212275519742441, 50.50378509014038997 ) ) ;
#45294 = ADVANCED_FACE ( 'NONE', ( #43025 ), #23348, .T. ) ;
#45295 = FACE_OUTER_BOUND ( 'NONE', #25001, .T. ) ;
#45296 = EDGE_CURVE ( 'NONE', #16121, #205, #38604, .T. ) ;
#45297 = EDGE_CURVE ( 'NONE', #33361, #45116, #17949, .T. ) ;
#45298 = EDGE_CURVE ( 'NONE', #24853, #14265, #47571, .T. ) ;
#45299 = ORIENTED_EDGE ( 'NONE', *, *, #31847, .T. ) ;
#45300 = VERTEX_POINT ( 'NONE', #38843 ) ;
#45301 = DIRECTION ( 'NONE',  ( 0.000000000000000000, 0.000000000000000000, 1.000000000000000000 ) ) ;
#45302 = DIRECTION ( 'NONE',  ( -2.231660450020913765E-16, -0.9999954153791275058, -0.003028072113822189229 ) ) ;
#45303 = CARTESIAN_POINT ( 'NONE',  ( -23.42626641412206823, -19.22254892098468204, 62.61052823878424078 ) ) ;
#45304 = DIRECTION ( 'NONE',  ( 6.374839753205895344E-22, 0.007114381193220357599, -0.9999746924698832418 ) ) ;
#45305 = CARTESIAN_POINT ( 'NONE',  ( -12.93659385759799285, -8.995762431863214559, 51.38120296130585274 ) ) ;
#45306 = CARTESIAN_POINT ( 'NONE',  ( -12.49878633484568446, -19.78335800357576346, 61.46966759759297361 ) ) ;
#45307 = CARTESIAN_POINT ( 'NONE',  ( -21.02292652713908794, -10.98678540089889921, 49.52966884056655772 ) ) ;
#45308 = VECTOR ( 'NONE', #12777, 1000.000000000000114 ) ;
#45309 = ORIENTED_EDGE ( 'NONE', *, *, #37390, .F. ) ;
#45310 = DIRECTION ( 'NONE',  ( 0.9687793358424819923, -0.2479245821708678243, 0.000000000000000000 ) ) ;
#45311 = CARTESIAN_POINT ( 'NONE',  ( -10.57043792878517685, -13.15679342524445516, 71.20828613024409037 ) ) ;
#45312 = FACE_OUTER_BOUND ( 'NONE', #6533, .T. ) ;
#45313 = ORIENTED_EDGE ( 'NONE', *, *, #31556, .T. ) ;
#45314 = VERTEX_POINT ( 'NONE', #39082 ) ;
#45315 = EDGE_CURVE ( 'NONE', #19053, #30371, #5366, .T. ) ;
#45316 = CARTESIAN_POINT ( 'NONE',  ( -7.540694356433003342, -14.17955609235691661, 53.49999999999995026 ) ) ;
#45317 = PLANE ( 'NONE',  #1694 ) ;
#45318 = B_SPLINE_CURVE_WITH_KNOTS ( 'NONE', 3,
 ( #10203, #33536, #48335, #22245, #18285, #40241, #17799, #40706, #10447, #29628 ),
 .UNSPECIFIED., .F., .F.,
 ( 4, 2, 2, 2, 4 ),
 ( 0.6272669072877586904, 0.7522669073072832946, 0.8772669073268077877, 1.002266907346332392, 1.127266907365856996 ),
 .UNSPECIFIED. ) ;
#45319 = CARTESIAN_POINT ( 'NONE',  ( -19.80886856394220175, -10.13209743873032131, 50.77966884056655772 ) ) ;
#45320 = ORIENTED_EDGE ( 'NONE', *, *, #46494, .F. ) ;
#45321 = CARTESIAN_POINT ( 'NONE',  ( -12.52591726580351228, -9.195683270288645517, 74.50418291613799227 ) ) ;
#45322 = VERTEX_POINT ( 'NONE', #13453 ) ;
#45323 = CARTESIAN_POINT ( 'NONE',  ( -10.35515617550548306, -17.16373074020370737, 61.34398415755805445 ) ) ;
#45324 = EDGE_CURVE ( 'NONE', #41313, #28733, #44606, .T. ) ;
#45325 = CARTESIAN_POINT ( 'NONE',  ( -22.96375064570672819, -10.44813988596692589, 63.08658113699938497 ) ) ;
#45326 = CARTESIAN_POINT ( 'NONE',  ( -12.41315146567207961, -9.850077947585075933, 57.08935532239181754 ) ) ;
#45327 = VERTEX_POINT ( 'NONE', #24575 ) ;
#45328 = FACE_OUTER_BOUND ( 'NONE', #42282, .T. ) ;
#45329 = AXIS2_PLACEMENT_3D ( 'NONE', #27279, #461, #23346 ) ;
#45330 = AXIS2_PLACEMENT_3D ( 'NONE', #29744, #29258, #10545 ) ;
#45331 = ORIENTED_EDGE ( 'NONE', *, *, #15673, .F. ) ;
#45332 = CARTESIAN_POINT ( 'NONE',  ( -10.44632879773527456, -17.41978534048111982, 64.80552118489215729 ) ) ;
#45333 = PLANE ( 'NONE',  #17941 ) ;
#45334 = ORIENTED_EDGE ( 'NONE', *, *, #47526, .T. ) ;
#45335 = CARTESIAN_POINT ( 'NONE',  ( -24.42398663107514523, -15.65075326911586906, 73.01775867260030850 ) ) ;
#45336 = DIRECTION ( 'NONE',  ( -1.616182858256118536E-16, -0.003028072113822188795, 0.9999954153791273948 ) ) ;
#45337 = CARTESIAN_POINT ( 'NONE',  ( -19.29284385650551670, -7.406986770994972602, 48.81910596585309747 ) ) ;
#45338 = CARTESIAN_POINT ( 'NONE',  ( -11.30361347545239958, -11.41219030243732391, 64.14882039658046153 ) ) ;
#45339 = DIRECTION ( 'NONE',  ( 3.827383494395459811E-06, -8.363078745702701817E-06, -0.9999999999577049437 ) ) ;
#45340 = CARTESIAN_POINT ( 'NONE',  ( -12.54253442593986456, -19.82621537833410841, 64.86674886820043184 ) ) ;
#45341 = CARTESIAN_POINT ( 'NONE',  ( -15.28291166272248169, -21.52618791248891128, 68.87592918174580348 ) ) ;
#45342 = ORIENTED_EDGE ( 'NONE', *, *, #24895, .F. ) ;
#45343 = CARTESIAN_POINT ( 'NONE',  ( -10.43288321166496502, -14.45853026220434323, 64.57907052596242181 ) ) ;
#45344 = DIRECTION ( 'NONE',  ( 0.9687793358424817702, -0.2479245821708686570, 0.000000000000000000 ) ) ;
#45345 = DIRECTION ( 'NONE',  ( 2.181982678098338148E-16, 0.000000000000000000, -1.000000000000000000 ) ) ;
#45346 = CARTESIAN_POINT ( 'NONE',  ( -18.64201680114630832, -7.915911148255196039, 70.65602612026023621 ) ) ;
#45347 = CARTESIAN_POINT ( 'NONE',  ( -22.83373948139051990, -9.686860930601344677, 73.58186838660923001 ) ) ;
#45348 = EDGE_CURVE ( 'NONE', #24292, #39358, #41759, .T. ) ;
#45349 = ADVANCED_FACE ( 'NONE', ( #43525 ), #9552, .T. ) ;
#45350 = ORIENTED_EDGE ( 'NONE', *, *, #1036, .F. ) ;
#45351 = ORIENTED_EDGE ( 'NONE', *, *, #48333, .T. ) ;
#45352 = CARTESIAN_POINT ( 'NONE',  ( -24.47354778464749003, -12.39902454472287197, 73.42720984402279782 ) ) ;
#45353 = CARTESIAN_POINT ( 'NONE',  ( -11.93195840498443516, -10.38844327383712773, 70.98365212470247343 ) ) ;
#45354 = EDGE_LOOP ( 'NONE', ( #12976, #15988, #40697, #10480, #42417 ) ) ;
#45355 = CARTESIAN_POINT ( 'NONE',  ( -17.85555652284939043, -7.772123375420258107, 60.09532845646905486 ) ) ;
#45356 = DIRECTION ( 'NONE',  ( 0.1206048672277635625, -0.4306442452895124506, 0.8944271909999158554 ) ) ;
#45357 = CARTESIAN_POINT ( 'NONE',  ( -12.04630953498396018, -19.96521513636629663, 61.55825118588921896 ) ) ;
#45358 = CARTESIAN_POINT ( 'NONE',  ( -50.42609385541305755, -14.90920654474414775, 61.02352941176469869 ) ) ;
#45359 = CARTESIAN_POINT ( 'NONE',  ( -13.44904343725875862, -12.32681728777199304, 52.02966884056656482 ) ) ;
#45360 = EDGE_CURVE ( 'NONE', #1918, #11910, #5225, .T. ) ;
#45361 = EDGE_CURVE ( 'NONE', #12034, #22754, #6326, .T. ) ;
#45362 = LINE ( 'NONE', #8412, #40669 ) ;
#45363 = DIRECTION ( 'NONE',  ( 3.071710424422018668E-17, -6.404604876783312462E-16, -1.000000000000000000 ) ) ;
#45364 = EDGE_CURVE ( 'NONE', #20890, #33252, #33407, .T. ) ;
#45365 = CARTESIAN_POINT ( 'NONE',  ( -16.07865488608826254, -7.939723797651444315, 63.67011030349581091 ) ) ;
#45366 = CARTESIAN_POINT ( 'NONE',  ( -10.99655737938916289, -18.57624151290433900, 57.99209991576458378 ) ) ;
#45367 = ORIENTED_EDGE ( 'NONE', *, *, #26430, .T. ) ;
#45368 = AXIS2_PLACEMENT_3D ( 'NONE', #5716, #20723, #38946 ) ;
#45369 = EDGE_LOOP ( 'NONE', ( #28669, #42265, #27006, #9664 ) ) ;
#45370 = AXIS2_PLACEMENT_3D ( 'NONE', #23520, #15364, #864 ) ;
#45371 = SURFACE_STYLE_USAGE ( .BOTH. , #18769 ) ;
#45372 = EDGE_LOOP ( 'NONE', ( #17806, #20754, #3939, #45446, #1883 ) ) ;
#45373 = ADVANCED_FACE ( 'NONE', ( #24803 ), #28254, .T. ) ;
#45374 = DIRECTION ( 'NONE',  ( -0.3824554607245533866, 0.9239739285077094300, -8.917814418161383551E-09 ) ) ;
#45375 = CARTESIAN_POINT ( 'NONE',  ( -22.58237342315448615, -13.83214364962418053, 50.77966884056655772 ) ) ;
#45376 = AXIS2_PLACEMENT_3D ( 'NONE', #24818, #17157, #1682 ) ;
#45377 = B_SPLINE_CURVE_WITH_KNOTS ( 'NONE', 3,
 ( #46792, #27828, #28327, #9371, #1736, #1232, #1478, #5683, #17212, #20693 ),
 .UNSPECIFIED., .F., .F.,
 ( 4, 2, 2, 2, 4 ),
 ( 0.000000000000000000, 0.2499999999999775180, 0.4999999999999850120, 0.7499999999999924505, 1.000000000000000000 ),
 .UNSPECIFIED. ) ;
#45378 = B_SPLINE_CURVE_WITH_KNOTS ( 'NONE', 3,
 ( #45610, #8175, #45120, #26150, #37946, #4460, #50, #19734, #30097, #14776 ),
 .UNSPECIFIED., .F., .F.,
 ( 4, 2, 2, 2, 4 ),
 ( 0.000000000000000000, 0.2500000000000000000, 0.5000000000000000000, 0.7500000000000000000, 1.000000000000000000 ),
 .UNSPECIFIED. ) ;
#45379 = LINE ( 'NONE', #321, #11161 ) ;
#45380 = CARTESIAN_POINT ( 'NONE',  ( -40.92409385541305511, -15.80920654474410725, 74.99999999999998579 ) ) ;
#45381 = ORIENTED_EDGE ( 'NONE', *, *, #41378, .T. ) ;
#45382 = CARTESIAN_POINT ( 'NONE',  ( -13.53189383941936264, -21.16172133628754892, 65.02982926591782586 ) ) ;
#45383 = CYLINDRICAL_SURFACE ( 'NONE', #14691, 1.250000000000001110 ) ;
#45384 = ORIENTED_EDGE ( 'NONE', *, *, #47454, .F. ) ;
#45385 = LINE ( 'NONE', #15073, #18630 ) ;
#45386 = CARTESIAN_POINT ( 'NONE',  ( -17.42409385541299471, -14.80920654474435771, 49.52966884056655772 ) ) ;
#45387 = VERTEX_POINT ( 'NONE', #43280 ) ;
#45388 = DIRECTION ( 'NONE',  ( 3.413470714839332458E-33, -1.190614954331866791E-16, 1.000000000000000000 ) ) ;
#45389 = DIRECTION ( 'NONE',  ( 0.3163880819683242418, 0.8528035521334692559, 0.4154812667942346938 ) ) ;
#45390 = LINE ( 'NONE', #5002, #1397 ) ;
#45391 = VERTEX_POINT ( 'NONE', #46956 ) ;
#45392 = CARTESIAN_POINT ( 'NONE',  ( -19.74917349865086180, -21.41189893251537413, 68.93482485975984275 ) ) ;
#45393 = DIRECTION ( 'NONE',  ( 3.071710424422018668E-17, -6.404604876783312462E-16, -1.000000000000000000 ) ) ;
#45394 =( BOUNDED_CURVE ( )  B_SPLINE_CURVE ( 3, ( #713, #18424, #30764, #33433 ),
 .UNSPECIFIED., .F., .F. ) 
 B_SPLINE_CURVE_WITH_KNOTS ( ( 4, 4 ),
 ( 0.000000000000000000, 0.4074455897393649551 ),
 .UNSPECIFIED. ) 
 CURVE ( )  GEOMETRIC_REPRESENTATION_ITEM ( )  RATIONAL_B_SPLINE_CURVE ( ( 1.000000000000000000, 0.4567392136813263059, 0.3561768502900282130, 0.6983129098261057210 ) ) 
 REPRESENTATION_ITEM ( '' )  );
#45395 = EDGE_CURVE ( 'NONE', #33399, #31657, #17134, .T. ) ;
#45396 = CARTESIAN_POINT ( 'NONE',  ( -50.42609385541305755, -14.80920654474412679, 59.91176470588234793 ) ) ;
#45397 = CARTESIAN_POINT ( 'NONE',  ( -13.65828898514496359, -20.76952646431350757, 65.00101022825411690 ) ) ;
#45398 = ORIENTED_EDGE ( 'NONE', *, *, #29543, .F. ) ;
#45399 = CARTESIAN_POINT ( 'NONE',  ( -10.61641629527463770, -11.78277212779517136, 74.74335553404092991 ) ) ;
#45400 = CARTESIAN_POINT ( 'NONE',  ( -42.43291738482482600, -14.90920654474415841, 62.92941176470587550 ) ) ;
#45401 = CARTESIAN_POINT ( 'NONE',  ( -10.76011155904975780, -12.66606457907365169, 61.09853557581804750 ) ) ;
#45402 = AXIS2_PLACEMENT_3D ( 'NONE', #25002, #40269, #35823 ) ;
#45403 = AXIS2_PLACEMENT_3D ( 'NONE', #381, #11698, #19323 ) ;
#45404 = CARTESIAN_POINT ( 'NONE',  ( -10.42334091404133645, -15.64104667191196185, 61.33789045260130024 ) ) ;
#45405 = CARTESIAN_POINT ( 'NONE',  ( -20.85319456454439546, -20.91190956734547157, 62.11471372081155096 ) ) ;
#45406 = CARTESIAN_POINT ( 'NONE',  ( -17.42409385541299471, -14.80920654474434883, 62.02966884056656482 ) ) ;
#45407 = CARTESIAN_POINT ( 'NONE',  ( -19.26159385650551670, -9.295667164867525756, 49.30633214617472504 ) ) ;
#45408 = ADVANCED_FACE ( 'NONE', ( #40304 ), #21593, .T. ) ;
#45409 = ORIENTED_EDGE ( 'NONE', *, *, #44966, .T. ) ;
#45410 = CARTESIAN_POINT ( 'NONE',  ( -15.59410181515468530, -19.12364873146921695, 52.02966884056656482 ) ) ;
#45411 = CARTESIAN_POINT ( 'NONE',  ( -17.42409385541299471, -14.80920654474435594, 52.02966884056656482 ) ) ;
#45412 = VERTEX_POINT ( 'NONE', #35860 ) ;
#45413 = CYLINDRICAL_SURFACE ( 'NONE', #22941, 7.500000000000001776 ) ;
#45414 = VECTOR ( 'NONE', #6258, 1000.000000000000000 ) ;
#45415 = CARTESIAN_POINT ( 'NONE',  ( -15.09544287645192462, -21.46351977604527761, 65.10596681500476279 ) ) ;
#45416 = CARTESIAN_POINT ( 'NONE',  ( -24.72409385541305582, -14.90920654474419038, 65.04705882352939739 ) ) ;
#45417 =( BOUNDED_CURVE ( )  B_SPLINE_CURVE ( 3, ( #4261, #41687, #10672, #327 ),
 .UNSPECIFIED., .F., .F. ) 
 B_SPLINE_CURVE_WITH_KNOTS ( ( 4, 4 ),
 ( 0.4074455897393671200, 0.5000000000000000000 ),
 .UNSPECIFIED. ) 
 CURVE ( )  GEOMETRIC_REPRESENTATION_ITEM ( )  RATIONAL_B_SPLINE_CURVE ( ( 0.6983129098260968393, 0.7760317562607000896, 0.8765941196520007361, 0.9999999999999978906 ) ) 
 REPRESENTATION_ITEM ( '' )  );
#45418 = VERTEX_POINT ( 'NONE', #40061 ) ;
#45419 =( BOUNDED_CURVE ( )  B_SPLINE_CURVE ( 3, ( #30129, #86, #45640, #30861 ),
 .UNSPECIFIED., .F., .F. ) 
 B_SPLINE_CURVE_WITH_KNOTS ( ( 4, 4 ),
 ( 0.000000000000000000, 0.4074455897393655657 ),
 .UNSPECIFIED. ) 
 CURVE ( )  GEOMETRIC_REPRESENTATION_ITEM ( )  RATIONAL_B_SPLINE_CURVE ( ( 1.000000000000000000, 0.4567392136813270276, 0.3561768502900284905, 0.6983129098261043888 ) ) 
 REPRESENTATION_ITEM ( '' )  );
#45420 = CARTESIAN_POINT ( 'NONE',  ( -18.24929096724884658, -21.81104555038653103, 68.82986815895560540 ) ) ;
#45421 = CARTESIAN_POINT ( 'NONE',  ( -20.68530789332051256, -8.558680460152096714, 60.13565450698544623 ) ) ;
#45422 = EDGE_CURVE ( 'NONE', #34178, #33339, #42261, .T. ) ;
#45423 = CARTESIAN_POINT ( 'NONE',  ( -41.04982914953070150, -14.80920654474427600, 73.99411764705880046 ) ) ;
#45424 = VERTEX_POINT ( 'NONE', #2139 ) ;
#45425 = CARTESIAN_POINT ( 'NONE',  ( -13.63659385650551847, -6.915538690918075382, 49.31353937987644542 ) ) ;
#45426 = ADVANCED_FACE ( 'NONE', ( #36574 ), #33224, .T. ) ;
#45427 = ADVANCED_FACE ( 'NONE', ( #26014 ), #41032, .T. ) ;
#45428 = LINE ( 'NONE', #42459, #27956 ) ;
#45429 = CARTESIAN_POINT ( 'NONE',  ( -10.88286923018596575, -17.43962093083235843, 68.11193994895104709 ) ) ;
#45430 = CARTESIAN_POINT ( 'NONE',  ( -15.55326400670571196, -7.597850160029695488, 70.65343888371961611 ) ) ;
#45431 = DIRECTION ( 'NONE',  ( 0.000000000000000000, 0.000000000000000000, 1.000000000000000000 ) ) ;
#45432 =( BOUNDED_CURVE ( )  B_SPLINE_CURVE ( 3, ( #23153, #7404, #38386, #27076 ),
 .UNSPECIFIED., .F., .F. ) 
 B_SPLINE_CURVE_WITH_KNOTS ( ( 4, 4 ),
 ( 0.5000000000000000000, 0.9074455897393651771 ),
 .UNSPECIFIED. ) 
 CURVE ( )  GEOMETRIC_REPRESENTATION_ITEM ( )  RATIONAL_B_SPLINE_CURVE ( ( 1.000000000000007772, 0.4567392136813430703, 0.3561768502900289346, 0.6983129098260736356 ) ) 
 REPRESENTATION_ITEM ( '' )  );
#45433 = ORIENTED_EDGE ( 'NONE', *, *, #21881, .F. ) ;
#45434 = ORIENTED_EDGE ( 'NONE', *, *, #17309, .T. ) ;
#45435 = CARTESIAN_POINT ( 'NONE',  ( -15.86159385650551634, -9.295667164867525756, 49.30633214617472504 ) ) ;
#45436 = CARTESIAN_POINT ( 'NONE',  ( -20.31796842471441522, -7.944138697998205600, 70.29454436300783016 ) ) ;
#45437 = FILL_AREA_STYLE ('',( #30179 ) ) ;
#45438 = EDGE_CURVE ( 'NONE', #34125, #19673, #10262, .T. ) ;
#45439 = CARTESIAN_POINT ( 'NONE',  ( -16.70534385650551457, -8.801233750844183135, 48.81488406609782515 ) ) ;
#45440 = VECTOR ( 'NONE', #27752, 1000.000000000000227 ) ;
#45441 = CYLINDRICAL_SURFACE ( 'NONE', #4876, 4.686499999999997002 ) ;
#45442 = CARTESIAN_POINT ( 'NONE',  ( -10.56016083362581703, -13.18709213229180932, 67.62343541709479666 ) ) ;
#45443 = FACE_OUTER_BOUND ( 'NONE', #14924, .T. ) ;
#45444 = VERTEX_POINT ( 'NONE', #33874 ) ;
#45445 = VECTOR ( 'NONE', #40194, 1000.000000000000000 ) ;
#45446 = ORIENTED_EDGE ( 'NONE', *, *, #14345, .T. ) ;
#45447 = CARTESIAN_POINT ( 'NONE',  ( -22.22371030936713510, -9.111184089457765367, 59.90666523727240644 ) ) ;
#45448 = LINE ( 'NONE', #27209, #46229 ) ;
#45449 = DIRECTION ( 'NONE',  ( -3.071710424422018668E-17, 6.404604876783312462E-16, 1.000000000000000000 ) ) ;
#45450 = CARTESIAN_POINT ( 'NONE',  ( -18.12273401612753077, -22.22646211661374593, 65.46036745194116691 ) ) ;
#45451 = ORIENTED_EDGE ( 'NONE', *, *, #7848, .T. ) ;
#45452 = DIRECTION ( 'NONE',  ( 0.3722980621098854748, 0.2477784351981106581, 0.8944271909999157444 ) ) ;
#45453 = CARTESIAN_POINT ( 'NONE',  ( -50.42409385541304800, -27.10920654474410796, 47.99999999999998579 ) ) ;
#45454 = B_SPLINE_CURVE_WITH_KNOTS ( 'NONE', 1,
 ( #43093, #1968 ),
 .UNSPECIFIED., .F., .F.,
 ( 2, 2 ),
 ( 0.000000000000000000, 1.000000000000000000 ),
 .UNSPECIFIED. ) ;
#45455 = EDGE_CURVE ( 'NONE', #40490, #15483, #15558, .T. ) ;
#45456 = CARTESIAN_POINT ( 'NONE',  ( -19.43641843455863238, -7.636073284130151961, 60.06818851049102648 ) ) ;
#45457 = CARTESIAN_POINT ( 'NONE',  ( -19.30271816048872324, -8.014114901043837946, 60.26092997144682073 ) ) ;
#45458 = ORIENTED_EDGE ( 'NONE', *, *, #25159, .F. ) ;
#45459 = CARTESIAN_POINT ( 'NONE',  ( -19.53281124456648854, -21.95454890610320930, 62.19514848487217051 ) ) ;
#45460 = CARTESIAN_POINT ( 'NONE',  ( -17.42409385541305511, -14.80920654474411080, 47.99999999999997868 ) ) ;
#45461 = CARTESIAN_POINT ( 'NONE',  ( -19.71801720247071543, -10.72249662993226060, 49.52966884056655772 ) ) ;
#45462 = FACE_BOUND ( 'NONE', #14403, .T. ) ;
#45463 = APPLICATION_PROTOCOL_DEFINITION ( 'draft international standard', 'automotive_design', 1998, #42294 ) ;
#45464 = EDGE_LOOP ( 'NONE', ( #33469, #18158, #47199, #32404, #4614 ) ) ;
#45465 = DIRECTION ( 'NONE',  ( -3.071710424422018668E-17, 6.404604876783312462E-16, 1.000000000000000000 ) ) ;
#45466 = CARTESIAN_POINT ( 'NONE',  ( -14.98249323814573941, -9.880861343182303358, 54.07175714974879099 ) ) ;
#45467 = CARTESIAN_POINT ( 'NONE',  ( -15.17321550381910988, -21.91105134213339412, 68.67569292545161375 ) ) ;
#45468 = AXIS2_PLACEMENT_3D ( 'NONE', #41200, #11169, #44198 ) ;
#45469 = ORIENTED_EDGE ( 'NONE', *, *, #36048, .F. ) ;
#45470 = CARTESIAN_POINT ( 'NONE',  ( -50.42609385541305755, -14.90920654474417972, 64.04117647058822627 ) ) ;
#45471 = ORIENTED_EDGE ( 'NONE', *, *, #19788, .T. ) ;
#45472 = AXIS2_PLACEMENT_3D ( 'NONE', #40202, #36961, #25651 ) ;
#45473 = DIRECTION ( 'NONE',  ( 1.224646799147353207E-16, 1.000000000000000000, -1.912410701131276611E-32 ) ) ;
#45474 = CARTESIAN_POINT ( 'NONE',  ( -16.71979392375450146, -22.22589398653607873, 68.80286503482692240 ) ) ;
#45475 = CARTESIAN_POINT ( 'NONE',  ( -14.29947512317492730, -8.480563224953527879, 63.94546151666516209 ) ) ;
#45476 = ORIENTED_EDGE ( 'NONE', *, *, #42576, .T. ) ;
#45477 = CIRCLE ( 'NONE', #46278, 2.000000000000001332 ) ;
#45478 = VECTOR ( 'NONE', #6867, 1000.000000000000114 ) ;
#45479 = DIRECTION ( 'NONE',  ( 0.3303050442826436783, -0.9438742382973702716, -3.829623548921168867E-09 ) ) ;
#45480 = ORIENTED_EDGE ( 'NONE', *, *, #30300, .F. ) ;
#45481 = ORIENTED_EDGE ( 'NONE', *, *, #6512, .T. ) ;
#45482 = ORIENTED_EDGE ( 'NONE', *, *, #39329, .T. ) ;
#45483 = CARTESIAN_POINT ( 'NONE',  ( -15.66808075433818992, -21.64011062311675815, 71.93086697972334775 ) ) ;
#45484 = EDGE_CURVE ( 'NONE', #3450, #43669, #37553, .T. ) ;
#45485 = DIRECTION ( 'NONE',  ( 0.2393415023380396911, -0.9709354485539016810, 6.438601123316501445E-08 ) ) ;
#45486 = AXIS2_PLACEMENT_3D ( 'NONE', #44612, #41, #18736 ) ;
#45487 = CARTESIAN_POINT ( 'NONE',  ( -21.27916101436501251, -20.65201899428944898, 69.16336101976946793 ) ) ;
#45488 = EDGE_CURVE ( 'NONE', #26444, #43233, #3815, .T. ) ;
#45489 = DIRECTION ( 'NONE',  ( 1.000000000000000000, -4.164305804376849172E-17, 1.614929280266638808E-16 ) ) ;
#45490 = CARTESIAN_POINT ( 'NONE',  ( -10.37345536002686686, -17.21617726224556932, 61.29709747334221248 ) ) ;
#45491 = CARTESIAN_POINT ( 'NONE',  ( -14.10256296019058198, -8.140532706836228982, 70.84462314181931220 ) ) ;
#45492 = LINE ( 'NONE', #28469, #22053 ) ;
#45493 = VERTEX_POINT ( 'NONE', #7314 ) ;
#45494 = ORIENTED_EDGE ( 'NONE', *, *, #11172, .F. ) ;
#45495 = EDGE_CURVE ( 'NONE', #37274, #16463, #3354, .T. ) ;
#45496 = CARTESIAN_POINT ( 'NONE',  ( -16.16221056564778991, -7.466773990862017207, 60.24382527849350311 ) ) ;
#45497 = CARTESIAN_POINT ( 'NONE',  ( -22.53655473247544805, -20.22829521909097394, 65.88917159596024931 ) ) ;
#45498 = CARTESIAN_POINT ( 'NONE',  ( -10.50393358731724369, -15.87404606333056911, 68.16695003737737579 ) ) ;
#45499 = CARTESIAN_POINT ( 'NONE',  ( -23.45651108574825372, -18.46362474097727002, 69.17883092557275404 ) ) ;
#45500 = ORIENTED_EDGE ( 'NONE', *, *, #25907, .T. ) ;
#45501 = EDGE_CURVE ( 'NONE', #37274, #41647, #35124, .T. ) ;
#45502 = CARTESIAN_POINT ( 'NONE',  ( -16.67409385650551812, -9.792211528768504536, 50.49490371617623197 ) ) ;
#45503 = ADVANCED_FACE ( 'NONE', ( #37815 ), #41512, .T. ) ;
#45504 = ORIENTED_EDGE ( 'NONE', *, *, #3136, .F. ) ;
#45505 = CARTESIAN_POINT ( 'NONE',  ( -10.61330328728660533, -12.98831903967553814, 67.73832347272892207 ) ) ;
#45506 = CARTESIAN_POINT ( 'NONE',  ( -16.92409385541305511, -14.80920654474410547, 52.21286476528345588 ) ) ;
#45507 = AXIS2_PLACEMENT_3D ( 'NONE', #47015, #2854, #42848 ) ;
#45508 = CARTESIAN_POINT ( 'NONE',  ( -12.68381388925888587, -19.95990997655619381, 68.63657438305759229 ) ) ;
#45509 =( BOUNDED_SURFACE ( )  B_SPLINE_SURFACE ( 3, 1, ( 
 ( #30576, #26140 ),
 ( #23418, #30334 ),
 ( #11850, #16003 ),
 ( #33994, #292 ),
 ( #37937, #42128 ),
 ( #11597, #26627 ),
 ( #4701, #4222 ) ),
 .UNSPECIFIED., .T., .F., .F. ) 
 B_SPLINE_SURFACE_WITH_KNOTS ( ( 4, 3, 4 ),
 ( 2, 2 ),
 ( 0.000000000000000000, 0.5000000000000000000, 1.000000000000000000 ),
 ( 0.000000000000000000, 1.000000000000000000 ),
 .UNSPECIFIED. ) 
 GEOMETRIC_REPRESENTATION_ITEM ( )  RATIONAL_B_SPLINE_SURFACE ( (
 ( 1.000000000000000000, 1.000000000000000000),
 ( 0.3333333333333335369, 0.3333333333333330373),
 ( 0.3333333333333335369, 0.3333333333333330373),
 ( 1.000000000000000000, 1.000000000000000000),
 ( 0.3333333333333333703, 0.3333333333333333703),
 ( 0.3333333333333333703, 0.3333333333333333703),
 ( 1.000000000000000000, 1.000000000000000000) ) ) 
 REPRESENTATION_ITEM ( '' )  SURFACE ( )  );
#45510 = CIRCLE ( 'NONE', #15598, 1.250000000000001110 ) ;
#45511 = ORIENTED_EDGE ( 'NONE', *, *, #25894, .F. ) ;
#45512 = FACE_OUTER_BOUND ( 'NONE', #45542, .T. ) ;
#45513 = B_SPLINE_CURVE_WITH_KNOTS ( 'NONE', 1,
 ( #1448, #46533 ),
 .UNSPECIFIED., .F., .F.,
 ( 2, 2 ),
 ( 0.000000000000000000, 1.000000000000000000 ),
 .UNSPECIFIED. ) ;
#45514 = VECTOR ( 'NONE', #22435, 1000.000000000000227 ) ;
#45515 = VECTOR ( 'NONE', #47456, 1000.000000000000114 ) ;
#45516 = CARTESIAN_POINT ( 'NONE',  ( -10.43073328261085386, -14.50439875238632403, 67.85800126138448718 ) ) ;
#45517 = CARTESIAN_POINT ( 'NONE',  ( -16.89979169948162863, -10.14008855580012636, 49.52966884056655772 ) ) ;
#45518 = EDGE_LOOP ( 'NONE', ( #12352, #47667, #48073, #707 ) ) ;
#45519 = VECTOR ( 'NONE', #20016, 1000.000000000000000 ) ;
#45520 = CARTESIAN_POINT ( 'NONE',  ( -13.10965166868813903, -12.97921450448603409, 49.52966884056655772 ) ) ;
#45521 = EDGE_CURVE ( 'NONE', #35971, #4639, #23501, .T. ) ;
#45522 = LINE ( 'NONE', #12738, #14141 ) ;
#45523 = DIRECTION ( 'NONE',  ( -3.071710424422018668E-17, 6.404604876783312462E-16, 1.000000000000000000 ) ) ;
#45524 = ORIENTED_EDGE ( 'NONE', *, *, #43086, .T. ) ;
#45525 = CARTESIAN_POINT ( 'NONE',  ( -23.42409385541304090, -9.359200813967568422, 50.49621490985803263 ) ) ;
#45526 = ORIENTED_EDGE ( 'NONE', *, *, #22857, .T. ) ;
#45527 = FACE_OUTER_BOUND ( 'NONE', #913, .T. ) ;
#45528 = DIRECTION ( 'NONE',  ( -3.071710424422018668E-17, 6.404604876783312462E-16, 1.000000000000000000 ) ) ;
#45529 = ORIENTED_EDGE ( 'NONE', *, *, #38218, .T. ) ;
#45530 = CYLINDRICAL_SURFACE ( 'NONE', #1446, 0.1500000000000006051 ) ;
#45531 = CARTESIAN_POINT ( 'NONE',  ( -14.96223302779666398, -10.63593772014186101, 49.52966884056655772 ) ) ;
#45532 = CYLINDRICAL_SURFACE ( 'NONE', #1380, 0.1500000000000003553 ) ;
#45533 = VERTEX_POINT ( 'NONE', #18600 ) ;
#45534 = CARTESIAN_POINT ( 'NONE',  ( -23.90959958070817848, -11.14304846090580980, 70.04210748470214298 ) ) ;
#45535 = DIRECTION ( 'NONE',  ( -1.522745435920864373E-06, 7.096186240322379876E-06, -0.9999999999736627343 ) ) ;
#45536 = CARTESIAN_POINT ( 'NONE',  ( -11.48064390335815155, -11.11094769457351816, 57.20903159568930363 ) ) ;
#45537 = ORIENTED_EDGE ( 'NONE', *, *, #16213, .F. ) ;
#45538 = EDGE_CURVE ( 'NONE', #25105, #24654, #5401, .T. ) ;
#45539 = FACE_OUTER_BOUND ( 'NONE', #22204, .T. ) ;
#45540 = PLANE ( 'NONE',  #48725 ) ;
#45541 = ORIENTED_EDGE ( 'NONE', *, *, #35898, .T. ) ;
#45542 = EDGE_LOOP ( 'NONE', ( #47193, #32092, #33933, #8519 ) ) ;
#45543 = CARTESIAN_POINT ( 'NONE',  ( -18.40115675053315059, -19.96748611248585448, 52.02966884056656482 ) ) ;
#45544 = DIRECTION ( 'NONE',  ( -0.8875028193683940358, -0.4608022847308269609, 4.020963237607658939E-08 ) ) ;
#45546 = CARTESIAN_POINT ( 'NONE',  ( -23.46741908093438767, -19.16603997859080266, 62.53902161361033052 ) ) ;
#45545 = CIRCLE ( 'NONE', #21138, 1.999999999999999334 ) ;
#45547 = CARTESIAN_POINT ( 'NONE',  ( -21.34284385650552096, -8.811426318492348031, 52.18089403414751359 ) ) ;
#45548 = CARTESIAN_POINT ( 'NONE',  ( -20.38226043987465630, -7.971587899251926679, 70.36605015394232510 ) ) ;
#45549 = DIRECTION ( 'NONE',  ( -0.9501515917649785425, -0.3117883138709295898, 1.594035198720926202E-08 ) ) ;
#45550 = CARTESIAN_POINT ( 'NONE',  ( -12.16409273157858628, -9.533090607804314942, 57.22902139051024051 ) ) ;
#45551 = LINE ( 'NONE', #34192, #8989 ) ;
#45552 = AXIS2_PLACEMENT_3D ( 'NONE', #5943, #2239, #24899 ) ;
#45553 = CARTESIAN_POINT ( 'NONE',  ( -11.01266498513346015, -11.85818215851522339, 67.77431642774575948 ) ) ;
#45554 = EDGE_LOOP ( 'NONE', ( #22268, #4320, #13667, #17057, #212 ) ) ;
#45555 = EDGE_CURVE ( 'NONE', #32237, #26756, #34658, .T. ) ;
#45556 = CARTESIAN_POINT ( 'NONE',  ( -24.39403702774331606, -17.44049340399234893, 69.52844358061491903 ) ) ;
#45557 = EDGE_CURVE ( 'NONE', #19035, #39384, #29459, .T. ) ;
#45558 = AXIS2_PLACEMENT_3D ( 'NONE', #17403, #21111, #13928 ) ;
#45559 = CARTESIAN_POINT ( 'NONE',  ( -10.57990114081760957, -13.11695186304740979, 71.22300718686658172 ) ) ;
#45560 = EDGE_CURVE ( 'NONE', #43276, #31666, #7646, .T. ) ;
#45561 = CARTESIAN_POINT ( 'NONE',  ( -21.92782103781014413, -9.450273908687094604, 60.02171200090587178 ) ) ;
#45562 =( BOUNDED_CURVE ( )  B_SPLINE_CURVE ( 3, ( #12868, #38975, #12633, #27655 ),
 .UNSPECIFIED., .F., .F. ) 
 B_SPLINE_CURVE_WITH_KNOTS ( ( 4, 4 ),
 ( 0.9074455897393682857, 1.000000000000000000 ),
 .UNSPECIFIED. ) 
 CURVE ( )  GEOMETRIC_REPRESENTATION_ITEM ( )  RATIONAL_B_SPLINE_CURVE ( ( 0.6983129098260908441, 0.7760317562606963149, 0.8765941196519994039, 1.000000000000000000 ) ) 
 REPRESENTATION_ITEM ( '' )  );
#45563 = ORIENTED_EDGE ( 'NONE', *, *, #27963, .F. ) ;
#45564 = ORIENTED_EDGE ( 'NONE', *, *, #35114, .T. ) ;
#45565 = CARTESIAN_POINT ( 'NONE',  ( -19.92070420837752565, -21.34886149063710192, 69.13710527445095977 ) ) ;
#45566 = FACE_OUTER_BOUND ( 'NONE', #26209, .T. ) ;
#45567 = CARTESIAN_POINT ( 'NONE',  ( -22.11925914797909343, -9.024813657292067859, 63.30658454184609241 ) ) ;
#45568 = CARTESIAN_POINT ( 'NONE',  ( -15.82259855879412846, -7.533287975791289171, 67.25511890406325222 ) ) ;
#45569 = EDGE_CURVE ( 'NONE', #31211, #24237, #31160, .T. ) ;
#45570 = VERTEX_POINT ( 'NONE', #23061 ) ;
#45571 = B_SPLINE_CURVE_WITH_KNOTS ( 'NONE', 1,
 ( #191, #22839 ),
 .UNSPECIFIED., .F., .F.,
 ( 2, 2 ),
 ( 0.000000000000000000, 1.000000000000000000 ),
 .UNSPECIFIED. ) ;
#45572 =( BOUNDED_SURFACE ( )  B_SPLINE_SURFACE ( 3, 1, ( 
 ( #35799, #16602 ),
 ( #31878, #9486 ),
 ( #39995, #46897 ),
 ( #1841, #28187 ),
 ( #39265, #16838 ),
 ( #36038, #31643 ),
 ( #46664, #24018 ) ),
 .UNSPECIFIED., .T., .F., .F. ) 
 B_SPLINE_SURFACE_WITH_KNOTS ( ( 4, 3, 4 ),
 ( 2, 2 ),
 ( 0.000000000000000000, 0.5000000000000000000, 1.000000000000000000 ),
 ( 0.000000000000000000, 1.000000000000000000 ),
 .UNSPECIFIED. ) 
 GEOMETRIC_REPRESENTATION_ITEM ( )  RATIONAL_B_SPLINE_SURFACE ( (
 ( 1.000000000000000000, 1.000000000000000000),
 ( 0.3333333333333335369, 0.3333333333333330373),
 ( 0.3333333333333335369, 0.3333333333333330373),
 ( 1.000000000000000000, 1.000000000000000000),
 ( 0.3333333333333333703, 0.3333333333333333703),
 ( 0.3333333333333333703, 0.3333333333333333703),
 ( 1.000000000000000000, 1.000000000000000000) ) ) 
 REPRESENTATION_ITEM ( '' )  SURFACE ( )  );
#45573 = ADVANCED_FACE ( 'NONE', ( #26983 ), #35084, .T. ) ;
#45574 = CARTESIAN_POINT ( 'NONE',  ( -12.99758137947571157, -9.386477775907486887, 71.14925353122600882 ) ) ;
#45576 = CARTESIAN_POINT ( 'NONE',  ( 18.57590614458706924, 2.137037847100829335, 51.75577699556788502 ) ) ;
#45575 = B_SPLINE_CURVE_WITH_KNOTS ( 'NONE', 3,
 ( #11457, #6793, #33597, #7535, #21808, #14384, #3338, #7045, #10497, #33112 ),
 .UNSPECIFIED., .F., .F.,
 ( 4, 2, 2, 2, 4 ),
 ( 0.1272669073658425354, 0.2522669073463276179, 0.3772669073268126727, 0.5022669073072977275, 0.6272669072877827823 ),
 .UNSPECIFIED. ) ;
#45577 = EDGE_CURVE ( 'NONE', #29452, #41905, #1084, .T. ) ;
#45578 = EDGE_CURVE ( 'NONE', #26071, #32198, #8120, .T. ) ;
#45579 = VERTEX_POINT ( 'NONE', #27945 ) ;
#45580 = AXIS2_PLACEMENT_3D ( 'NONE', #10639, #33755, #37441 ) ;
#45581 = DIRECTION ( 'NONE',  ( -0.000000000000000000, 0.000000000000000000, 1.000000000000000000 ) ) ;
#45582 = CARTESIAN_POINT ( 'NONE',  ( -22.14599188607209612, -19.97735994708842355, 65.98805141629955529 ) ) ;
#45583 = ORIENTED_EDGE ( 'NONE', *, *, #18831, .T. ) ;
#45584 = CARTESIAN_POINT ( 'NONE',  ( -10.42334066387008207, -15.64104445138816679, 61.03789045260961643 ) ) ;
#45585 = VECTOR ( 'NONE', #46328, 1000.000000000000114 ) ;
#45586 = AXIS2_PLACEMENT_3D ( 'NONE', #1006, #15270, #45344 ) ;
#45587 = ORIENTED_EDGE ( 'NONE', *, *, #9770, .F. ) ;
#45588 = CARTESIAN_POINT ( 'NONE',  ( -17.26784385759799179, -9.357632978295821857, 49.97845033065681974 ) ) ;
#45589 = CYLINDRICAL_SURFACE ( 'NONE', #21064, 0.1499999999999963030 ) ;
#45590 = VERTEX_POINT ( 'NONE', #38788 ) ;
#45591 = CARTESIAN_POINT ( 'NONE',  ( -41.17556444364835500, -14.80920654474426534, 72.98823529411762934 ) ) ;
#45592 = DIRECTION ( 'NONE',  ( -3.071710424422018668E-17, 6.404604876783312462E-16, 1.000000000000000000 ) ) ;
#45593 = CARTESIAN_POINT ( 'NONE',  ( -21.26159385650551314, -9.295667164867525756, 49.30633214617472504 ) ) ;
#45594 = CARTESIAN_POINT ( 'NONE',  ( -17.78823985852933731, -7.818684566706888717, 60.08060768393342954 ) ) ;
#45595 = VECTOR ( 'NONE', #1239, 1000.000000000000114 ) ;
#45596 = CARTESIAN_POINT ( 'NONE',  ( -12.06140467229625912, -20.05244645202335008, 47.99999999999994316 ) ) ;
#45597 = CARTESIAN_POINT ( 'NONE',  ( -22.40450728528633206, -19.80423666046082687, 65.70421711893553152 ) ) ;
#45598 = ORIENTED_EDGE ( 'NONE', *, *, #29572, .T. ) ;
#45599 = CARTESIAN_POINT ( 'NONE',  ( -24.47295431262708476, -15.06807065624729169, 59.33480201725491554 ) ) ;
#45600 = CARTESIAN_POINT ( 'NONE',  ( -12.81450749931373245, -9.474957484202729319, 74.31923006089486705 ) ) ;
#45601 = CARTESIAN_POINT ( 'NONE',  ( -22.58065782673598321, -12.89613362149922438, 53.49999999999995026 ) ) ;
#45602 = CARTESIAN_POINT ( 'NONE',  ( -45.38107656289594161, -12.76354662275040219, 70.13000000000000966 ) ) ;
#45603 = CARTESIAN_POINT ( 'NONE',  ( -22.86572475812252847, -14.01004878893095196, 53.49899999999994549 ) ) ;
#45604 = ADVANCED_FACE ( 'NONE', ( #20078 ), #45721, .T. ) ;
#45605 = EDGE_LOOP ( 'NONE', ( #32016, #20240, #6927, #27578, #7418 ) ) ;
#45606 = EDGE_LOOP ( 'NONE', ( #20436, #46354, #10811, #31284, #33846 ) ) ;
#45607 = CARTESIAN_POINT ( 'NONE',  ( -24.49858526622490373, -12.47342014262311949, 73.42038324740811106 ) ) ;
#45608 = CARTESIAN_POINT ( 'NONE',  ( -24.72409385541305582, -14.80920654474427423, 73.99411764705880046 ) ) ;
#45609 = ORIENTED_EDGE ( 'NONE', *, *, #37736, .F. ) ;
#45610 = CARTESIAN_POINT ( 'NONE',  ( -24.05059659118241555, -17.06519001246171996, 72.88336032079776317 ) ) ;
#45611 = DIRECTION ( 'NONE',  ( 0.8398192074808117358, 0.5428661886195298436, 7.907900705247678986E-08 ) ) ;
#45612 = CARTESIAN_POINT ( 'NONE',  ( -22.66784385759799392, -9.357632978295830739, 49.97845033065684106 ) ) ;
#45613 = PLANE ( 'NONE',  #2220 ) ;
#45614 = CARTESIAN_POINT ( 'NONE',  ( -12.08906526520849489, -20.00921629736058804, 61.59667419651943021 ) ) ;
#45615 = CARTESIAN_POINT ( 'NONE',  ( -11.40656469618873814, -19.20173789643934015, 71.84832430454555663 ) ) ;
#45616 = CARTESIAN_POINT ( 'NONE',  ( -15.61111608319569477, -19.14379616117205885, 49.52966884056656482 ) ) ;
#45617 = LINE ( 'NONE', #19251, #13901 ) ;
#45618 = CARTESIAN_POINT ( 'NONE',  ( -11.55573786329523855, -10.21941616939416342, 71.15388509157428132 ) ) ;
#45619 = EDGE_CURVE ( 'NONE', #33140, #5827, #42008, .T. ) ;
#45620 = AXIS2_PLACEMENT_3D ( 'NONE', #19941, #20672, #743 ) ;
#45621 = DIRECTION ( 'NONE',  ( 3.071710424422018668E-17, -6.404604876783312462E-16, -1.000000000000000000 ) ) ;
#45622 = DIRECTION ( 'NONE',  ( 0.000000000000000000, 0.000000000000000000, 1.000000000000000000 ) ) ;
#45623 = DIRECTION ( 'NONE',  ( -2.866981220435666553E-17, 1.000000000000000000, 1.190614954331866791E-16 ) ) ;
#45624 = CARTESIAN_POINT ( 'NONE',  ( -18.26345899425187369, -22.21252533677388286, 65.45876839498835409 ) ) ;
#45625 = CIRCLE ( 'NONE', #18056, 0.5560000000000009379 ) ;
#45626 = ORIENTED_EDGE ( 'NONE', *, *, #37674, .F. ) ;
#45627 = ORIENTED_EDGE ( 'NONE', *, *, #39529, .T. ) ;
#45628 = CARTESIAN_POINT ( 'NONE',  ( -20.17979545193272273, -21.30158238988698116, 72.28990119599492914 ) ) ;
#45629 = EDGE_LOOP ( 'NONE', ( #29345, #18560 ) ) ;
#45630 = CYLINDRICAL_SURFACE ( 'NONE', #31926, 0.1499999999999992450 ) ;
#45631 = CARTESIAN_POINT ( 'NONE',  ( -16.54715509603413537, -21.75405920933647863, 61.86454047598803641 ) ) ;
#45632 = AXIS2_PLACEMENT_3D ( 'NONE', #40827, #37608, #4154 ) ;
#45633 = CARTESIAN_POINT ( 'NONE',  ( -15.84452207058844486, -7.934630762070933763, 63.67010736139238958 ) ) ;
#45634 = EDGE_CURVE ( 'NONE', #40340, #4523, #20325, .T. ) ;
#45635 = EDGE_CURVE ( 'NONE', #45990, #3943, #46788, .T. ) ;
#45636 = DIRECTION ( 'NONE',  ( 0.1261685609230673022, 0.9920088176193797569, 5.058037262945178882E-08 ) ) ;
#45637 = AXIS2_PLACEMENT_3D ( 'NONE', #2809, #38852, #21306 ) ;
#45638 = ORIENTED_EDGE ( 'NONE', *, *, #10646, .T. ) ;
#45639 = CARTESIAN_POINT ( 'NONE',  ( -18.11889201384288128, -21.82488578508536747, 65.34532159284481168 ) ) ;
#45640 = CARTESIAN_POINT ( 'NONE',  ( -24.16016232491792337, -12.71630861904342069, 66.30246503819121529 ) ) ;
#45641 = ORIENTED_EDGE ( 'NONE', *, *, #6855, .F. ) ;
#45642 = DIRECTION ( 'NONE',  ( 1.000000000000000000, -4.164305804376849788E-17, 1.614929280266638808E-16 ) ) ;
#45643 = CARTESIAN_POINT ( 'NONE',  ( -15.29809632361469873, -21.47854941203162937, 68.57592918283285144 ) ) ;
#45644 = VERTEX_POINT ( 'NONE', #1351 ) ;
#45645 = EDGE_CURVE ( 'NONE', #5827, #40125, #31086, .T. ) ;
#45646 = EDGE_CURVE ( 'NONE', #12097, #25463, #12688, .T. ) ;
#45647 = FACE_OUTER_BOUND ( 'NONE', #423, .T. ) ;
#45648 = CARTESIAN_POINT ( 'NONE',  ( -12.81450527785482407, -9.474959380418823685, 74.61923006088066757 ) ) ;
#45649 = CARTESIAN_POINT ( 'NONE',  ( -12.55198883488284878, -12.25722835735234639, 53.49999999999995026 ) ) ;
#45650 = ORIENTED_EDGE ( 'NONE', *, *, #22170, .T. ) ;
#45651 = CARTESIAN_POINT ( 'NONE',  ( -10.90458911758865312, -11.20383709417547280, 64.34870811186064543 ) ) ;
#45652 = CARTESIAN_POINT ( 'NONE',  ( -15.02405691534179688, -8.340062653448299557, 56.49999999999994316 ) ) ;
#45653 = VECTOR ( 'NONE', #44071, 1000.000000000000114 ) ;
#45654 = AXIS2_PLACEMENT_3D ( 'NONE', #4688, #19710, #46551 ) ;
#45655 = DIRECTION ( 'NONE',  ( 1.000000000000000000, 2.866981220435666553E-17, 0.000000000000000000 ) ) ;
#45656 = PLANE ( 'NONE',  #30018 ) ;
#45657 = VERTEX_POINT ( 'NONE', #27708 ) ;
#45658 = CARTESIAN_POINT ( 'NONE',  ( -17.32409385759798681, -9.359200813967568422, 50.49621490985803263 ) ) ;
#45659 = VECTOR ( 'NONE', #14193, 1000.000000000000000 ) ;
#45660 = DIRECTION ( 'NONE',  ( 2.866981220435666553E-17, -1.000000000000000000, -1.190614954331866791E-16 ) ) ;
#45661 = DIRECTION ( 'NONE',  ( -3.071710424422018668E-17, 6.404604876783312462E-16, 1.000000000000000000 ) ) ;
#45662 = DIRECTION ( 'NONE',  ( 0.9687793358424819923, -0.2479245821708680464, 0.000000000000000000 ) ) ;
#45663 = CARTESIAN_POINT ( 'NONE',  ( -21.00534385650551883, -8.801233750844183135, 48.81488406609782515 ) ) ;
#45664 = EDGE_CURVE ( 'NONE', #30036, #42348, #34847, .T. ) ;
#45665 = EDGE_LOOP ( 'NONE', ( #23547, #7711, #40386, #25088 ) ) ;
#45666 = LINE ( 'NONE', #8713, #40050 ) ;
#45667 = DIRECTION ( 'NONE',  ( -1.000000000000000000, 0.000000000000000000, 0.000000000000000000 ) ) ;
#45668 = VERTEX_POINT ( 'NONE', #23788 ) ;
#45669 = CARTESIAN_POINT ( 'NONE',  ( -15.68502974777997316, -7.977065180327441496, 70.90989839958919561 ) ) ;
#45670 = CARTESIAN_POINT ( 'NONE',  ( -24.72409385541305582, -14.80920654474416764, 63.93529411764704662 ) ) ;
#45671 = EDGE_LOOP ( 'NONE', ( #11880, #28956, #23149, #18311, #4009 ) ) ;
#45672 = PLANE ( 'NONE',  #5049 ) ;
#45673 = CARTESIAN_POINT ( 'NONE',  ( -24.42421125441087071, -14.80070621231813455, 59.24300242292227381 ) ) ;
#45674 = FACE_OUTER_BOUND ( 'NONE', #4306, .T. ) ;
#45675 = ORIENTED_EDGE ( 'NONE', *, *, #23391, .T. ) ;
#45676 = CARTESIAN_POINT ( 'NONE',  ( -14.64909385650551776, -8.104110260919579645, 48.81699501597546487 ) ) ;
#45677 = CARTESIAN_POINT ( 'NONE',  ( -10.77303304197945621, -12.62668734528506853, 61.09853568451838868 ) ) ;
#45678 = CYLINDRICAL_SURFACE ( 'NONE', #30066, 0.1500000000000057676 ) ;
#45679 = CARTESIAN_POINT ( 'NONE',  ( -24.72409385541305582, -14.80920654474424225, 70.97647058823527288 ) ) ;
#45680 = CARTESIAN_POINT ( 'NONE',  ( -23.10699383429526321, -18.89654842981622807, 62.35406835440843309 ) ) ;
#45681 = ORIENTED_EDGE ( 'NONE', *, *, #17524, .F. ) ;
#45682 = ORIENTED_EDGE ( 'NONE', *, *, #13893, .T. ) ;
#45683 = CARTESIAN_POINT ( 'NONE',  ( -23.03034385541304729, -6.857644439848013640, 49.98602051094139398 ) ) ;
#45684 = CARTESIAN_POINT ( 'NONE',  ( -22.94595275489701081, -9.807970174690861853, 70.20452678257210266 ) ) ;
#45685 = AXIS2_PLACEMENT_3D ( 'NONE', #9121, #31765, #16962 ) ;
#45686 = CARTESIAN_POINT ( 'NONE',  ( -24.16575310113231012, -12.74704012323608104, 70.07243002239954421 ) ) ;
#45687 = DIRECTION ( 'NONE',  ( -0.7700094066334506326, -0.6380325334150297456, 6.510647142068518693E-17 ) ) ;
#45688 = AXIS2_PLACEMENT_3D ( 'NONE', #33918, #210, #34154 ) ;
#45689 = PRODUCT ( 'Pin Studded Brass Music Cylinder', 'Pin Studded Brass Music Cylinder', '', ( #30932 ) ) ;
#45690 = CYLINDRICAL_SURFACE ( 'NONE', #15857, 2.000000000000001332 ) ;
#45691 = ADVANCED_FACE ( 'NONE', ( #24029 ), #1605, .T. ) ;
#45692 = CARTESIAN_POINT ( 'NONE',  ( -17.98657259272421172, -21.83703102787368167, 62.16063850355641307 ) ) ;
#45693 = CARTESIAN_POINT ( 'NONE',  ( -13.91545454884148825, -8.237059506355153715, 74.45600559034086530 ) ) ;
#45694 = CARTESIAN_POINT ( 'NONE',  ( -13.73934026678462850, -20.82397421667150894, 61.51646026183723137 ) ) ;
#45695 =( BOUNDED_SURFACE ( )  B_SPLINE_SURFACE ( 3, 1, ( 
 ( #5151, #46755 ),
 ( #46269, #43311 ),
 ( #39598, #12998 ),
 ( #19925, #12526 ),
 ( #28029, #20161 ),
 ( #27551, #43052 ),
 ( #35648, #1930 ) ),
 .UNSPECIFIED., .T., .F., .F. ) 
 B_SPLINE_SURFACE_WITH_KNOTS ( ( 4, 3, 4 ),
 ( 2, 2 ),
 ( 0.000000000000000000, 0.5000000000000000000, 1.000000000000000000 ),
 ( 0.000000000000000000, 1.000000000000000000 ),
 .UNSPECIFIED. ) 
 GEOMETRIC_REPRESENTATION_ITEM ( )  RATIONAL_B_SPLINE_SURFACE ( (
 ( 1.000000000000000000, 1.000000000000000000),
 ( 0.3333333333333335369, 0.3333333333333330373),
 ( 0.3333333333333335369, 0.3333333333333330373),
 ( 1.000000000000000000, 1.000000000000000000),
 ( 0.3333333333333333703, 0.3333333333333333703),
 ( 0.3333333333333333703, 0.3333333333333333703),
 ( 1.000000000000000000, 1.000000000000000000) ) ) 
 REPRESENTATION_ITEM ( '' )  SURFACE ( )  );
#45696 = ORIENTED_EDGE ( 'NONE', *, *, #39962, .T. ) ;
#45697 = CYLINDRICAL_SURFACE ( 'NONE', #12357, 0.1500000000000026867 ) ;
#45698 = ORIENTED_EDGE ( 'NONE', *, *, #2717, .F. ) ;
#45699 = EDGE_CURVE ( 'NONE', #36313, #32331, #9339, .T. ) ;
#45700 = DIRECTION ( 'NONE',  ( -3.071710424422018668E-17, 6.404604876783312462E-16, 1.000000000000000000 ) ) ;
#45701 = CARTESIAN_POINT ( 'NONE',  ( -20.98638901306355820, -20.89730141071840208, 69.35450455931557201 ) ) ;
#45702 = CARTESIAN_POINT ( 'NONE',  ( -12.58002213166789041, -9.148928514680237711, 74.43427606957253317 ) ) ;
#45703 = LINE ( 'NONE', #41498, #13608 ) ;
#45704 = AXIS2_PLACEMENT_3D ( 'NONE', #25392, #45523, #11778 ) ;
#45705 = EDGE_CURVE ( 'NONE', #5535, #40722, #43111, .T. ) ;
#45706 = ORIENTED_EDGE ( 'NONE', *, *, #34258, .F. ) ;
#45707 = CARTESIAN_POINT ( 'NONE',  ( -17.98424483515344718, -22.23819686138322638, 61.91890007431585019 ) ) ;
#45708 = CARTESIAN_POINT ( 'NONE',  ( -14.66315376424047301, -7.889636616332322383, 60.51334572945852130 ) ) ;
#45709 = EDGE_CURVE ( 'NONE', #35450, #3087, #19517, .T. ) ;
#45710 =( BOUNDED_SURFACE ( )  B_SPLINE_SURFACE ( 3, 1, ( 
 ( #25454, #6742 ),
 ( #21757, #38713 ),
 ( #15560, #15814 ),
 ( #35011, #23470 ),
 ( #41933, #30134 ),
 ( #5000, #20009 ),
 ( #38466, #37734 ) ),
 .UNSPECIFIED., .T., .F., .F. ) 
 B_SPLINE_SURFACE_WITH_KNOTS ( ( 4, 3, 4 ),
 ( 2, 2 ),
 ( 0.000000000000000000, 0.5000000000000000000, 1.000000000000000000 ),
 ( 0.000000000000000000, 1.000000000000000000 ),
 .UNSPECIFIED. ) 
 GEOMETRIC_REPRESENTATION_ITEM ( )  RATIONAL_B_SPLINE_SURFACE ( (
 ( 1.000000000000000000, 1.000000000000000000),
 ( 0.3333333333333335369, 0.3333333333333330373),
 ( 0.3333333333333335369, 0.3333333333333330373),
 ( 1.000000000000000000, 1.000000000000000000),
 ( 0.3333333333333333703, 0.3333333333333333703),
 ( 0.3333333333333333703, 0.3333333333333333703),
 ( 1.000000000000000000, 1.000000000000000000) ) ) 
 REPRESENTATION_ITEM ( '' )  SURFACE ( )  );
#45711 = CARTESIAN_POINT ( 'NONE',  ( -10.33699397268960674, -12.51219692611108236, 60.90515267099636532 ) ) ;
#45712 = CARTESIAN_POINT ( 'NONE',  ( -20.88147576600584543, -8.209942340109883219, 60.02620652709861560 ) ) ;
#45713 = EDGE_LOOP ( 'NONE', ( #34708, #6524, #11775, #13895, #16052 ) ) ;
#45714 = CARTESIAN_POINT ( 'NONE',  ( -19.98813040044048606, -21.37641421727040125, 72.40478737316021807 ) ) ;
#45715 = CARTESIAN_POINT ( 'NONE',  ( -17.78683253498428485, -22.25049694173829096, 58.58270294325748750 ) ) ;
#45716 =( BOUNDED_SURFACE ( )  B_SPLINE_SURFACE ( 3, 1, ( 
 ( #26831, #37642 ),
 ( #33444, #37143 ),
 ( #14717, #25842 ),
 ( #40860, #22393 ),
 ( #7638, #3678 ),
 ( #11809, #41108 ),
 ( #29788, #10819 ) ),
 .UNSPECIFIED., .T., .F., .F. ) 
 B_SPLINE_SURFACE_WITH_KNOTS ( ( 4, 3, 4 ),
 ( 2, 2 ),
 ( 0.000000000000000000, 0.5000000000000000000, 1.000000000000000000 ),
 ( 0.000000000000000000, 1.000000000000000000 ),
 .UNSPECIFIED. ) 
 GEOMETRIC_REPRESENTATION_ITEM ( )  RATIONAL_B_SPLINE_SURFACE ( (
 ( 1.000000000000000000, 1.000000000000000000),
 ( 0.3333333333333335369, 0.3333333333333330373),
 ( 0.3333333333333335369, 0.3333333333333330373),
 ( 1.000000000000000000, 1.000000000000000000),
 ( 0.3333333333333333703, 0.3333333333333333703),
 ( 0.3333333333333333703, 0.3333333333333333703),
 ( 1.000000000000000000, 1.000000000000000000) ) ) 
 REPRESENTATION_ITEM ( '' )  SURFACE ( )  );
#45717 = CARTESIAN_POINT ( 'NONE',  ( -24.33163080547450718, -17.59998302563209904, 66.09357240084537466 ) ) ;
#45718 = PRODUCT_CONTEXT ( 'NONE', #15516, 'mechanical' ) ;
#45719 = ORIENTED_EDGE ( 'NONE', *, *, #19122, .F. ) ;
#45720 = VECTOR ( 'NONE', #8361, 1000.000000000000227 ) ;
#45721 = CYLINDRICAL_SURFACE ( 'NONE', #11686, 0.1500000000000037970 ) ;
#45722 = DIRECTION ( 'NONE',  ( 0.3636930986378154040, 0.9315188296557533887, -1.850371886801397658E-09 ) ) ;
#45723 = ADVANCED_FACE ( 'NONE', ( #9966 ), #2087, .T. ) ;
#45724 = DIRECTION ( 'NONE',  ( 1.000000000000000000, 2.866981220435666553E-17, 0.000000000000000000 ) ) ;
#45725 = CIRCLE ( 'NONE', #4827, 2.000000000000000000 ) ;
#45726 = CARTESIAN_POINT ( 'NONE',  ( -10.64577744754535082, -11.71757184301072563, 74.67344733366148546 ) ) ;
#45727 = ORIENTED_EDGE ( 'NONE', *, *, #10028, .T. ) ;
#45728 = CARTESIAN_POINT ( 'NONE',  ( -14.07539681412750809, -8.605278097683306981, 74.49954655214880006 ) ) ;
#45729 = VERTEX_POINT ( 'NONE', #28916 ) ;
#45730 = FACE_OUTER_BOUND ( 'NONE', #12831, .T. ) ;
#45731 = CARTESIAN_POINT ( 'NONE',  ( -13.25597844349469057, -9.183841988267115397, 67.60772729950176085 ) ) ;
#45732 = ORIENTED_EDGE ( 'NONE', *, *, #1294, .T. ) ;
#45733 = VECTOR ( 'NONE', #44975, 1000.000000000000000 ) ;
#45734 =( BOUNDED_CURVE ( )  B_SPLINE_CURVE ( 3, ( #11773, #26791, #929, #41816 ),
 .UNSPECIFIED., .F., .F. ) 
 B_SPLINE_CURVE_WITH_KNOTS ( ( 4, 4 ),
 ( 0.000000000000000000, 0.4074455897393705062 ),
 .UNSPECIFIED. ) 
 CURVE ( )  GEOMETRIC_REPRESENTATION_ITEM ( )  RATIONAL_B_SPLINE_CURVE ( ( 1.000000000000000000, 0.4567392136813268610, 0.3561768502900283795, 0.6983129098261044998 ) ) 
 REPRESENTATION_ITEM ( '' )  );
#45735 = FACE_BOUND ( 'NONE', #19132, .T. ) ;
#45736 = ORIENTED_EDGE ( 'NONE', *, *, #10973, .F. ) ;
#45737 = ORIENTED_EDGE ( 'NONE', *, *, #19290, .T. ) ;
#45738 = EDGE_LOOP ( 'NONE', ( #11964, #16899, #11276, #29712, #29660 ) ) ;
#45739 = LINE ( 'NONE', #23805, #19445 ) ;
#45740 = CARTESIAN_POINT ( 'NONE',  ( -21.77108044372514684, -13.02615771018284541, 49.52966884056655772 ) ) ;
#45741 = CARTESIAN_POINT ( 'NONE',  ( -16.43513463834741728, -22.19403045546258468, 65.41219756188628764 ) ) ;
#45742 = CYLINDRICAL_SURFACE ( 'NONE', #11797, 0.1500000000000009936 ) ;
#45743 = CARTESIAN_POINT ( 'NONE',  ( -11.82668574982945664, -9.892677223491459060, 64.13576029842931803 ) ) ;
#45744 = FACE_OUTER_BOUND ( 'NONE', #8894, .T. ) ;
#45745 = ORIENTED_EDGE ( 'NONE', *, *, #27043, .T. ) ;
#45746 = ORIENTED_EDGE ( 'NONE', *, *, #47131, .T. ) ;
#45747 = CARTESIAN_POINT ( 'NONE',  ( -17.65810221059773610, -7.762793303104815301, 63.56529088875731759 ) ) ;
#45748 = AXIS2_PLACEMENT_3D ( 'NONE', #2378, #35616, #5610 ) ;
#45749 = CARTESIAN_POINT ( 'NONE',  ( -9.990737576226866423, -14.31032742905966337, 64.43157936802064967 ) ) ;
#45750 = CARTESIAN_POINT ( 'NONE',  ( -13.42648243792925555, -12.34047032955235501, 52.02966884056656482 ) ) ;
#45751 = DIRECTION ( 'NONE',  ( -0.8507615431891570879, 0.5255518971808580408, 6.876821558984483597E-08 ) ) ;
#45752 = ORIENTED_EDGE ( 'NONE', *, *, #1986, .T. ) ;
#45753 = EDGE_CURVE ( 'NONE', #34525, #17998, #40169, .T. ) ;
#45754 = CARTESIAN_POINT ( 'NONE',  ( -14.25534385650552238, -7.417179338643134834, 52.18511593390279302 ) ) ;
#45755 = ORIENTED_EDGE ( 'NONE', *, *, #18957, .T. ) ;
#45756 = STYLED_ITEM ( 'NONE', ( #2714 ), #31971 ) ;
#45757 = CARTESIAN_POINT ( 'NONE',  ( -15.74783386771837890, -7.961078896070159061, 70.62461975990308360 ) ) ;
#45758 = ADVANCED_FACE ( 'NONE', ( #39520 ), #23214, .T. ) ;
#45759 = CARTESIAN_POINT ( 'NONE',  ( -12.10599122619147749, -20.02663529450013513, 61.58173959111590534 ) ) ;
#45760 = CARTESIAN_POINT ( 'NONE',  ( -10.47387877723939731, -13.58059689071059495, 57.59258137113961595 ) ) ;
#45761 = VERTEX_POINT ( 'NONE', #39757 ) ;
#45762 = LINE ( 'NONE', #15429, #47669 ) ;
#45763 = CARTESIAN_POINT ( 'NONE',  ( -12.17725024227025621, -10.08844384719822429, 57.24502831558379512 ) ) ;
#45764 = ADVANCED_FACE ( 'NONE', ( #43225 ), #24268, .T. ) ;
#45765 = ORIENTED_EDGE ( 'NONE', *, *, #41925, .T. ) ;
#45766 = AXIS2_PLACEMENT_3D ( 'NONE', #35059, #16339, #2305 ) ;
#45767 = CARTESIAN_POINT ( 'NONE',  ( -11.04141237841800560, -11.93494539390495568, 74.85840195306853673 ) ) ;
#45768 = ADVANCED_FACE ( 'NONE', ( #35808 ), #46909, .T. ) ;
#45769 = CARTESIAN_POINT ( 'NONE',  ( -17.60317953294568127, -7.758478677834707682, 67.43528183898541783 ) ) ;
#45770 = CARTESIAN_POINT ( 'NONE',  ( -17.02409385541305653, -14.80920654474410725, 47.99999999999998579 ) ) ;
#45771 = ORIENTED_EDGE ( 'NONE', *, *, #18789, .T. ) ;
#45772 = DIRECTION ( 'NONE',  ( -1.000000000000000000, 4.164305804376849172E-17, -1.614929280266638808E-16 ) ) ;
#45773 = ORIENTED_EDGE ( 'NONE', *, *, #38662, .T. ) ;
#45774 = CARTESIAN_POINT ( 'NONE',  ( -24.71344798646422802, -16.35160113208834431, 62.77984073303771595 ) ) ;
#45775 = EDGE_CURVE ( 'NONE', #31812, #1447, #4949, .T. ) ;
#45776 = EDGE_LOOP ( 'NONE', ( #41566, #35930 ) ) ;
#45777 = CARTESIAN_POINT ( 'NONE',  ( -24.46479343890040070, -14.44719913075708817, 66.48292729247950206 ) ) ;
#45778 = AXIS2_PLACEMENT_3D ( 'NONE', #15822, #30385, #19284 ) ;
#45779 = DIRECTION ( 'NONE',  ( -3.071710424422018668E-17, 6.404604876783312462E-16, 1.000000000000000000 ) ) ;
#45780 = B_SPLINE_CURVE_WITH_KNOTS ( 'NONE', 3,
 ( #42930, #5512, #20530, #35532, #1806, #13107, #36707, #10645, #14306, #43915 ),
 .UNSPECIFIED., .F., .F.,
 ( 4, 2, 2, 2, 4 ),
 ( 0.6272669072877762320, 0.7522669073072868473, 0.8772669073267975737, 1.002266907346308189, 1.127266907365818804 ),
 .UNSPECIFIED. ) ;
#45781 = ORIENTED_EDGE ( 'NONE', *, *, #34171, .F. ) ;
#45782 = CARTESIAN_POINT ( 'NONE',  ( -21.31800492490012999, -20.62620369199774117, 72.52446429884872714 ) ) ;
#45783 = ADVANCED_FACE ( 'NONE', ( #13872 ), #21622, .T. ) ;
#45784 = CARTESIAN_POINT ( 'NONE',  ( -16.34731059182330526, -7.892077880983075389, 60.21645166852753306 ) ) ;
#45785 = DIRECTION ( 'NONE',  ( -0.9990515194385546360, -0.04354378839186318767, 1.103613758316041215E-08 ) ) ;
#45786 = ORIENTED_EDGE ( 'NONE', *, *, #11731, .F. ) ;
#45787 = DIRECTION ( 'NONE',  ( -0.9410372374137779827, -0.3383029970317210644, -1.029646047569396398E-09 ) ) ;
#45788 = EDGE_LOOP ( 'NONE', ( #8922, #19663, #1519, #24647 ) ) ;
#45789 = ORIENTED_EDGE ( 'NONE', *, *, #40542, .F. ) ;
#45790 = CIRCLE ( 'NONE', #27673, 1.999999999999999112 ) ;
#45791 = CARTESIAN_POINT ( 'NONE',  ( -22.84587788576350675, -10.37951466216800966, 66.61352538834459835 ) ) ;
#45792 = DIRECTION ( 'NONE',  ( 0.9687793358424822143, -0.2479245821708672415, 0.000000000000000000 ) ) ;
#45793 = CARTESIAN_POINT ( 'NONE',  ( -22.29909385650551812, -8.114302828567740988, 52.18300498402516041 ) ) ;
#45794 = DIRECTION ( 'NONE',  ( -3.071710424422018668E-17, 6.404604876783312462E-16, 1.000000000000000000 ) ) ;
#45795 = CARTESIAN_POINT ( 'NONE',  ( -11.51240771850610933, -10.27427218717217627, 71.08237763624090633 ) ) ;
#45796 = CARTESIAN_POINT ( 'NONE',  ( -18.56710112356817532, -7.447357278511908873, 74.03338530932549588 ) ) ;
#45797 = CARTESIAN_POINT ( 'NONE',  ( -12.11393208253047149, -10.17166670693309349, 64.32354556750141228 ) ) ;
#45798 = ORIENTED_EDGE ( 'NONE', *, *, #37544, .T. ) ;
#45799 = EDGE_LOOP ( 'NONE', ( #42353, #43319, #25193, #42229, #46586 ) ) ;
#45800 = CARTESIAN_POINT ( 'NONE',  ( -22.71059208588729561, -10.14448404190931186, 70.02650598627910483 ) ) ;
#45801 = CARTESIAN_POINT ( 'NONE',  ( -10.02816200250604872, -13.91188849819191553, 57.58678490442956388 ) ) ;
#45802 = DIRECTION ( 'NONE',  ( -3.071710424422018668E-17, 6.404604876783312462E-16, 1.000000000000000000 ) ) ;
#45803 = EDGE_CURVE ( 'NONE', #17364, #10113, #20366, .T. ) ;
#45804 = VERTEX_POINT ( 'NONE', #12121 ) ;
#45805 = ORIENTED_EDGE ( 'NONE', *, *, #39896, .F. ) ;
#45806 = LINE ( 'NONE', #19692, #24901 ) ;
#45807 = DIRECTION ( 'NONE',  ( -4.734277553319870270E-07, 1.363385191780837012E-06, 0.9999999999989586108 ) ) ;
#45808 = CARTESIAN_POINT ( 'NONE',  ( -41.03659385541305937, -14.90920654474428630, 74.09999999999998010 ) ) ;
#45809 = CARTESIAN_POINT ( 'NONE',  ( -14.93034385541216480, -6.857644439842304429, 49.98602051094714938 ) ) ;
#45810 = EDGE_LOOP ( 'NONE', ( #48362, #35054, #20976, #8047, #19124 ) ) ;
#45811 = EDGE_CURVE ( 'NONE', #45533, #25725, #39243, .T. ) ;
#45812 = CARTESIAN_POINT ( 'NONE',  ( -27.42409385541305511, -25.10920654474410441, 54.99999999999997868 ) ) ;
#45813 = CYLINDRICAL_SURFACE ( 'NONE', #7079, 1.999999999999999556 ) ;
#45814 = ORIENTED_EDGE ( 'NONE', *, *, #41378, .F. ) ;
#45815 = EDGE_CURVE ( 'NONE', #43494, #7495, #1701, .T. ) ;
#45816 = FACE_OUTER_BOUND ( 'NONE', #31200, .T. ) ;
#45817 = ORIENTED_EDGE ( 'NONE', *, *, #28706, .F. ) ;
#45818 = CYLINDRICAL_SURFACE ( 'NONE', #43283, 1.999999999999994893 ) ;
#45819 = ORIENTED_EDGE ( 'NONE', *, *, #33099, .T. ) ;
#45820 = FACE_OUTER_BOUND ( 'NONE', #46446, .T. ) ;
#45821 = EDGE_CURVE ( 'NONE', #18340, #5003, #42376, .T. ) ;
#45822 = CARTESIAN_POINT ( 'NONE',  ( -19.29992334121955366, -21.55324995122935761, 58.81041981532258944 ) ) ;
#45823 = ORIENTED_EDGE ( 'NONE', *, *, #19436, .T. ) ;
#45824 = CARTESIAN_POINT ( 'NONE',  ( -17.42409385541299471, -14.80920654474435771, 49.52966884056655772 ) ) ;
#45825 = CARTESIAN_POINT ( 'NONE',  ( -24.27033112822875793, -13.12649005559073245, 63.13264177271827293 ) ) ;
#45826 = CARTESIAN_POINT ( 'NONE',  ( -17.49284385650551599, -7.406986770994972602, 48.81910596585309747 ) ) ;
#45827 = CARTESIAN_POINT ( 'NONE',  ( -17.42409385541299471, -14.80920654474435771, 49.52966884056655772 ) ) ;
#45828 = EDGE_CURVE ( 'NONE', #45934, #27520, #23454, .T. ) ;
#45829 = DIRECTION ( 'NONE',  ( -5.731567514496413899E-31, -1.020425574103664789E-16, -1.000000000000000000 ) ) ;
#45830 = CARTESIAN_POINT ( 'NONE',  ( -14.97035482569482312, -21.41873484682592377, 61.92128389535452015 ) ) ;
#45831 = ORIENTED_EDGE ( 'NONE', *, *, #3066, .T. ) ;
#45832 = CARTESIAN_POINT ( 'NONE',  ( -24.72409385541305582, -14.80920654474419962, 66.95294117647057419 ) ) ;
#45833 = CARTESIAN_POINT ( 'NONE',  ( -17.42409385541299471, -14.80920654474435771, 49.52966884056655772 ) ) ;
#45834 = CARTESIAN_POINT ( 'NONE',  ( -15.71784385541289275, -6.860780111191378872, 51.02154966934401159 ) ) ;
#45835 = CARTESIAN_POINT ( 'NONE',  ( -18.34835985623554677, -21.74804277390830975, 68.81514668082158437 ) ) ;
#45836 = CARTESIAN_POINT ( 'NONE',  ( -12.74802523442671465, -20.09592109768945889, 65.02242199588995675 ) ) ;
#45837 = EDGE_LOOP ( 'NONE', ( #15373, #35869, #13553, #4518, #38594 ) ) ;
#45838 = ORIENTED_EDGE ( 'NONE', *, *, #18929, .T. ) ;
#45839 = DIRECTION ( 'NONE',  ( 3.084459863448555673E-06, -5.853393718798201518E-06, 0.9999999999781119531 ) ) ;
#45840 = LINE ( 'NONE', #38677, #46253 ) ;
#45841 = VERTEX_POINT ( 'NONE', #45867 ) ;
#45842 = CARTESIAN_POINT ( 'NONE',  ( -10.42131017383741032, -15.64935787052201910, 57.45304097017945111 ) ) ;
#45843 = CARTESIAN_POINT ( 'NONE',  ( -15.74601971208386786, -7.550529481922165331, 67.26194484337577251 ) ) ;
#45844 = CARTESIAN_POINT ( 'NONE',  ( -20.81159385759798752, -8.990409506049200417, 49.61344411288074951 ) ) ;
#45845 = CARTESIAN_POINT ( 'NONE',  ( -14.81535805098777736, -7.777528402031244958, 75.49999999999994316 ) ) ;
#45846 =( BOUNDED_CURVE ( )  B_SPLINE_CURVE ( 3, ( #39073, #694, #38592, #5114 ),
 .UNSPECIFIED., .F., .F. ) 
 B_SPLINE_CURVE_WITH_KNOTS ( ( 4, 4 ),
 ( 4.712388980384689674, 4.921828490624008623 ),
 .UNSPECIFIED. ) 
 CURVE ( )  GEOMETRIC_REPRESENTATION_ITEM ( )  RATIONAL_B_SPLINE_CURVE ( ( 1.000000000000000000, 0.9963479302455156006, 0.9963479302455156006, 1.000000000000000000 ) ) 
 REPRESENTATION_ITEM ( '' )  );
#45847 = EDGE_CURVE ( 'NONE', #43944, #1710, #34518, .T. ) ;
#45848 = CARTESIAN_POINT ( 'NONE',  ( -14.28769015366465567, -8.051497000463099241, 67.51620991724109899 ) ) ;
#45849 = LINE ( 'NONE', #40919, #17605 ) ;
#45850 = PLANE ( 'NONE',  #9059 ) ;
#45851 = EDGE_CURVE ( 'NONE', #27306, #7306, #9891, .T. ) ;
#45852 = ORIENTED_EDGE ( 'NONE', *, *, #16333, .T. ) ;
#45853 = CARTESIAN_POINT ( 'NONE',  ( -24.39511741622861507, -15.44614315551445571, 73.22977031223102529 ) ) ;
#45854 = EDGE_CURVE ( 'NONE', #41721, #27154, #3058, .T. ) ;
#45855 = SURFACE_STYLE_USAGE ( .BOTH. , #4242 ) ;
#45856 = CARTESIAN_POINT ( 'NONE',  ( -10.63004074901718532, -12.92571453866564823, 67.75304464120749515 ) ) ;
#45857 = CARTESIAN_POINT ( 'NONE',  ( -50.42609385541305755, -14.80920654474426534, 72.08823529411763786 ) ) ;
#45858 = CARTESIAN_POINT ( 'NONE',  ( -15.88655729437939534, -7.980152340574909076, 67.44007279406643818 ) ) ;
#45859 =( BOUNDED_SURFACE ( )  B_SPLINE_SURFACE ( 3, 1, ( 
 ( #32218, #16690 ),
 ( #2414, #47234 ),
 ( #10048, #25721 ),
 ( #5148, #28025 ),
 ( #31730, #46519 ),
 ( #27786, #46752 ),
 ( #12994, #43049 ) ),
 .UNSPECIFIED., .T., .F., .F. ) 
 B_SPLINE_SURFACE_WITH_KNOTS ( ( 4, 3, 4 ),
 ( 2, 2 ),
 ( 0.000000000000000000, 0.5000000000000000000, 1.000000000000000000 ),
 ( 0.000000000000000000, 1.000000000000000000 ),
 .UNSPECIFIED. ) 
 GEOMETRIC_REPRESENTATION_ITEM ( )  RATIONAL_B_SPLINE_SURFACE ( (
 ( 1.000000000000000000, 1.000000000000000000),
 ( 0.3333333333333335369, 0.3333333333333330373),
 ( 0.3333333333333335369, 0.3333333333333330373),
 ( 1.000000000000000000, 1.000000000000000000),
 ( 0.3333333333333333703, 0.3333333333333333703),
 ( 0.3333333333333333703, 0.3333333333333333703),
 ( 1.000000000000000000, 1.000000000000000000) ) ) 
 REPRESENTATION_ITEM ( '' )  SURFACE ( )  );
#45860 = VERTEX_POINT ( 'NONE', #27626 ) ;
#45861 = ORIENTED_EDGE ( 'NONE', *, *, #25640, .F. ) ;
#45862 = FACE_OUTER_BOUND ( 'NONE', #13216, .T. ) ;
#45863 = ORIENTED_EDGE ( 'NONE', *, *, #12060, .T. ) ;
#45864 = CARTESIAN_POINT ( 'NONE',  ( -11.21783104652298846, -18.93062367394879431, 64.93202350587574756 ) ) ;
#45865 = DIRECTION ( 'NONE',  ( -3.071710424422018668E-17, 6.404604876783312462E-16, 1.000000000000000000 ) ) ;
#45866 = ORIENTED_EDGE ( 'NONE', *, *, #26341, .T. ) ;
#45867 = CARTESIAN_POINT ( 'NONE',  ( -10.40888626530166405, -14.10966241957602385, 60.91821293886854249 ) ) ;
#45868 = CARTESIAN_POINT ( 'NONE',  ( -13.61216655543990584, -20.68217103177308047, 65.09702080378529843 ) ) ;
#45869 = CARTESIAN_POINT ( 'NONE',  ( -16.91855125566938511, -22.24212016642244905, 72.28047911973106920 ) ) ;
#45870 = VECTOR ( 'NONE', #44665, 1000.000000000000000 ) ;
#45871 = ORIENTED_EDGE ( 'NONE', *, *, #33839, .F. ) ;
#45872 = CARTESIAN_POINT ( 'NONE',  ( -20.90293659130012216, -8.221317335593040454, 60.04114024615370937 ) ) ;
#45873 = DIRECTION ( 'NONE',  ( 0.8467008005855419794, -0.3141239757129650201, 0.4294460177601872597 ) ) ;
#45874 = ORIENTED_EDGE ( 'NONE', *, *, #18454, .T. ) ;
#45875 = DIRECTION ( 'NONE',  ( -3.071710424422018668E-17, 6.404604876783312462E-16, 1.000000000000000000 ) ) ;
#45876 = CARTESIAN_POINT ( 'NONE',  ( -23.93244369146852080, -17.39065619829227671, 69.60266770082890275 ) ) ;
#45877 = VERTEX_POINT ( 'NONE', #46098 ) ;
#45878 = FACE_OUTER_BOUND ( 'NONE', #17700, .T. ) ;
#45879 = CARTESIAN_POINT ( 'NONE',  ( -22.20824715029565866, -20.52011977224520223, 58.86419268801586924 ) ) ;
#45880 = EDGE_CURVE ( 'NONE', #21727, #40683, #17976, .T. ) ;
#45881 = CARTESIAN_POINT ( 'NONE',  ( -24.00920687666620168, -12.43512006407420145, 73.35111597096941694 ) ) ;
#45882 = VERTEX_POINT ( 'NONE', #24179 ) ;
#45883 = CARTESIAN_POINT ( 'NONE',  ( -23.25280541480605834, -10.16922674724575693, 63.17911852083285851 ) ) ;
#45884 = CARTESIAN_POINT ( 'NONE',  ( -17.80126953765676845, -21.79909748901075517, 58.42055855158453426 ) ) ;
#45885 = CARTESIAN_POINT ( 'NONE',  ( -23.58616520728616806, -18.99640775243969060, 66.00884813586510802 ) ) ;
#45886 = DIRECTION ( 'NONE',  ( 1.000000000000000000, 0.000000000000000000, 0.000000000000000000 ) ) ;
#45887 = CARTESIAN_POINT ( 'NONE',  ( -24.36621887139804699, -13.91093020482227693, 73.31374677385069560 ) ) ;
#45888 = CARTESIAN_POINT ( 'NONE',  ( -10.42052617248403124, -15.61735782369945547, 61.03789063027900141 ) ) ;
#45889 = CYLINDRICAL_SURFACE ( 'NONE', #36778, 0.1499999999999963585 ) ;
#45890 = CARTESIAN_POINT ( 'NONE',  ( -24.25171713147202368, -16.35308467727669068, 59.12332432120680181 ) ) ;
#45891 = CARTESIAN_POINT ( 'NONE',  ( -14.90981300391230846, -21.39562377109201208, 61.63600440604547970 ) ) ;
#45892 = CARTESIAN_POINT ( 'NONE',  ( -14.98659385650551457, -9.302874398569244363, 51.68646062012417985 ) ) ;
#45893 = ORIENTED_EDGE ( 'NONE', *, *, #46915, .T. ) ;
#45894 = CARTESIAN_POINT ( 'NONE',  ( -19.38197731428664028, -19.06713733463150007, 49.52966884056656482 ) ) ;
#45895 = CARTESIAN_POINT ( 'NONE',  ( -10.47936380272204104, -17.50656370757942781, 64.78772765493845043 ) ) ;
#45896 = ORIENTED_EDGE ( 'NONE', *, *, #18900, .F. ) ;
#45897 = CARTESIAN_POINT ( 'NONE',  ( -16.17793336889135603, -22.15441545345155205, 58.44618891099874958 ) ) ;
#45898 = CARTESIAN_POINT ( 'NONE',  ( -19.37409385541300111, -6.859212275519753099, 50.50378509014300477 ) ) ;
#45899 = LINE ( 'NONE', #4776, #36775 ) ;
#45900 = ORIENTED_EDGE ( 'NONE', *, *, #21553, .T. ) ;
#45901 = CARTESIAN_POINT ( 'NONE',  ( -23.65624121974494898, -11.51332442490695307, 66.42214514605623776 ) ) ;
#45902 = EDGE_CURVE ( 'NONE', #38928, #42512, #39182, .T. ) ;
#45903 = DIRECTION ( 'NONE',  ( -1.224646799147353207E-16, -1.000000000000000000, 1.912410701131276611E-32 ) ) ;
#45904 = CARTESIAN_POINT ( 'NONE',  ( -23.51785719624223958, -11.36449344406884343, 70.19210750610864125 ) ) ;
#45905 = EDGE_CURVE ( 'NONE', #34665, #7279, #7545, .T. ) ;
#45906 = EDGE_CURVE ( 'NONE', #29749, #4669, #48355, .T. ) ;
#45907 = ORIENTED_EDGE ( 'NONE', *, *, #26113, .F. ) ;
#45908 = CIRCLE ( 'NONE', #24670, 1.999999999999999778 ) ;
#45909 = CARTESIAN_POINT ( 'NONE',  ( -13.29699920919266631, -9.093425021029217348, 63.90946558901772079 ) ) ;
#45910 = CARTESIAN_POINT ( 'NONE',  ( -24.39403702774331606, -17.44049340399234893, 69.52844358061491903 ) ) ;
#45911 = CARTESIAN_POINT ( 'NONE',  ( -24.55620591900586902, -12.65601924842659720, 69.96581314741867175 ) ) ;
#45912 = CARTESIAN_POINT ( 'NONE',  ( -23.23616624490289340, -18.79948399208958776, 66.12389430041484673 ) ) ;
#45913 = CARTESIAN_POINT ( 'NONE',  ( -10.84300597751149553, -17.34773470226564029, 61.15743043792785016 ) ) ;
#45914 = ORIENTED_EDGE ( 'NONE', *, *, #35322, .T. ) ;
#45915 = ORIENTED_EDGE ( 'NONE', *, *, #44515, .T. ) ;
#45916 = CARTESIAN_POINT ( 'NONE',  ( -21.45534385541304445, -8.623186033802570094, 49.24843789510466507 ) ) ;
#45917 = CARTESIAN_POINT ( 'NONE',  ( -11.93102662126159785, -10.47028825497329585, 70.96893105764984000 ) ) ;
#45918 = CARTESIAN_POINT ( 'NONE',  ( -24.15877587438482976, -12.72423012542946807, 70.07242983926148838 ) ) ;
#45919 = CARTESIAN_POINT ( 'NONE',  ( -18.52416312356643147, -7.896186446804856374, 73.84064402154488960 ) ) ;
#45920 = FACE_OUTER_BOUND ( 'NONE', #40565, .T. ) ;
#45921 = EDGE_CURVE ( 'NONE', #7173, #10403, #39913, .T. ) ;
#45922 = CARTESIAN_POINT ( 'NONE',  ( -12.77796340496265692, -17.75258416873320400, 54.07175714974880520 ) ) ;
#45923 = FACE_OUTER_BOUND ( 'NONE', #34183, .T. ) ;
#45924 = VERTEX_POINT ( 'NONE', #21207 ) ;
#45925 = CARTESIAN_POINT ( 'NONE',  ( -24.32852063849251323, -13.38246526728995001, 59.37740068604990995 ) ) ;
#45926 = B_SPLINE_CURVE_WITH_KNOTS ( 'NONE', 1,
 ( #8628, #27326 ),
 .UNSPECIFIED., .F., .F.,
 ( 2, 2 ),
 ( 0.000000000000000000, 1.000000000000000000 ),
 .UNSPECIFIED. ) ;
#45927 = VECTOR ( 'NONE', #30943, 1000.000000000000000 ) ;
#45928 = EDGE_LOOP ( 'NONE', ( #43707, #26727, #14003, #27997, #36034 ) ) ;
#45929 = CARTESIAN_POINT ( 'NONE',  ( -22.96481576609224717, -19.16891988936071556, 58.89882756593014790 ) ) ;
#45930 = LINE ( 'NONE', #1104, #25003 ) ;
#45931 = VERTEX_POINT ( 'NONE', #20721 ) ;
#45932 = CARTESIAN_POINT ( 'NONE',  ( -13.24261801534493088, -8.643248549050911222, 60.55454889300790455 ) ) ;
#45933 = CIRCLE ( 'NONE', #24716, 4.686499999999999666 ) ;
#45934 = VERTEX_POINT ( 'NONE', #17493 ) ;
#45935 = DIRECTION ( 'NONE',  ( 0.9271861211590526342, 0.3746009833543293421, -1.005599061620490611E-08 ) ) ;
#45936 = ADVANCED_FACE ( 'NONE', ( #48027 ), #17964, .F. ) ;
#45937 = CARTESIAN_POINT ( 'NONE',  ( -10.39693166811831304, -15.37990016280386740, 57.58264896457095006 ) ) ;
#45938 = CARTESIAN_POINT ( 'NONE',  ( -20.94465790601859467, -8.243431112063134947, 59.95629843672877257 ) ) ;
#45939 = ORIENTED_EDGE ( 'NONE', *, *, #21406, .F. ) ;
#45940 = CARTESIAN_POINT ( 'NONE',  ( -21.79028809537168243, -9.273590339475653366, 63.47681654923867711 ) ) ;
#45941 = FACE_OUTER_BOUND ( 'NONE', #45799, .T. ) ;
#45942 = CARTESIAN_POINT ( 'NONE',  ( -46.29409385541305255, -12.70920654474410760, 69.20000000000001705 ) ) ;
#45943 = FACE_BOUND ( 'NONE', #26490, .T. ) ;
#45944 = SHAPE_DEFINITION_REPRESENTATION ( #34663, #2486 ) ;
#45945 = CARTESIAN_POINT ( 'NONE',  ( -11.36794959886231915, -18.31963617796164812, 57.80714594517343841 ) ) ;
#45946 = CARTESIAN_POINT ( 'NONE',  ( -19.98813035779708969, -21.37641423362171267, 72.55478737316022375 ) ) ;
#45947 = DIRECTION ( 'NONE',  ( -0.9584484254710481377, -0.2852658684667118139, 3.516456354099036190E-08 ) ) ;
#45948 = ORIENTED_EDGE ( 'NONE', *, *, #43023, .F. ) ;
#45949 = PLANE ( 'NONE',  #10309 ) ;
#45950 = VERTEX_POINT ( 'NONE', #29313 ) ;
#45951 = CARTESIAN_POINT ( 'NONE',  ( -11.95727733380162050, -19.27338395605723420, 71.84252737392968413 ) ) ;
#45952 = CARTESIAN_POINT ( 'NONE',  ( -22.90877043182983286, -10.45950943414446854, 63.37186031185718349 ) ) ;
#45953 = ORIENTED_EDGE ( 'NONE', *, *, #36235, .F. ) ;
#45954 = CARTESIAN_POINT ( 'NONE',  ( -24.32852063849251323, -13.38246526728995001, 59.37740068604990995 ) ) ;
#45955 = FACE_BOUND ( 'NONE', #23278, .T. ) ;
#45956 = VERTEX_POINT ( 'NONE', #32983 ) ;
#45957 = EDGE_CURVE ( 'NONE', #40380, #2617, #28533, .T. ) ;
#45958 = ORIENTED_EDGE ( 'NONE', *, *, #38080, .T. ) ;
#45959 = ORIENTED_EDGE ( 'NONE', *, *, #26194, .F. ) ;
#45960 = CARTESIAN_POINT ( 'NONE',  ( -17.71668947275567874, -21.85613660542494685, 62.29024590482070778 ) ) ;
#45961 = CARTESIAN_POINT ( 'NONE',  ( -13.73970969606274473, -20.76112332560825990, 65.28628881671112083 ) ) ;
#45962 = CARTESIAN_POINT ( 'NONE',  ( -16.08659385759798965, -7.222650657624104298, 49.61879703869476543 ) ) ;
#45963 = CARTESIAN_POINT ( 'NONE',  ( -14.51896086823277443, -8.440036041935664812, 67.27591678782368945 ) ) ;
#45964 = CARTESIAN_POINT ( 'NONE',  ( -19.28939461086542906, -8.062307027802660286, 60.26092997386343342 ) ) ;
#45965 = VERTEX_POINT ( 'NONE', #43384 ) ;
#45966 = ORIENTED_EDGE ( 'NONE', *, *, #45699, .F. ) ;
#45967 = CIRCLE ( 'NONE', #3489, 2.500000000000002220 ) ;
#45968 = EDGE_CURVE ( 'NONE', #26266, #17919, #22734, .T. ) ;
#45969 = EDGE_CURVE ( 'NONE', #18851, #1251, #10120, .T. ) ;
#45970 = CARTESIAN_POINT ( 'NONE',  ( -23.11784385650551954, -9.790100578890868377, 49.79778022625162492 ) ) ;
#45971 = CIRCLE ( 'NONE', #8996, 4.686499999999998778 ) ;
#45972 = EDGE_CURVE ( 'NONE', #8735, #26020, #12243, .T. ) ;
#45973 = CARTESIAN_POINT ( 'NONE',  ( -11.82605070163061534, -9.893394921550459742, 64.22188489775784603 ) ) ;
#45974 = PLANE ( 'NONE',  #31509 ) ;
#45975 = CARTESIAN_POINT ( 'NONE',  ( -19.63985863958091116, -21.44939509270802702, 65.76486191116302393 ) ) ;
#45976 = EDGE_CURVE ( 'NONE', #39245, #12574, #29071, .T. ) ;
#45977 = VERTEX_POINT ( 'NONE', #24430 ) ;
#45978 =( BOUNDED_CURVE ( )  B_SPLINE_CURVE ( 3, ( #2168, #47958, #6107, #3135 ),
 .UNSPECIFIED., .F., .F. ) 
 B_SPLINE_CURVE_WITH_KNOTS ( ( 4, 4 ),
 ( 0.000000000000000000, 0.4074455897393572390 ),
 .UNSPECIFIED. ) 
 CURVE ( )  GEOMETRIC_REPRESENTATION_ITEM ( )  RATIONAL_B_SPLINE_CURVE ( ( 1.000000000000000000, 0.4567392136813397396, 0.3561768502900331534, 0.6983129098260801859 ) ) 
 REPRESENTATION_ITEM ( '' )  );
#45979 = CARTESIAN_POINT ( 'NONE',  ( -20.75534385650551528, -7.417179338643134834, 52.18511593390279302 ) ) ;
#45980 = ORIENTED_EDGE ( 'NONE', *, *, #42518, .F. ) ;
#45981 = CARTESIAN_POINT ( 'NONE',  ( -16.16816684335524457, -21.69572884791061540, 58.58585623285081567 ) ) ;
#45982 = EDGE_CURVE ( 'NONE', #2125, #35489, #25845, .T. ) ;
#45983 = CARTESIAN_POINT ( 'NONE',  ( -24.46043589294705001, -17.25765543095130639, 73.02302651788181720 ) ) ;
#45984 = ORIENTED_EDGE ( 'NONE', *, *, #34909, .T. ) ;
#45985 = B_SPLINE_CURVE_WITH_KNOTS ( 'NONE', 3,
 ( #47343, #1790, #31339, #17274, #5496, #43156, #46617, #28385, #39458, #32321 ),
 .UNSPECIFIED., .F., .F.,
 ( 4, 2, 2, 2, 4 ),
 ( 0.000000000000000000, 0.2500000000000000000, 0.5000000000000000000, 0.7500000000000000000, 1.000000000000000000 ),
 .UNSPECIFIED. ) ;
#45986 = CYLINDRICAL_SURFACE ( 'NONE', #4485, 4.686499999999997002 ) ;
#45987 =( BOUNDED_CURVE ( )  B_SPLINE_CURVE ( 3, ( #43677, #9930, #24949, #36258 ),
 .UNSPECIFIED., .F., .F. ) 
 B_SPLINE_CURVE_WITH_KNOTS ( ( 4, 4 ),
 ( 0.9074455897393653991, 1.000000000000000000 ),
 .UNSPECIFIED. ) 
 CURVE ( )  GEOMETRIC_REPRESENTATION_ITEM ( )  RATIONAL_B_SPLINE_CURVE ( ( 0.6983129098261022794, 0.7760317562607061959, 0.8765941196520053991, 1.000000000000000000 ) ) 
 REPRESENTATION_ITEM ( '' )  );
#45988 = CARTESIAN_POINT ( 'NONE',  ( -10.42579980212244983, -14.65467349332582714, 68.04903362315590698 ) ) ;
#45989 = LINE ( 'NONE', #12246, #16094 ) ;
#45990 = VERTEX_POINT ( 'NONE', #35719 ) ;
#45991 = CARTESIAN_POINT ( 'NONE',  ( -14.67111564601650997, -7.886426081561471513, 60.43500846974642116 ) ) ;
#45992 = FACE_OUTER_BOUND ( 'NONE', #4449, .T. ) ;
#45993 = DIRECTION ( 'NONE',  ( 0.000000000000000000, 1.000000000000000000, -0.000000000000000000 ) ) ;
#45994 = ORIENTED_EDGE ( 'NONE', *, *, #1154, .T. ) ;
#45995 = CARTESIAN_POINT ( 'NONE',  ( -16.04111743724699224, -7.488525900945328218, 63.83157579393176917 ) ) ;
#45996 =( BOUNDED_CURVE ( )  B_SPLINE_CURVE ( 3, ( #11050, #26073, #41085, #44309 ),
 .UNSPECIFIED., .F., .F. ) 
 B_SPLINE_CURVE_WITH_KNOTS ( ( 4, 4 ),
 ( 0.9074455897393604031, 1.000000000000000000 ),
 .UNSPECIFIED. ) 
 CURVE ( )  GEOMETRIC_REPRESENTATION_ITEM ( )  RATIONAL_B_SPLINE_CURVE ( ( 0.6983129098260856260, 0.7760317562606918740, 0.8765941196519966283, 1.000000000000000000 ) ) 
 REPRESENTATION_ITEM ( '' )  );
#45997 = ORIENTED_EDGE ( 'NONE', *, *, #28242, .T. ) ;
#45998 = VECTOR ( 'NONE', #34432, 1000.000000000000000 ) ;
#45999 = CARTESIAN_POINT ( 'NONE',  ( -9.974456273375457371, -14.72748566909688073, 71.51278126739182994 ) ) ;
#46000 = CARTESIAN_POINT ( 'NONE',  ( -23.77487038158592014, -11.74745262826995429, 62.96690348473899235 ) ) ;
#46001 = ORIENTED_EDGE ( 'NONE', *, *, #34953, .T. ) ;
#46002 = CARTESIAN_POINT ( 'NONE',  ( -18.57089378905319421, -22.17041224548506406, 72.43510938007564448 ) ) ;
#46003 = CARTESIAN_POINT ( 'NONE',  ( -11.02242957576233451, -11.85532881267382166, 74.57312195644870201 ) ) ;
#46004 = CIRCLE ( 'NONE', #2747, 2.000000000000000000 ) ;
#46005 = CARTESIAN_POINT ( 'NONE',  ( -16.19814190158817269, -21.75179548504963023, 58.43585572027992470 ) ) ;
#46006 = EDGE_LOOP ( 'NONE', ( #1960, #43802 ) ) ;
#46007 = CARTESIAN_POINT ( 'NONE',  ( -9.996765541055841808, -14.22627829241283770, 64.52770499853964736 ) ) ;
#46008 = UNCERTAINTY_MEASURE_WITH_UNIT (LENGTH_MEASURE( 1.000000000000000082E-05 ), #31734, 'distance_accuracy_value', 'NONE');
#46009 = CARTESIAN_POINT ( 'NONE',  ( -15.11368083008136587, -21.89207339945041753, 68.71559548072659140 ) ) ;
#46010 = ADVANCED_FACE ( 'NONE', ( #16995 ), #32044, .T. ) ;
#46011 = CARTESIAN_POINT ( 'NONE',  ( -19.63868610202945675, -21.50238589859430149, 65.76486200656573544 ) ) ;
#46012 = CARTESIAN_POINT ( 'NONE',  ( -11.07857809310684338, -11.73724795245126273, 71.38860870961248395 ) ) ;
#46013 = ORIENTED_EDGE ( 'NONE', *, *, #35841, .F. ) ;
#46014 = CARTESIAN_POINT ( 'NONE',  ( -15.82259747647940173, -7.533288219471245384, 67.25511999279136433 ) ) ;
#46015 = CARTESIAN_POINT ( 'NONE',  ( -11.31808814922340822, -18.33929587155208552, 61.69199689979424051 ) ) ;
#46016 = EDGE_CURVE ( 'NONE', #34094, #25136, #7801, .T. ) ;
#46017 = ORIENTED_EDGE ( 'NONE', *, *, #48609, .F. ) ;
#46018 = ORIENTED_EDGE ( 'NONE', *, *, #41035, .F. ) ;
#46019 = DIRECTION ( 'NONE',  ( -8.260587980841940012E-17, 0.000000000000000000, -1.000000000000000000 ) ) ;
#46020 = CARTESIAN_POINT ( 'NONE',  ( 8.575906144586953772, -0.1092432217106413528, 50.52422457691089619 ) ) ;
#46021 = CARTESIAN_POINT ( 'NONE',  ( -10.37743123699495307, -15.12446308634721603, 74.79778699417029486 ) ) ;
#46022 = CARTESIAN_POINT ( 'NONE',  ( -20.49909385650551741, -8.114302828567740988, 52.18300498402516041 ) ) ;
#46023 = CARTESIAN_POINT ( 'NONE',  ( -12.43267529144301520, -19.71710391272808849, 61.39678636628809727 ) ) ;
#46024 = CARTESIAN_POINT ( 'NONE',  ( -24.05420634179087358, -17.20676946999824608, 69.69867738674849988 ) ) ;
#46025 = CARTESIAN_POINT ( 'NONE',  ( -10.37394849890712401, -14.76283852923608286, 71.61310637325181006 ) ) ;
#46026 = ORIENTED_EDGE ( 'NONE', *, *, #40392, .F. ) ;
#46027 = ORIENTED_EDGE ( 'NONE', *, *, #16553, .F. ) ;
#46028 = CARTESIAN_POINT ( 'NONE',  ( -22.62394951084894146, -10.04809318868971424, 70.29706442286226320 ) ) ;
#46029 =( NAMED_UNIT ( * ) SI_UNIT ( $, .STERADIAN. ) SOLID_ANGLE_UNIT ( ) );
#46030 = EDGE_CURVE ( 'NONE', #14825, #10444, #4654, .T. ) ;
#46031 = CARTESIAN_POINT ( 'NONE',  ( -14.60783614669699304, -21.70648650955843806, 58.35113213314874514 ) ) ;
#46032 = DIRECTION ( 'NONE',  ( -0.6607190350374015919, -0.7506333037770474004, 0.000000000000000000 ) ) ;
#46033 = CARTESIAN_POINT ( 'NONE',  ( -18.90456104531098092, -7.507023198961870314, 70.55723427638547207 ) ) ;
#46034 = ADVANCED_FACE ( 'NONE', ( #19203 ), #37660, .T. ) ;
#46035 = ORIENTED_EDGE ( 'NONE', *, *, #3136, .T. ) ;
#46036 = AXIS2_PLACEMENT_3D ( 'NONE', #14307, #48548, #44628 ) ;
#46037 = ORIENTED_EDGE ( 'NONE', *, *, #42135, .T. ) ;
#46038 = DIRECTION ( 'NONE',  ( 0.06357898915123888495, -0.9979768094191902028, 2.038786632797724544E-16 ) ) ;
#46039 = CARTESIAN_POINT ( 'NONE',  ( -14.93767672275562575, -21.83209540852061181, 65.29934976567700744 ) ) ;
#46040 = LINE ( 'NONE', #12296, #25666 ) ;
#46041 = EDGE_CURVE ( 'NONE', #45281, #15441, #5436, .T. ) ;
#46042 = EDGE_LOOP ( 'NONE', ( #30900, #14438 ) ) ;
#46043 = FACE_OUTER_BOUND ( 'NONE', #45188, .T. ) ;
#46044 = DIRECTION ( 'NONE',  ( -3.071710424422018668E-17, 6.404604876783312462E-16, 1.000000000000000000 ) ) ;
#46045 = ORIENTED_EDGE ( 'NONE', *, *, #16695, .T. ) ;
#46046 = CYLINDRICAL_SURFACE ( 'NONE', #36710, 0.1500000000000007716 ) ;
#46047 = DIRECTION ( 'NONE',  ( 0.8507615431891570879, -0.5255518971808580408, -6.876821557926347540E-08 ) ) ;
#46048 = VERTEX_POINT ( 'NONE', #7656 ) ;
#46049 = CARTESIAN_POINT ( 'NONE',  ( -23.65754020941666269, -18.88946062594842701, 69.47184773153367132 ) ) ;
#46050 = EDGE_LOOP ( 'NONE', ( #9227, #10057 ) ) ;
#46051 = CYLINDRICAL_SURFACE ( 'NONE', #7112, 0.1500000000000061007 ) ;
#46052 = FACE_OUTER_BOUND ( 'NONE', #6388, .T. ) ;
#46053 = ORIENTED_EDGE ( 'NONE', *, *, #17440, .F. ) ;
#46054 = CARTESIAN_POINT ( 'NONE',  ( -23.96654618570108042, -17.44381333609114648, 62.35872369075587329 ) ) ;
#46055 = CARTESIAN_POINT ( 'NONE',  ( -16.16784385541286895, -9.357632978295828963, 49.97845033065649289 ) ) ;
#46056 = CARTESIAN_POINT ( 'NONE',  ( -17.99909385650551741, -8.114302828567740988, 52.18300498402516041 ) ) ;
#46057 = CARTESIAN_POINT ( 'NONE',  ( -11.97955916273614285, -10.40884600102296176, 70.98509759323277990 ) ) ;
#46058 = EDGE_CURVE ( 'NONE', #4721, #5613, #16325, .T. ) ;
#46059 = CARTESIAN_POINT ( 'NONE',  ( -19.24190786459753610, -7.584296138276666710, 63.54593947706258206 ) ) ;
#46060 = LINE ( 'NONE', #7677, #38405 ) ;
#46061 = VERTEX_POINT ( 'NONE', #15484 ) ;
#46062 = PLANE ( 'NONE',  #16840 ) ;
#46063 = CARTESIAN_POINT ( 'NONE',  ( -11.43058294688041165, -10.38410865082031442, 74.48239070398270201 ) ) ;
#46064 = AXIS2_PLACEMENT_3D ( 'NONE', #46144, #38503, #34311 ) ;
#46065 = CARTESIAN_POINT ( 'NONE',  ( -15.60534385541290980, -7.595227055684650175, 51.75156210489618758 ) ) ;
#46066 = PLANE ( 'NONE',  #1479 ) ;
#46067 = DIRECTION ( 'NONE',  ( -1.069388061899112173E-05, 2.778940573026428581E-06, 0.9999999999389591609 ) ) ;
#46068 = VERTEX_POINT ( 'NONE', #30062 ) ;
#46069 = ORIENTED_EDGE ( 'NONE', *, *, #31293, .T. ) ;
#46070 = CARTESIAN_POINT ( 'NONE',  ( -15.35027035934970918, -7.653577032698213323, 74.26481056556292515 ) ) ;
#46071 = CARTESIAN_POINT ( 'NONE',  ( -24.37683887807358118, -15.97618392648307761, 66.36324926629207255 ) ) ;
#46072 = ORIENTED_EDGE ( 'NONE', *, *, #26113, .T. ) ;
#46073 = CARTESIAN_POINT ( 'NONE',  ( -22.48237781098097798, -19.73147542146173450, 65.85988959519353614 ) ) ;
#46074 = CYLINDRICAL_SURFACE ( 'NONE', #5891, 0.1499999999999979128 ) ;
#46075 = CARTESIAN_POINT ( 'NONE',  ( -23.04367355717579002, -10.55211556811382678, 59.90203429191419104 ) ) ;
#46076 = CARTESIAN_POINT ( 'NONE',  ( -24.74348659356070002, -16.19898255343749582, 62.73182120491487268 ) ) ;
#46077 = B_SPLINE_CURVE_WITH_KNOTS ( 'NONE', 3,
 ( #14160, #7548, #30205, #33126, #40775, #45226, #44735, #29455, #26010, #26493 ),
 .UNSPECIFIED., .F., .F.,
 ( 4, 2, 2, 2, 4 ),
 ( 0.000000000000000000, 0.2500000000000000000, 0.5000000000000000000, 0.7500000000000000000, 1.000000000000000000 ),
 .UNSPECIFIED. ) ;
#46078 = CARTESIAN_POINT ( 'NONE',  ( -12.10067708704646527, -20.02116635982656945, 61.58952802380450464 ) ) ;
#46079 = CARTESIAN_POINT ( 'NONE',  ( -17.42409385541299471, -14.80920654474434883, 62.02966884056656482 ) ) ;
#46080 = FACE_BOUND ( 'NONE', #39368, .T. ) ;
#46081 = ORIENTED_EDGE ( 'NONE', *, *, #28530, .F. ) ;
#46082 = PRODUCT ( 'Attachment Screw', 'Attachment Screw', '', ( #4106 ) ) ;
#46083 = DIRECTION ( 'NONE',  ( 0.1738928961406289442, -0.9847645711904030597, -7.871847300026996438E-08 ) ) ;
#46084 = ADVANCED_FACE ( 'NONE', ( #11091 ), #16, .T. ) ;
#46085 = CARTESIAN_POINT ( 'NONE',  ( -22.66727108289645543, -10.09628893573625064, 70.01178520457129650 ) ) ;
#46086 = DIRECTION ( 'NONE',  ( 0.9687793358424821033, -0.2479245821708679909, 0.000000000000000000 ) ) ;
#46087 = CARTESIAN_POINT ( 'NONE',  ( -11.86838218109940790, -9.845554053733961197, 64.14419007574942100 ) ) ;
#46088 = EDGE_CURVE ( 'NONE', #31720, #15639, #37516, .T. ) ;
#46089 = ORIENTED_EDGE ( 'NONE', *, *, #14834, .F. ) ;
#46090 = ORIENTED_EDGE ( 'NONE', *, *, #44457, .T. ) ;
#46091 = CARTESIAN_POINT ( 'NONE',  ( -20.16691211377460391, -21.73601867580754288, 72.58974061177721637 ) ) ;
#46092 = EDGE_CURVE ( 'NONE', #21832, #43615, #3430, .T. ) ;
#46093 = ORIENTED_EDGE ( 'NONE', *, *, #41060, .T. ) ;
#46094 = CARTESIAN_POINT ( 'NONE',  ( -12.00385017463665704, -9.698023059171664073, 60.75256377526179818 ) ) ;
#46095 = CARTESIAN_POINT ( 'NONE',  ( -17.42409385541300892, -14.80920654474439679, 54.49999999999994316 ) ) ;
#46096 = EDGE_CURVE ( 'NONE', #28180, #44222, #28110, .T. ) ;
#46097 = EDGE_LOOP ( 'NONE', ( #25625, #6342, #560, #32935 ) ) ;
#46098 = CARTESIAN_POINT ( 'NONE',  ( -11.14114473067313682, -10.80566704772025233, 57.32407823191172014 ) ) ;
#46099 = CIRCLE ( 'NONE', #48441, 0.2499999999999976408 ) ;
#46100 = CARTESIAN_POINT ( 'NONE',  ( -13.36271920075327557, -8.563530200375994994, 57.07629425018297553 ) ) ;
#46101 = ORIENTED_EDGE ( 'NONE', *, *, #33107, .F. ) ;
#46102 = CARTESIAN_POINT ( 'NONE',  ( -20.93707211197437346, -8.239410368917360117, 60.03463562270969334 ) ) ;
#46103 = CARTESIAN_POINT ( 'NONE',  ( -23.77826926726992340, -17.74977703228070069, 62.66287969925918588 ) ) ;
#46104 = ORIENTED_EDGE ( 'NONE', *, *, #46979, .F. ) ;
#46105 = CARTESIAN_POINT ( 'NONE',  ( -19.97164249076357478, -21.81019033462135326, 69.11977790463622284 ) ) ;
#46106 = EDGE_CURVE ( 'NONE', #39956, #8033, #3051, .T. ) ;
#46107 = CARTESIAN_POINT ( 'NONE',  ( -13.53919695188330508, -21.16624214383947589, 65.10816087775715744 ) ) ;
#46108 = EDGE_CURVE ( 'NONE', #26226, #41394, #26348, .T. ) ;
#46109 = ORIENTED_EDGE ( 'NONE', *, *, #21294, .T. ) ;
#46110 = CARTESIAN_POINT ( 'NONE',  ( -10.37081839464344668, -14.73079292305692789, 67.85800084537061139 ) ) ;
#46111 = CARTESIAN_POINT ( 'NONE',  ( -16.98902004117856990, -21.84877635801032270, 68.58071880800348197 ) ) ;
#46112 = CARTESIAN_POINT ( 'NONE',  ( -18.53201708017407157, -7.846807123103141102, 74.14064401780551350 ) ) ;
#46113 = EDGE_LOOP ( 'NONE', ( #10733, #7411, #47320, #23445, #12833, #39167 ) ) ;
#46114 = CARTESIAN_POINT ( 'NONE',  ( -10.91516777394897986, -11.18477724879597623, 64.34893244028862114 ) ) ;
#46115 = CARTESIAN_POINT ( 'NONE',  ( -19.42896492416523913, -21.56812594671148275, 61.99503644571810668 ) ) ;
#46116 =( BOUNDED_SURFACE ( )  B_SPLINE_SURFACE ( 3, 1, ( 
 ( #21480, #36234 ),
 ( #3236, #28389 ),
 ( #2517, #10399 ),
 ( #17277, #6692 ),
 ( #47578, #39700 ),
 ( #20988, #32781 ),
 ( #47347, #13810 ) ),
 .UNSPECIFIED., .T., .F., .F. ) 
 B_SPLINE_SURFACE_WITH_KNOTS ( ( 4, 3, 4 ),
 ( 2, 2 ),
 ( 0.000000000000000000, 0.5000000000000000000, 1.000000000000000000 ),
 ( 0.000000000000000000, 1.000000000000000000 ),
 .UNSPECIFIED. ) 
 GEOMETRIC_REPRESENTATION_ITEM ( )  RATIONAL_B_SPLINE_SURFACE ( (
 ( 1.000000000000000000, 1.000000000000000000),
 ( 0.3333333333333335369, 0.3333333333333330373),
 ( 0.3333333333333335369, 0.3333333333333330373),
 ( 1.000000000000000000, 1.000000000000000000),
 ( 0.3333333333333333703, 0.3333333333333333703),
 ( 0.3333333333333333703, 0.3333333333333333703),
 ( 1.000000000000000000, 1.000000000000000000) ) ) 
 REPRESENTATION_ITEM ( '' )  SURFACE ( )  );
#46117 = EDGE_CURVE ( 'NONE', #21578, #20573, #33526, .T. ) ;
#46118 = CARTESIAN_POINT ( 'NONE',  ( -45.55409385541305767, -14.20920654474410760, 70.08498674719956512 ) ) ;
#46119 = CARTESIAN_POINT ( 'NONE',  ( -21.18398698114219769, -21.24092341087395752, 65.69958654271196963 ) ) ;
#46120 = CARTESIAN_POINT ( 'NONE',  ( -17.71784385759799108, -6.860780111191487229, 51.02154966934377711 ) ) ;
#46121 = CARTESIAN_POINT ( 'NONE',  ( -13.71339271347210342, -20.80363700974685059, 65.28628881287177421 ) ) ;
#46122 = CYLINDRICAL_SURFACE ( 'NONE', #6167, 0.1499999999999991618 ) ;
#46123 = CARTESIAN_POINT ( 'NONE',  ( -17.42409385541299471, -14.80920654474435771, 49.52966884056655772 ) ) ;
#46124 = CARTESIAN_POINT ( 'NONE',  ( -12.26581428767149795, -15.78626943986449405, 52.02966884056656482 ) ) ;
#46125 = CARTESIAN_POINT ( 'NONE',  ( -14.76159385650551847, -9.295667164867525756, 49.30633214617472504 ) ) ;
#46126 = ORIENTED_EDGE ( 'NONE', *, *, #47427, .T. ) ;
#46127 = DIRECTION ( 'NONE',  ( -3.071710424422018668E-17, 6.404604876783312462E-16, 1.000000000000000000 ) ) ;
#46128 = FACE_OUTER_BOUND ( 'NONE', #24892, .T. ) ;
#46129 = ORIENTED_EDGE ( 'NONE', *, *, #15162, .F. ) ;
#46130 = LINE ( 'NONE', #27899, #37856 ) ;
#46131 = CARTESIAN_POINT ( 'NONE',  ( -10.63483715323753565, -17.87674169505483235, 71.75213630217804450 ) ) ;
#46132 = CARTESIAN_POINT ( 'NONE',  ( -24.46812100523181144, -14.51191712007779699, 66.19764790277996269 ) ) ;
#46133 = DIRECTION ( 'NONE',  ( -0.000000000000000000, -1.000000000000000000, 0.000000000000000000 ) ) ;
#46134 = ORIENTED_EDGE ( 'NONE', *, *, #18753, .T. ) ;
#46135 = DIRECTION ( 'NONE',  ( 0.000000000000000000, -0.9999954153791273948, -0.003028072113819838245 ) ) ;
#46136 =( BOUNDED_CURVE ( )  B_SPLINE_CURVE ( 3, ( #15101, #355, #7263, #10941 ),
 .UNSPECIFIED., .F., .F. ) 
 B_SPLINE_CURVE_WITH_KNOTS ( ( 4, 4 ),
 ( 0.4074455897393662873, 0.5000000000000000000 ),
 .UNSPECIFIED. ) 
 CURVE ( )  GEOMETRIC_REPRESENTATION_ITEM ( )  RATIONAL_B_SPLINE_CURVE ( ( 0.6983129098260991707, 0.7760317562607093045, 0.8765941196520112833, 1.000000000000009326 ) ) 
 REPRESENTATION_ITEM ( '' )  );
#46137 = AXIS2_PLACEMENT_3D ( 'NONE', #40878, #24902, #47319 ) ;
#46138 = CARTESIAN_POINT ( 'NONE',  ( -24.42401644153718721, -14.84212863923847081, 59.24300237020570137 ) ) ;
#46139 = VECTOR ( 'NONE', #4925, 1000.000000000000000 ) ;
#46140 = DIRECTION ( 'NONE',  ( -2.526377660313140381E-06, -1.273612632024531482E-05, 0.9999999999157043185 ) ) ;
#46141 = ORIENTED_EDGE ( 'NONE', *, *, #24957, .F. ) ;
#46142 = CARTESIAN_POINT ( 'NONE',  ( -13.31471556610697249, -9.080541429120991381, 63.91506350995963714 ) ) ;
#46143 = VECTOR ( 'NONE', #17850, 1000.000000000000000 ) ;
#46144 = CARTESIAN_POINT ( 'NONE',  ( -17.42409385541305511, -14.80920654474410725, 48.99999999999997868 ) ) ;
#46145 = FACE_OUTER_BOUND ( 'NONE', #18086, .T. ) ;
#46146 = CARTESIAN_POINT ( 'NONE',  ( -21.77128597137166111, -8.759032111691572808, 70.23158298676763422 ) ) ;
#46147 = PLANE ( 'NONE',  #10252 ) ;
#46148 = ORIENTED_EDGE ( 'NONE', *, *, #34445, .T. ) ;
#46149 = ORIENTED_EDGE ( 'NONE', *, *, #30253, .F. ) ;
#46150 = CARTESIAN_POINT ( 'NONE',  ( -20.38659385541304303, -7.222650657624104298, 49.61879703869476543 ) ) ;
#46151 = EDGE_CURVE ( 'NONE', #15790, #700, #26111, .T. ) ;
#46152 = B_SPLINE_CURVE_WITH_KNOTS ( 'NONE', 3,
 ( #27849, #24167, #24657, #46583, #32030, #32285, #2477, #5703, #36191, #1756 ),
 .UNSPECIFIED., .F., .F.,
 ( 4, 2, 2, 2, 4 ),
 ( 0.1272669073658771188, 0.2522669073439901544, 0.3772669073221032177, 0.5022669073002161699, 0.6272669072783292332 ),
 .UNSPECIFIED. ) ;
#46153 = CARTESIAN_POINT ( 'NONE',  ( -22.99810592004713072, -9.865991162508992218, 70.17325022503489151 ) ) ;
#46154 = EDGE_CURVE ( 'NONE', #44219, #28192, #33694, .T. ) ;
#46155 = CARTESIAN_POINT ( 'NONE',  ( -17.42409385541299471, -14.80920654474435771, 49.52966884056655772 ) ) ;
#46156 = CARTESIAN_POINT ( 'NONE',  ( -10.78905035535072265, -17.04131954076935074, 61.44126548158209289 ) ) ;
#46157 = CARTESIAN_POINT ( 'NONE',  ( -24.47368665962210343, -14.70950332193510590, 62.72768537250228604 ) ) ;
#46158 = CARTESIAN_POINT ( 'NONE',  ( -10.43972881942000086, -15.77115500203794873, 64.52243715390834211 ) ) ;
#46159 = CARTESIAN_POINT ( 'NONE',  ( -18.32364513544568752, -21.80460793730824420, 65.23043427352648393 ) ) ;
#46160 = VERTEX_POINT ( 'NONE', #22759 ) ;
#46161 = CARTESIAN_POINT ( 'NONE',  ( -21.63336539757928634, -9.153348366551478321, 66.94677872351418557 ) ) ;
#46162 = ADVANCED_FACE ( 'NONE', ( #41948 ), #45173, .T. ) ;
#46163 = CARTESIAN_POINT ( 'NONE',  ( -21.36284794767689377, -21.13297080501056513, 69.16954792666395235 ) ) ;
#46164 = ADVANCED_FACE ( 'NONE', ( #4512 ), #40019, .F. ) ;
#46165 = CIRCLE ( 'NONE', #45402, 2.000000000000001776 ) ;
#46166 = AXIS2_PLACEMENT_3D ( 'NONE', #30913, #41489, #33851 ) ;
#46167 = ORIENTED_EDGE ( 'NONE', *, *, #25297, .F. ) ;
#46168 = CARTESIAN_POINT ( 'NONE',  ( -21.53861794036900079, -21.02004141303368101, 72.63951040967180006 ) ) ;
#46169 = CARTESIAN_POINT ( 'NONE',  ( -13.60238606012557483, -8.884930320952351579, 56.96967755506135234 ) ) ;
#46170 = EDGE_CURVE ( 'NONE', #8953, #37481, #46314, .T. ) ;
#46172 = EDGE_CURVE ( 'NONE', #313, #35202, #21665, .T. ) ;
#46171 = ORIENTED_EDGE ( 'NONE', *, *, #28298, .T. ) ;
#46173 = DIRECTION ( 'NONE',  ( 0.7700094066334507437, 0.6380325334150297456, 2.326497556385334706E-17 ) ) ;
#46174 = EDGE_CURVE ( 'NONE', #43409, #36016, #15574, .T. ) ;
#46175 = CARTESIAN_POINT ( 'NONE',  ( -21.90726424129253047, -20.25032565763172343, 58.77002696425551420 ) ) ;
#46176 = VECTOR ( 'NONE', #4996, 1000.000000000000000 ) ;
#46177 = CARTESIAN_POINT ( 'NONE',  ( -21.73229268148169879, -8.731123941674052702, 70.17486588183628271 ) ) ;
#46178 = CARTESIAN_POINT ( 'NONE',  ( -24.30269901035189761, -16.11584067364758610, 66.17398127870760050 ) ) ;
#46179 = ORIENTED_EDGE ( 'NONE', *, *, #48623, .T. ) ;
#46180 = CARTESIAN_POINT ( 'NONE',  ( -10.95917937052863422, -17.62195967018737619, 71.58190244267143498 ) ) ;
#46181 = CARTESIAN_POINT ( 'NONE',  ( -10.91684962386814917, -11.18174702714047442, 64.24907796807872273 ) ) ;
#46182 = CARTESIAN_POINT ( 'NONE',  ( -17.42409385541300892, -14.80920654474439679, 47.99999999999994316 ) ) ;
#46183 = CONTEXT_DEPENDENT_SHAPE_REPRESENTATION ( #46403, #22049 ) ;
#46184 = DIRECTION ( 'NONE',  ( 0.9922778767136677391, 0.000000000000000000, -0.1240347345892083841 ) ) ;
#46185 = CARTESIAN_POINT ( 'NONE',  ( -11.53247150430815715, -18.68106468654471541, 64.89707076448696910 ) ) ;
#46186 = CARTESIAN_POINT ( 'NONE',  ( -10.54994933093899867, -13.24305344519376781, 71.49356453765415154 ) ) ;
#46187 = ORIENTED_EDGE ( 'NONE', *, *, #22141, .T. ) ;
#46188 = CARTESIAN_POINT ( 'NONE',  ( -17.77409385759798965, -6.859212275519751323, 50.50378509014259265 ) ) ;
#46189 = ORIENTED_EDGE ( 'NONE', *, *, #25919, .F. ) ;
#46190 = B_SPLINE_CURVE_WITH_KNOTS ( 'NONE', 3,
 ( #28047, #2191, #29690, #22062, #48393, #20912, #24851, #40765, #5894, #37061 ),
 .UNSPECIFIED., .F., .F.,
 ( 4, 2, 2, 2, 4 ),
 ( 0.6272669072877737895, 0.7522669073072834056, 0.8772669073267929107, 1.002266907346302638, 1.127266907365812143 ),
 .UNSPECIFIED. ) ;
#46191 = CARTESIAN_POINT ( 'NONE',  ( -11.19248847611778785, -11.62034934314885959, 67.61864580749579545 ) ) ;
#46192 = CARTESIAN_POINT ( 'NONE',  ( -16.77486212007157818, -22.23091360578541043, 68.80222337029485402 ) ) ;
#46193 = ORIENTED_EDGE ( 'NONE', *, *, #32593, .F. ) ;
#46194 = DIRECTION ( 'NONE',  ( -2.866981220435666553E-17, 1.000000000000000000, 1.190614954331866791E-16 ) ) ;
#46195 = FACE_BOUND ( 'NONE', #39196, .T. ) ;
#46196 = EDGE_LOOP ( 'NONE', ( #19756, #33073, #31665, #6066, #41838 ) ) ;
#46197 = ADVANCED_FACE ( 'NONE', ( #30391 ), #580, .T. ) ;
#46198 = ORIENTED_EDGE ( 'NONE', *, *, #38597, .F. ) ;
#46199 = VERTEX_POINT ( 'NONE', #45890 ) ;
#46200 = CARTESIAN_POINT ( 'NONE',  ( -17.98657259272421172, -21.83703102787368167, 62.16063850355641307 ) ) ;
#46201 = CARTESIAN_POINT ( 'NONE',  ( -18.73233999060757426, -21.74043542732912826, 72.49330701881069672 ) ) ;
#46202 = CARTESIAN_POINT ( 'NONE',  ( -48.42409385541304800, -25.10920654474410441, 45.99999999999998579 ) ) ;
#46203 = CARTESIAN_POINT ( 'NONE',  ( -14.41428173599358331, -7.994163662063686893, 63.97474278339937115 ) ) ;
#46204 = CARTESIAN_POINT ( 'NONE',  ( -12.57344172079930544, -19.85833258862019335, 68.52584420683459143 ) ) ;
#46205 = CARTESIAN_POINT ( 'NONE',  ( -16.30609998749194745, -22.17489236838497746, 61.94906455514021815 ) ) ;
#46206 = VECTOR ( 'NONE', #29018, 1000.000000000000000 ) ;
#46207 = ORIENTED_EDGE ( 'NONE', *, *, #33600, .F. ) ;
#46208 = ORIENTED_EDGE ( 'NONE', *, *, #33169, .T. ) ;
#46209 = CARTESIAN_POINT ( 'NONE',  ( -20.98034385650551314, -6.424090610841176385, 49.80797279389977916 ) ) ;
#46210 = EDGE_CURVE ( 'NONE', #9191, #42180, #14555, .T. ) ;
#46211 = CARTESIAN_POINT ( 'NONE',  ( -29.92409385541305156, -6.359206544744109735, 52.99999999999997158 ) ) ;
#46212 = CARTESIAN_POINT ( 'NONE',  ( -21.00380318978402627, -21.34292366101719196, 62.22975991904223747 ) ) ;
#46213 = VECTOR ( 'NONE', #26429, 999.9999999999998863 ) ;
#46214 = CARTESIAN_POINT ( 'NONE',  ( -21.49816216734858898, -9.116934002111024782, 70.13132539266752019 ) ) ;
#46215 = ORIENTED_EDGE ( 'NONE', *, *, #20900, .T. ) ;
#46216 = CARTESIAN_POINT ( 'NONE',  ( -21.93659385650551741, -6.915538690918074494, 49.31353937987644542 ) ) ;
#46217 = EDGE_LOOP ( 'NONE', ( #37564, #2702 ) ) ;
#46218 = CARTESIAN_POINT ( 'NONE',  ( -23.00382044653182945, -10.58231046269237829, 59.60203429539187425 ) ) ;
#46219 = CARTESIAN_POINT ( 'NONE',  ( -30.42409385541305156, -8.109206544744111511, 50.50000000000000000 ) ) ;
#46220 = DIRECTION ( 'NONE',  ( -0.9959323210854037489, 0.09010444948746665350, 2.601165157765155817E-08 ) ) ;
#46221 = VERTEX_POINT ( 'NONE', #37994 ) ;
#46222 = DIRECTION ( 'NONE',  ( -0.5881408891789771110, -0.8087584895849666555, 7.565907428972492613E-08 ) ) ;
#46223 = CARTESIAN_POINT ( 'NONE',  ( -22.79960313759534074, -9.650943445293346912, 73.66656413195866548 ) ) ;
#46224 = CARTESIAN_POINT ( 'NONE',  ( -10.43073325114686511, -14.50439929630985603, 68.15800126138398696 ) ) ;
#46225 = EDGE_CURVE ( 'NONE', #44868, #26800, #10132, .T. ) ;
#46226 = EDGE_CURVE ( 'NONE', #1531, #8650, #14671, .T. ) ;
#46227 = CARTESIAN_POINT ( 'NONE',  ( -22.84073111900424990, -19.92438295589304786, 72.78254066635705044 ) ) ;
#46228 = ORIENTED_EDGE ( 'NONE', *, *, #27487, .T. ) ;
#46229 = VECTOR ( 'NONE', #871, 1000.000000000000114 ) ;
#46230 = CARTESIAN_POINT ( 'NONE',  ( -14.10256395084115866, -8.140532207465255965, 70.84462205307964666 ) ) ;
#46231 = LINE ( 'NONE', #19391, #9488 ) ;
#46232 = CARTESIAN_POINT ( 'NONE',  ( -20.43185948505062299, -8.432683554863363184, 66.79576150497511833 ) ) ;
#46233 = EDGE_LOOP ( 'NONE', ( #3295, #20176, #1610, #28928, #20787 ) ) ;
#46234 = CARTESIAN_POINT ( 'NONE',  ( -16.00230047675183087, -7.496128538412458298, 63.87022237253693646 ) ) ;
#46235 = AXIS2_PLACEMENT_3D ( 'NONE', #3650, #22878, #7367 ) ;
#46236 = CIRCLE ( 'NONE', #25008, 5.249999999999998224 ) ;
#46237 = ORIENTED_EDGE ( 'NONE', *, *, #28308, .F. ) ;
#46238 = CARTESIAN_POINT ( 'NONE',  ( -15.28965001900414755, -21.53148179447737220, 64.99108044553886998 ) ) ;
#46239 = ADVANCED_FACE ( 'NONE', ( #23240 ), #19050, .T. ) ;
#46240 = EDGE_CURVE ( 'NONE', #27154, #45533, #34478, .T. ) ;
#46241 = CARTESIAN_POINT ( 'NONE',  ( -15.03263910315855512, -8.176888424288380364, 56.86472059657746314 ) ) ;
#46242 = ORIENTED_EDGE ( 'NONE', *, *, #7401, .T. ) ;
#46243 = DIRECTION ( 'NONE',  ( -2.866981220435666553E-17, 1.000000000000000000, 1.190614954331866791E-16 ) ) ;
#46244 = CARTESIAN_POINT ( 'NONE',  ( -10.72017361938626934, -12.61779402817458973, 57.21368711609748203 ) ) ;
#46245 = CARTESIAN_POINT ( 'NONE',  ( -14.21809028606166869, -8.084188479104598812, 67.38162348312260974 ) ) ;
#46246 = CYLINDRICAL_SURFACE ( 'NONE', #39249, 4.686499999999997002 ) ;
#46247 = EDGE_LOOP ( 'NONE', ( #14990, #44045, #21057, #14577, #2803 ) ) ;
#46248 = FACE_OUTER_BOUND ( 'NONE', #28455, .T. ) ;
#46249 = FACE_OUTER_BOUND ( 'NONE', #20083, .T. ) ;
#46250 = CARTESIAN_POINT ( 'NONE',  ( -23.10220861922097768, -9.986187529005633223, 66.69182256001187170 ) ) ;
#46251 = FACE_OUTER_BOUND ( 'NONE', #48534, .T. ) ;
#46252 = VERTEX_POINT ( 'NONE', #3792 ) ;
#46253 = VECTOR ( 'NONE', #12576, 1000.000000000000227 ) ;
#46254 = CARTESIAN_POINT ( 'NONE',  ( -24.72559841154505023, -16.28986789441275107, 62.77141465262073439 ) ) ;
#46255 = EDGE_CURVE ( 'NONE', #7279, #34665, #31620, .T. ) ;
#46256 = ORIENTED_EDGE ( 'NONE', *, *, #6613, .T. ) ;
#46257 = ORIENTED_EDGE ( 'NONE', *, *, #41490, .F. ) ;
#46258 = CARTESIAN_POINT ( 'NONE',  ( -10.49223796394545616, -15.78356480554473862, 61.14675028274938740 ) ) ;
#46259 = CARTESIAN_POINT ( 'NONE',  ( -10.54994933093899867, -13.24305344519376959, 71.49356453765415154 ) ) ;
#46260 = DIRECTION ( 'NONE',  ( 0.9294853595766526810, 0.3688590060343663324, 6.440324111080732189E-17 ) ) ;
#46261 = CARTESIAN_POINT ( 'NONE',  ( -13.10534385759798681, -7.595227055684746986, 51.75156210489594599 ) ) ;
#46262 = CARTESIAN_POINT ( 'NONE',  ( -12.18719842096713357, -10.08886484896570934, 64.04386393395434141 ) ) ;
#46263 =( BOUNDED_CURVE ( )  B_SPLINE_CURVE ( 3, ( #2603, #25728, #6299, #9989 ),
 .UNSPECIFIED., .F., .F. ) 
 B_SPLINE_CURVE_WITH_KNOTS ( ( 4, 4 ),
 ( 1.675516081914553590, 1.780235837034217283 ),
 .UNSPECIFIED. ) 
 CURVE ( )  GEOMETRIC_REPRESENTATION_ITEM ( )  RATIONAL_B_SPLINE_CURVE ( ( 1.000000000000000000, 0.9990863565030491111, 0.9990863565030491111, 1.000000000000000000 ) ) 
 REPRESENTATION_ITEM ( '' )  );
#46264 = DIRECTION ( 'NONE',  ( 1.224646799147353207E-16, 1.000000000000000000, -1.912410701131276611E-32 ) ) ;
#46265 = DIRECTION ( 'NONE',  ( -1.000000000000000000, 0.000000000000000000, -0.000000000000000000 ) ) ;
#46266 = CARTESIAN_POINT ( 'NONE',  ( -24.72409385541305582, -14.90920654474427565, 73.09411764705880898 ) ) ;
#46267 = ORIENTED_EDGE ( 'NONE', *, *, #6200, .F. ) ;
#46268 = ORIENTED_EDGE ( 'NONE', *, *, #24687, .T. ) ;
#46269 = CARTESIAN_POINT ( 'NONE',  ( -10.85811841353450369, -12.22020323829153554, 74.71407760726656022 ) ) ;
#46270 = B_SPLINE_CURVE_WITH_KNOTS ( 'NONE', 3,
 ( #25687, #37981, #15317, #4266, #29885, #41199, #18286, #40707, #14333, #22746 ),
 .UNSPECIFIED., .F., .F.,
 ( 4, 2, 2, 2, 4 ),
 ( 0.000000000000000000, 0.2500000000000000000, 0.5000000000000000000, 0.7500000000000000000, 1.000000000000000000 ),
 .UNSPECIFIED. ) ;
#46271 = DIRECTION ( 'NONE',  ( 1.000000000000000000, 0.000000000000000000, 0.000000000000000000 ) ) ;
#46272 = CARTESIAN_POINT ( 'NONE',  ( -21.91034545428830782, -20.18261758176410936, 58.76442899736473180 ) ) ;
#46273 = CIRCLE ( 'NONE', #11679, 2.500000000000002220 ) ;
#46274 = CARTESIAN_POINT ( 'NONE',  ( -21.95938932932862642, -9.477124872050278981, 60.02171213236835712 ) ) ;
#46275 = CARTESIAN_POINT ( 'NONE',  ( -23.90247617018859572, -17.59042147582948701, 62.76801221965811095 ) ) ;
#46276 = VECTOR ( 'NONE', #38235, 1000.000000000000000 ) ;
#46277 =( BOUNDED_CURVE ( )  B_SPLINE_CURVE ( 2, ( #11976, #41771, #19346, #3595, #15888, #23545, #15641, #23297, #26252 ),
 .UNSPECIFIED., .F., .F. ) 
 B_SPLINE_CURVE_WITH_KNOTS ( ( 3, 2, 2, 2, 3 ),
 ( 0.07868091852197928171, 0.07966438894987652730, 0.08064785937777378677, 0.08163132980567104624, 0.08261480023356829183 ),
 .UNSPECIFIED. ) 
 CURVE ( )  GEOMETRIC_REPRESENTATION_ITEM ( )  RATIONAL_B_SPLINE_CURVE ( ( 0.9999999999999700240, 0.9238795325113167145, 1.000000000000000000, 0.9238795325112867385, 1.000000000000000000, 0.9238795325112867385, 1.000000000000000000, 0.9238795325111349710, 1.000000000000151656 ) ) 
 REPRESENTATION_ITEM ( '' )  );
#46278 = AXIS2_PLACEMENT_3D ( 'NONE', #24028, #35082, #1346 ) ;
#46279 = AXIS2_PLACEMENT_3D ( 'NONE', #44991, #14896, #18112 ) ;
#46280 = ORIENTED_EDGE ( 'NONE', *, *, #6281, .F. ) ;
#46281 = CARTESIAN_POINT ( 'NONE',  ( -19.92716201441182378, -21.34638099545626133, 69.11007586060172514 ) ) ;
#46282 = CARTESIAN_POINT ( 'NONE',  ( -24.46146587544552276, -14.38248120490118787, 66.46820668217904426 ) ) ;
#46283 = B_SPLINE_CURVE_WITH_KNOTS ( 'NONE', 3,
 ( #38871, #1689, #1192, #43048, #23866, #9326, #19681, #8354, #45796, #34687 ),
 .UNSPECIFIED., .F., .F.,
 ( 4, 2, 2, 2, 4 ),
 ( 0.1272669073658402039, 0.2522669073463257305, 0.3772669073268112294, 0.5022669073072968393, 0.6272669072877823382 ),
 .UNSPECIFIED. ) ;
#46284 = CARTESIAN_POINT ( 'NONE',  ( -17.33262245845742910, -7.759502110702281463, 67.30567542699309058 ) ) ;
#46285 = CARTESIAN_POINT ( 'NONE',  ( -15.81422232498451130, -7.535173854406034266, 67.33345604418946095 ) ) ;
#46286 = AXIS2_PLACEMENT_3D ( 'NONE', #28246, #9781, #47924 ) ;
#46287 = ORIENTED_EDGE ( 'NONE', *, *, #41377, .F. ) ;
#46288 = CARTESIAN_POINT ( 'NONE',  ( -24.46828707212341669, -14.45681828193256280, 70.06763959435293998 ) ) ;
#46289 =( BOUNDED_CURVE ( )  B_SPLINE_CURVE ( 3, ( #45912, #42936, #26953, #9211 ),
 .UNSPECIFIED., .F., .F. ) 
 B_SPLINE_CURVE_WITH_KNOTS ( ( 4, 4 ),
 ( 0.9074455897393635118, 1.000000000000000000 ),
 .UNSPECIFIED. ) 
 CURVE ( )  GEOMETRIC_REPRESENTATION_ITEM ( )  RATIONAL_B_SPLINE_CURVE ( ( 0.6983129098260891787, 0.7760317562606948716, 0.8765941196519985157, 1.000000000000000000 ) ) 
 REPRESENTATION_ITEM ( '' )  );
#46290 = ADVANCED_FACE ( 'NONE', ( #35990 ), #27650, .T. ) ;
#46291 = EDGE_LOOP ( 'NONE', ( #33518, #1613, #38008, #17098 ) ) ;
#46292 = CARTESIAN_POINT ( 'NONE',  ( -12.86132678492178982, -20.11796087281938838, 71.80653668692889369 ) ) ;
#46293 = DIRECTION ( 'NONE',  ( -0.7506333037770538397, 0.6607190350373941534, 0.000000000000000000 ) ) ;
#46294 = ORIENTED_EDGE ( 'NONE', *, *, #11328, .T. ) ;
#46295 = CARTESIAN_POINT ( 'NONE',  ( -13.29821074602480557, -9.088145836456059001, 67.47123022012044657 ) ) ;
#46296 = EDGE_LOOP ( 'NONE', ( #32499, #32437, #41768, #714 ) ) ;
#46297 = ADVANCED_FACE ( 'NONE', ( #9908 ), #13334, .T. ) ;
#46298 = DIRECTION ( 'NONE',  ( -1.000000000000000000, -2.866981220435666553E-17, -0.000000000000000000 ) ) ;
#46299 = CARTESIAN_POINT ( 'NONE',  ( -10.42407724285790138, -14.83420999182403577, 71.55456108509550006 ) ) ;
#46300 = ORIENTED_EDGE ( 'NONE', *, *, #17770, .T. ) ;
#46301 = CARTESIAN_POINT ( 'NONE',  ( -24.44689184067228638, -14.18710713894228093, 69.93803194250310185 ) ) ;
#46302 = CARTESIAN_POINT ( 'NONE',  ( -10.29602973214897155, -12.64239231158840759, 64.39119220775197050 ) ) ;
#46303 = EDGE_CURVE ( 'NONE', #36695, #15426, #21904, .T. ) ;
#46304 = CARTESIAN_POINT ( 'NONE',  ( -15.86159385650551634, -9.295667164867525756, 49.30633214617472504 ) ) ;
#46305 = CIRCLE ( 'NONE', #3046, 1.000000000000000888 ) ;
#46306 = CARTESIAN_POINT ( 'NONE',  ( -23.53384949963793105, -19.19053592108923212, 53.76227901944321275 ) ) ;
#46307 = ADVANCED_FACE ( 'NONE', ( #43413 ), #42915, .T. ) ;
#46308 = VECTOR ( 'NONE', #21505, 1000.000000000000000 ) ;
#46309 = CARTESIAN_POINT ( 'NONE',  ( -10.64890997270348549, -11.71061566262665998, 74.68123243985192516 ) ) ;
#46310 = CARTESIAN_POINT ( 'NONE',  ( -16.43749525924751964, -22.19434601430465293, 61.86912739712975906 ) ) ;
#46311 = VERTEX_POINT ( 'NONE', #16302 ) ;
#46312 = CYLINDRICAL_SURFACE ( 'NONE', #12152, 5.249999999999998224 ) ;
#46313 = AXIS2_PLACEMENT_3D ( 'NONE', #41522, #33373, #3866 ) ;
#46314 = CIRCLE ( 'NONE', #35296, 1.999999999999999334 ) ;
#46315 = CARTESIAN_POINT ( 'NONE',  ( -10.95467737376780271, -17.63084047650967889, 64.78306623841410783 ) ) ;
#46316 = CARTESIAN_POINT ( 'NONE',  ( -40.92409385541305511, -14.80920654474410725, 74.99999999999998579 ) ) ;
#46317 = CARTESIAN_POINT ( 'NONE',  ( -24.59503728228645159, -12.78882255129604850, 66.47963607747338699 ) ) ;
#46318 = CARTESIAN_POINT ( 'NONE',  ( -20.68576141724628670, -21.00469082583299496, 62.30398495060934749 ) ) ;
#46319 = VERTEX_POINT ( 'NONE', #35744 ) ;
#46320 = ORIENTED_EDGE ( 'NONE', *, *, #48395, .F. ) ;
#46321 = CARTESIAN_POINT ( 'NONE',  ( -18.55957040452605611, -7.446158924837727788, 74.02559677774105751 ) ) ;
#46322 = CARTESIAN_POINT ( 'NONE',  ( -10.35879128504702251, -12.44577124159657089, 60.97666315383261804 ) ) ;
#46323 = EDGE_LOOP ( 'NONE', ( #10790, #34129 ) ) ;
#46324 = CARTESIAN_POINT ( 'NONE',  ( -15.81235419205221859, -7.945607373518419614, 67.42535135806457447 ) ) ;
#46325 = FACE_OUTER_BOUND ( 'NONE', #38310, .T. ) ;
#46326 = DIRECTION ( 'NONE',  ( -3.071710424422018668E-17, 6.404604876783312462E-16, 1.000000000000000000 ) ) ;
#46327 = CARTESIAN_POINT ( 'NONE',  ( -9.424093855413051557, -25.10920654474410441, 77.00000000000000000 ) ) ;
#46328 = DIRECTION ( 'NONE',  ( -0.1240347345892086200, 1.145860353393066553E-16, -0.9922778767136676281 ) ) ;
#46329 = CARTESIAN_POINT ( 'NONE',  ( -23.54569140518488624, -19.05536029250058050, 65.93894040291287695 ) ) ;
#46330 = DIRECTION ( 'NONE',  ( -0.9163203205182084421, -0.4004460890125009498, 2.380681625734479923E-09 ) ) ;
#46331 = ORIENTED_EDGE ( 'NONE', *, *, #37709, .T. ) ;
#46332 = CARTESIAN_POINT ( 'NONE',  ( -22.33376602745314798, -19.86903051493497685, 69.18890041286789483 ) ) ;
#46333 = CARTESIAN_POINT ( 'NONE',  ( -21.00380318978402627, -21.34292366101719196, 62.22975991904223747 ) ) ;
#46334 = CARTESIAN_POINT ( 'NONE',  ( -23.13305522301093120, -10.65917872773856878, 63.21619042434998903 ) ) ;
#46335 = CARTESIAN_POINT ( 'NONE',  ( -12.52591726580351228, -9.195683270288645517, 74.50418291613799227 ) ) ;
#46336 = CARTESIAN_POINT ( 'NONE',  ( -21.38734882604794407, -9.039157345192338155, 70.35805789912156172 ) ) ;
#46337 = ORIENTED_EDGE ( 'NONE', *, *, #23804, .T. ) ;
#46338 = ORIENTED_EDGE ( 'NONE', *, *, #19691, .T. ) ;
#46339 = CARTESIAN_POINT ( 'NONE',  ( -22.01784385650551812, -9.790100578890868377, 49.79778022625162492 ) ) ;
#46340 = ORIENTED_EDGE ( 'NONE', *, *, #17763, .F. ) ;
#46341 = DIRECTION ( 'NONE',  ( 1.352396030810764649E-06, 5.694414615768204918E-07, 0.9999999999989234167 ) ) ;
#46342 = AXIS2_PLACEMENT_3D ( 'NONE', #21424, #36406, #32491 ) ;
#46343 = CARTESIAN_POINT ( 'NONE',  ( -19.85891393954322837, -21.37210614461000446, 47.99999999999994316 ) ) ;
#46344 = PRODUCT_DEFINITION_FORMATION_WITH_SPECIFIED_SOURCE ( 'ANY', '', #42558, .NOT_KNOWN. ) ;
#46345 = EDGE_CURVE ( 'NONE', #34499, #24622, #23939, .T. ) ;
#46346 = ORIENTED_EDGE ( 'NONE', *, *, #3068, .T. ) ;
#46347 = AXIS2_PLACEMENT_3D ( 'NONE', #40430, #48540, #34006 ) ;
#46348 = AXIS2_PLACEMENT_3D ( 'NONE', #25888, #21950, #40902 ) ;
#46349 = CARTESIAN_POINT ( 'NONE',  ( -21.41781370759021641, -8.989828079956971862, 66.81716936885602820 ) ) ;
#46350 = CARTESIAN_POINT ( 'NONE',  ( -10.37878816232847967, -14.54793763971057174, 68.15240352950337410 ) ) ;
#46351 = ORIENTED_EDGE ( 'NONE', *, *, #1495, .T. ) ;
#46352 = CARTESIAN_POINT ( 'NONE',  ( -20.88821433888680446, -8.213514021607622340, 60.03399393531998385 ) ) ;
#46353 = CARTESIAN_POINT ( 'NONE',  ( -23.82261072958198511, -17.64831273128667632, 62.47360983446513671 ) ) ;
#46354 = ORIENTED_EDGE ( 'NONE', *, *, #8676, .F. ) ;
#46355 = CARTESIAN_POINT ( 'NONE',  ( -19.90583630033073703, -21.83377919204098205, 69.19128392610542733 ) ) ;
#46356 = CARTESIAN_POINT ( 'NONE',  ( -23.67397131994236759, -11.53905716532417536, 70.19210929491518414 ) ) ;
#46357 = ORIENTED_EDGE ( 'NONE', *, *, #22764, .F. ) ;
#46358 = CARTESIAN_POINT ( 'NONE',  ( -16.13263948075386978, -7.878200451182638453, 63.68483172840383588 ) ) ;
#46359 = CARTESIAN_POINT ( 'NONE',  ( -22.23155801786484176, -20.50065754255900075, 58.88630131417564684 ) ) ;
#46360 = CARTESIAN_POINT ( 'NONE',  ( -10.41531639268335496, -14.04517892474411589, 60.93293405735092705 ) ) ;
#46361 = VERTEX_POINT ( 'NONE', #5013 ) ;
#46362 = PLANE ( 'NONE',  #5802 ) ;
#46363 = EDGE_CURVE ( 'NONE', #40793, #40783, #2253, .T. ) ;
#46364 = DIRECTION ( 'NONE',  ( 2.866981220435666553E-17, -1.000000000000000000, -1.190614954331866791E-16 ) ) ;
#46365 = EDGE_CURVE ( 'NONE', #25227, #34833, #1473, .T. ) ;
#46366 = CARTESIAN_POINT ( 'NONE',  ( -11.55140690636466339, -10.22489917031350970, 71.09080336155108171 ) ) ;
#46367 = CARTESIAN_POINT ( 'NONE',  ( -35.32409385541306079, -2.423472813913224222, 48.79999999999998295 ) ) ;
#46368 = DIRECTION ( 'NONE',  ( -5.731567514496413899E-31, -1.020425574103664789E-16, -1.000000000000000000 ) ) ;
#46369 = CARTESIAN_POINT ( 'NONE',  ( -17.42409385541299471, -14.80920654474435771, 49.52966884056655772 ) ) ;
#46370 = FACE_OUTER_BOUND ( 'NONE', #11045, .T. ) ;
#46371 = CARTESIAN_POINT ( 'NONE',  ( -15.00927913818083859, -10.79274639537912783, 49.52966884056655772 ) ) ;
#46372 = EDGE_CURVE ( 'NONE', #15929, #6697, #46849, .T. ) ;
#46373 = CARTESIAN_POINT ( 'NONE',  ( -17.99909385759799108, -8.105421454601382081, 49.25000573077640098 ) ) ;
#46374 = CARTESIAN_POINT ( 'NONE',  ( -15.49284385650551421, -7.406986770994972602, 48.81910596585309747 ) ) ;
#46375 = EDGE_LOOP ( 'NONE', ( #20613, #4467 ) ) ;
#46376 = VECTOR ( 'NONE', #5167, 1000.000000000000000 ) ;
#46377 = CARTESIAN_POINT ( 'NONE',  ( -17.42409385541299471, -14.80920654474434883, 62.02966884056656482 ) ) ;
#46378 = CYLINDRICAL_SURFACE ( 'NONE', #31266, 0.1500000000000052125 ) ;
#46379 = ORIENTED_EDGE ( 'NONE', *, *, #11285, .F. ) ;
#46380 = DIRECTION ( 'NONE',  ( 0.9687793358424817702, -0.2479245821708686570, 0.000000000000000000 ) ) ;
#46381 = LINE ( 'NONE', #35278, #22765 ) ;
#46382 = CARTESIAN_POINT ( 'NONE',  ( -10.40888601095206134, -14.10966482229656194, 61.21821293885882653 ) ) ;
#46383 = LINE ( 'NONE', #45670, #15602 ) ;
#46384 = CARTESIAN_POINT ( 'NONE',  ( -14.62324732345129341, -21.22583884561250400, 58.23788065448412965 ) ) ;
#46385 = EDGE_CURVE ( 'NONE', #41672, #5421, #1600, .T. ) ;
#46386 = ORIENTED_EDGE ( 'NONE', *, *, #47511, .T. ) ;
#46387 = CARTESIAN_POINT ( 'NONE',  ( -24.80769062643263467, -15.80232089486973557, 69.71802876059763321 ) ) ;
#46388 = VECTOR ( 'NONE', #2458, 1000.000000000000000 ) ;
#46389 = CARTESIAN_POINT ( 'NONE',  ( -11.21157534608376061, -11.58358818987947814, 67.91864608155252370 ) ) ;
#46390 = CARTESIAN_POINT ( 'NONE',  ( -19.02448764833726713, -7.994547592594012819, 63.44591627019872959 ) ) ;
#46391 = VERTEX_POINT ( 'NONE', #1792 ) ;
#46392 = CARTESIAN_POINT ( 'NONE',  ( -18.59868636808265663, -22.16608242820997887, 72.47785073958938540 ) ) ;
#46393 = VECTOR ( 'NONE', #35535, 1000.000000000000000 ) ;
#46394 = CARTESIAN_POINT ( 'NONE',  ( -46.46711114793018282, -12.76354662275040042, 70.87000000000000455 ) ) ;
#46395 = CYLINDRICAL_SURFACE ( 'NONE', #32414, 4.686499999999997002 ) ;
#46396 = CARTESIAN_POINT ( 'NONE',  ( -16.53659385759799250, -8.995762431863214559, 51.38120296130585274 ) ) ;
#46397 = CARTESIAN_POINT ( 'NONE',  ( -45.88030547859645480, -14.20318880037429565, 71.05512804915051106 ) ) ;
#46398 = ORIENTED_EDGE ( 'NONE', *, *, #4985, .T. ) ;
#46399 = ORIENTED_EDGE ( 'NONE', *, *, #15889, .F. ) ;
#46400 = CARTESIAN_POINT ( 'NONE',  ( -20.10534385541304658, -7.595227055684746986, 51.75156210489594599 ) ) ;
#46401 = CARTESIAN_POINT ( 'NONE',  ( -20.89788161767221197, -20.94431024770144489, 62.39999296070408974 ) ) ;
#46402 = AXIS2_PLACEMENT_3D ( 'NONE', #30758, #42070, #45535 ) ;
#46403 =( REPRESENTATION_RELATIONSHIP ('NONE','NONE', #2768, #41459 ) REPRESENTATION_RELATIONSHIP_WITH_TRANSFORMATION ( #15385 )SHAPE_REPRESENTATION_RELATIONSHIP( ) );
#46404 = CARTESIAN_POINT ( 'NONE',  ( -19.99112905230247961, -8.296885111154901793, 73.72096600045514947 ) ) ;
#46405 = ADVANCED_FACE ( 'NONE', ( #47346 ), #13574, .T. ) ;
#46406 = CARTESIAN_POINT ( 'NONE',  ( -24.12071557656922494, -11.54438865435207795, 63.06722852297808402 ) ) ;
#46407 = CARTESIAN_POINT ( 'NONE',  ( -24.31285881818529404, -17.64644613426892406, 66.08323844663713942 ) ) ;
#46408 = VERTEX_POINT ( 'NONE', #46371 ) ;
#46409 = CIRCLE ( 'NONE', #29100, 5.500000000000000000 ) ;
#46410 = PLANE ( 'NONE',  #22912 ) ;
#46411 = VECTOR ( 'NONE', #11644, 1000.000000000000114 ) ;
#46412 = CARTESIAN_POINT ( 'NONE',  ( -24.41841346439724347, -17.37497344050957437, 69.45693887357894880 ) ) ;
#46413 = VERTEX_POINT ( 'NONE', #8948 ) ;
#46414 =( BOUNDED_CURVE ( )  B_SPLINE_CURVE ( 3, ( #42732, #42243, #16106, #8999 ),
 .UNSPECIFIED., .F., .F. ) 
 B_SPLINE_CURVE_WITH_KNOTS ( ( 4, 4 ),
 ( 0.9074455897393669535, 1.000000000000000000 ),
 .UNSPECIFIED. ) 
 CURVE ( )  GEOMETRIC_REPRESENTATION_ITEM ( )  RATIONAL_B_SPLINE_CURVE ( ( 0.6983129098260874024, 0.7760317562606933173, 0.8765941196519975165, 1.000000000000000000 ) ) 
 REPRESENTATION_ITEM ( '' )  );
#46415 = CARTESIAN_POINT ( 'NONE',  ( -21.31800817620502286, -20.62620158190326336, 72.82446429882371319 ) ) ;
#46416 = EDGE_CURVE ( 'NONE', #17241, #2873, #14461, .T. ) ;
#46417 = CARTESIAN_POINT ( 'NONE',  ( -27.42409385541305511, -15.80920654474410725, 63.99999999999998579 ) ) ;
#46418 = ORIENTED_EDGE ( 'NONE', *, *, #34795, .F. ) ;
#46419 = FACE_OUTER_BOUND ( 'NONE', #25741, .T. ) ;
#46420 = LINE ( 'NONE', #38528, #3768 ) ;
#46421 = ORIENTED_EDGE ( 'NONE', *, *, #45220, .F. ) ;
#46422 = CARTESIAN_POINT ( 'NONE',  ( -13.90356134367569041, -20.91730929552939600, 68.75625110435674969 ) ) ;
#46423 = CARTESIAN_POINT ( 'NONE',  ( -10.00684590941331820, -15.50754077729470559, 57.67454502885500034 ) ) ;
#46424 = CIRCLE ( 'NONE', #6346, 0.5560000000000009379 ) ;
#46425 = CARTESIAN_POINT ( 'NONE',  ( -21.47456293661849713, -9.038556783377254433, 70.41660404402310292 ) ) ;
#46426 = CARTESIAN_POINT ( 'NONE',  ( -24.49056774983930751, -17.16914905338390085, 73.06052939366072962 ) ) ;
#46427 = ORIENTED_EDGE ( 'NONE', *, *, #47501, .F. ) ;
#46428 = CARTESIAN_POINT ( 'NONE',  ( -10.32823143149344247, -17.07887373198904513, 57.78736918859686966 ) ) ;
#46429 = LINE ( 'NONE', #12684, #36808 ) ;
#46431 =( BOUNDED_CURVE ( )  B_SPLINE_CURVE ( 3, ( #13024, #46295, #24376, #34950 ),
 .UNSPECIFIED., .F., .F. ) 
 B_SPLINE_CURVE_WITH_KNOTS ( ( 4, 4 ),
 ( 0.5000000000000000000, 0.9074455897393624015 ),
 .UNSPECIFIED. ) 
 CURVE ( )  GEOMETRIC_REPRESENTATION_ITEM ( )  RATIONAL_B_SPLINE_CURVE ( ( 1.000000000000003109, 0.4567392136813368531, 0.3561768502900296562, 0.6983129098260851819 ) ) 
 REPRESENTATION_ITEM ( '' )  );
#46430 = DIRECTION ( 'NONE',  ( 0.8603395911234834603, 0.5097212845717522534, 0.000000000000000000 ) ) ;
#46432 = CARTESIAN_POINT ( 'NONE',  ( -10.99586697244644640, -11.04334986774487781, 60.86381167495338929 ) ) ;
#46433 = EDGE_CURVE ( 'NONE', #42239, #11354, #43221, .T. ) ;
#46434 = CARTESIAN_POINT ( 'NONE',  ( -22.79734409636068904, -10.24514240368273477, 66.54182257473807738 ) ) ;
#46435 = CARTESIAN_POINT ( 'NONE',  ( -17.73278501768472992, -7.757988417614677168, 67.16472282884072342 ) ) ;
#46436 = CYLINDRICAL_SURFACE ( 'NONE', #6203, 0.1499999999999974132 ) ;
#46437 = VERTEX_POINT ( 'NONE', #24457 ) ;
#46438 = CARTESIAN_POINT ( 'NONE',  ( 18.57590614458706924, 1.637040139411203965, 51.75426295951086075 ) ) ;
#46439 = ADVANCED_FACE ( 'NONE', ( #24923 ), #48528, .T. ) ;
#46440 = ORIENTED_EDGE ( 'NONE', *, *, #18264, .T. ) ;
#46441 = CARTESIAN_POINT ( 'NONE',  ( -11.45751978572037011, -19.27057081285444085, 71.87181161472111057 ) ) ;
#46442 = CARTESIAN_POINT ( 'NONE',  ( -13.14998806103231566, -9.265559761403904915, 67.67942786032521951 ) ) ;
#46443 = VERTEX_POINT ( 'NONE', #10398 ) ;
#46444 = DIRECTION ( 'NONE',  ( 0.9163203205182083311, 0.4004460890125009498, -2.380681616944615543E-09 ) ) ;
#46445 = CARTESIAN_POINT ( 'NONE',  ( -12.70413878835906729, -9.045123344351514660, 71.04914126506433547 ) ) ;
#46446 = EDGE_LOOP ( 'NONE', ( #39794, #8825, #17874, #37460 ) ) ;
#46447 = EDGE_LOOP ( 'NONE', ( #21627, #3604, #17573, #36950, #4549, #5846, #12165 ) ) ;
#46448 = VERTEX_POINT ( 'NONE', #40418 ) ;
#46450 = CARTESIAN_POINT ( 'NONE',  ( -10.03035355355731006, -15.72374577095404824, 61.22284339518546403 ) ) ;
#46449 = AXIS2_PLACEMENT_3D ( 'NONE', #43518, #43758, #39807 ) ;
#46451 = LINE ( 'NONE', #16389, #1984 ) ;
#46452 = CARTESIAN_POINT ( 'NONE',  ( -21.94239175829699207, -20.22099772874085488, 59.06442899522711798 ) ) ;
#46453 = EDGE_CURVE ( 'NONE', #4771, #956, #30403, .T. ) ;
#46454 = DIRECTION ( 'NONE',  ( 1.056002951008363407E-14, 0.000000000000000000, -1.000000000000000000 ) ) ;
#46455 = B_SPLINE_CURVE_WITH_KNOTS ( 'NONE', 3,
 ( #7540, #45218, #48158, #41256, #14390, #44479, #22548, #37543, #3845, #10730 ),
 .UNSPECIFIED., .F., .F.,
 ( 4, 2, 2, 2, 4 ),
 ( 0.1272669073657964056, 0.2522669073487617819, 0.3772669073317270749, 0.5022669073146924790, 0.6272669072976577720 ),
 .UNSPECIFIED. ) ;
#46456 = CARTESIAN_POINT ( 'NONE',  ( -10.70785606720758487, -16.78775419186948881, 57.79833654845999291 ) ) ;
#46457 = AXIS2_PLACEMENT_3D ( 'NONE', #38248, #4530, #34566 ) ;
#46458 = EDGE_CURVE ( 'NONE', #1265, #41721, #31399, .T. ) ;
#46459 = ORIENTED_EDGE ( 'NONE', *, *, #27817, .F. ) ;
#46460 = ORIENTED_EDGE ( 'NONE', *, *, #39737, .F. ) ;
#46461 = CARTESIAN_POINT ( 'NONE',  ( -20.41784385650551314, -9.790100578890868377, 49.79778022625163203 ) ) ;
#46462 = EDGE_CURVE ( 'NONE', #22244, #35282, #47120, .T. ) ;
#46463 = EDGE_CURVE ( 'NONE', #37281, #47436, #47914, .T. ) ;
#46464 = CARTESIAN_POINT ( 'NONE',  ( -11.39127492490111315, -11.16067319722467843, 60.69357916181100876 ) ) ;
#46465 = CARTESIAN_POINT ( 'NONE',  ( -45.92409385541306222, -14.90920654474410867, 70.50000000000000000 ) ) ;
#46466 = AXIS2_PLACEMENT_3D ( 'NONE', #30241, #41549, #8545 ) ;
#46467 = CARTESIAN_POINT ( 'NONE',  ( -23.27053873564116770, -18.65887406133006010, 66.05062667540605048 ) ) ;
#46468 = CARTESIAN_POINT ( 'NONE',  ( -13.52409385650551599, -6.426201560718813433, 50.50509628382439331 ) ) ;
#46469 = ORIENTED_EDGE ( 'NONE', *, *, #30646, .F. ) ;
#46470 = DIRECTION ( 'NONE',  ( 0.2122660683108583690, -0.9772119095896469876, 7.504255179194988334E-08 ) ) ;
#46471 = DIRECTION ( 'NONE',  ( -1.000000000000000000, 0.000000000000000000, 0.000000000000000000 ) ) ;
#46472 = AXIS2_PLACEMENT_3D ( 'NONE', #12849, #38955, #20499 ) ;
#46474 = DIRECTION ( 'NONE',  ( -0.3478314405900341799, -0.9375570856950852239, 0.000000000000000000 ) ) ;
#46473 = B_SPLINE_CURVE_WITH_KNOTS ( 'NONE', 3,
 ( #33319, #32846, #24997, #2816, #48126, #25965, #33079, #29655, #44691, #3057 ),
 .UNSPECIFIED., .F., .F.,
 ( 4, 2, 2, 2, 4 ),
 ( 0.1272669073658475869, 0.2522669073463348899, 0.3772669073268222206, 0.5022669073073094959, 0.6272669072877967711 ),
 .UNSPECIFIED. ) ;
#46475 = ORIENTED_EDGE ( 'NONE', *, *, #17610, .F. ) ;
#46476 = CARTESIAN_POINT ( 'NONE',  ( -15.48261606618132546, -10.53062973237823918, 52.02966884056656482 ) ) ;
#46477 = B_SPLINE_CURVE_WITH_KNOTS ( 'NONE', 1,
 ( #38302, #26037 ),
 .UNSPECIFIED., .F., .F.,
 ( 2, 2 ),
 ( 0.000000000000000000, 1.000000000000000000 ),
 .UNSPECIFIED. ) ;
#46478 = AXIS2_PLACEMENT_3D ( 'NONE', #12469, #34873, #15914 ) ;
#46479 = CARTESIAN_POINT ( 'NONE',  ( -10.40121522062585591, -17.29573862802152817, 61.20097198354311274 ) ) ;
#46480 = CARTESIAN_POINT ( 'NONE',  ( -22.11331555132107241, -9.020036405104091770, 63.29879605510286922 ) ) ;
#46481 = CARTESIAN_POINT ( 'NONE',  ( -24.17580812652340683, -11.65980397366943855, 59.65952650191913875 ) ) ;
#46482 = CIRCLE ( 'NONE', #25249, 2.000000000000001332 ) ;
#46483 = ORIENTED_EDGE ( 'NONE', *, *, #1246, .F. ) ;
#46484 = DIRECTION ( 'NONE',  ( -5.731567514496413899E-31, -1.020425574103664789E-16, -1.000000000000000000 ) ) ;
#46485 = CARTESIAN_POINT ( 'NONE',  ( -24.82755346431643417, -15.64070656656598857, 73.20314952539401077 ) ) ;
#46486 = CARTESIAN_POINT ( 'NONE',  ( -11.44812054352227193, -18.45465371200965166, 61.27710877960604563 ) ) ;
#46487 = EDGE_LOOP ( 'NONE', ( #6833, #36109 ) ) ;
#46488 = CARTESIAN_POINT ( 'NONE',  ( -10.00731251637046881, -14.10555026099538978, 61.10316585833331260 ) ) ;
#46489 = VECTOR ( 'NONE', #31342, 1000.000000000000000 ) ;
#46490 = ORIENTED_EDGE ( 'NONE', *, *, #13647, .T. ) ;
#46491 = DIRECTION ( 'NONE',  ( 0.000000000000000000, -0.9999954153791273948, -0.003028072113819838245 ) ) ;
#46492 = FACE_OUTER_BOUND ( 'NONE', #3530, .T. ) ;
#46494 = EDGE_CURVE ( 'NONE', #23020, #18740, #39791, .T. ) ;
#46493 = ORIENTED_EDGE ( 'NONE', *, *, #2846, .T. ) ;
#46495 = DIRECTION ( 'NONE',  ( 0.000000000000000000, 1.000000000000000000, 0.000000000000000000 ) ) ;
#46496 = CARTESIAN_POINT ( 'NONE',  ( -10.37762151648083808, -12.38827872426728050, 57.44202070861023657 ) ) ;
#46497 = CARTESIAN_POINT ( 'NONE',  ( -24.25757915753366589, -13.28409016433970535, 63.02191351886040138 ) ) ;
#46498 = DIRECTION ( 'NONE',  ( 0.000000000000000000, 0.000000000000000000, 1.000000000000000000 ) ) ;
#46499 = ORIENTED_EDGE ( 'NONE', *, *, #42074, .F. ) ;
#46500 = CARTESIAN_POINT ( 'NONE',  ( -22.41668094288463919, -16.43295965837073780, 52.02966884056656482 ) ) ;
#46501 = VECTOR ( 'NONE', #25486, 1000.000000000000000 ) ;
#46502 = DIRECTION ( 'NONE',  ( 0.8402231219892249969, -0.5322911103758141138, 0.1033986416233923511 ) ) ;
#46503 = CARTESIAN_POINT ( 'NONE',  ( -23.42121016340660233, -19.22949192118923989, 62.53219661271650409 ) ) ;
#46504 = VERTEX_POINT ( 'NONE', #10148 ) ;
#46505 = DIRECTION ( 'NONE',  ( 0.000000000000000000, 0.000000000000000000, 1.000000000000000000 ) ) ;
#46506 = CARTESIAN_POINT ( 'NONE',  ( -11.14144638094932382, -18.81445342923831987, 61.39055447797494480 ) ) ;
#46508 = ORIENTED_EDGE ( 'NONE', *, *, #19567, .F. ) ;
#46507 = AXIS2_PLACEMENT_3D ( 'NONE', #34399, #4880, #16418 ) ;
#46509 = ORIENTED_EDGE ( 'NONE', *, *, #25593, .F. ) ;
#46510 = CARTESIAN_POINT ( 'NONE',  ( -23.83080496556880945, -17.75212211224490133, 59.28906343887996400 ) ) ;
#46511 = CARTESIAN_POINT ( 'NONE',  ( -13.07136565370527315, -8.762923774744256988, 64.02451247989536398 ) ) ;
#46512 = DIRECTION ( 'NONE',  ( 0.000000000000000000, 0.9999954153791273948, 0.003028072113819836077 ) ) ;
#46513 = SHAPE_REPRESENTATION ( 'Base Cast Iron Chassis Plate', ( #29031 ), #39238 ) ;
#46514 = CARTESIAN_POINT ( 'NONE',  ( -16.78659385650551883, -9.302874398569244363, 51.68646062012417985 ) ) ;
#46515 = CARTESIAN_POINT ( 'NONE',  ( -12.35435101773841993, -9.982347803354048921, 57.31608956411530187 ) ) ;
#46516 = B_SPLINE_CURVE_WITH_KNOTS ( 'NONE', 3,
 ( #39340, #46967, #47696, #14174, #40314, #44501, #6818, #28745, #6090, #28509 ),
 .UNSPECIFIED., .F., .F.,
 ( 4, 2, 2, 2, 4 ),
 ( 0.6272669072877915530, 0.7522669073073021684, 0.8772669073268128948, 1.002266907346323510, 1.127266907365834125 ),
 .UNSPECIFIED. ) ;
#46517 = CARTESIAN_POINT ( 'NONE',  ( -19.72726371358324471, -21.89426820971140941, 65.56511966726597507 ) ) ;
#46518 = EDGE_CURVE ( 'NONE', #20335, #29820, #30652, .T. ) ;
#46519 = CARTESIAN_POINT ( 'NONE',  ( -23.25646303129147441, -19.44570675813884009, 59.07065992548621125 ) ) ;
#46520 = ORIENTED_EDGE ( 'NONE', *, *, #35920, .T. ) ;
#46521 = ORIENTED_EDGE ( 'NONE', *, *, #41812, .T. ) ;
#46522 = VECTOR ( 'NONE', #41614, 1000.000000000000227 ) ;
#46523 = EDGE_CURVE ( 'NONE', #37668, #46893, #14046, .T. ) ;
#46524 = EDGE_CURVE ( 'NONE', #8094, #41701, #43304, .T. ) ;
#46525 =( NAMED_UNIT ( * ) PLANE_ANGLE_UNIT ( ) SI_UNIT ( $, .RADIAN. ) );
#46526 = VECTOR ( 'NONE', #48601, 1000.000000000000000 ) ;
#46527 = DIRECTION ( 'NONE',  ( -3.071710424422018668E-17, 6.404604876783312462E-16, 1.000000000000000000 ) ) ;
#46528 = LINE ( 'NONE', #9336, #45308 ) ;
#46529 = CARTESIAN_POINT ( 'NONE',  ( -21.84435842615539158, -9.381383662134735957, 59.83057260011872103 ) ) ;
#46530 = AXIS2_PLACEMENT_3D ( 'NONE', #27448, #5547, #35068 ) ;
#46531 = ADVANCED_FACE ( 'NONE', ( #3235 ), #47808, .T. ) ;
#46532 = VERTEX_POINT ( 'NONE', #25637 ) ;
#46533 = CARTESIAN_POINT ( 'NONE',  ( -11.96084830514426400, -9.743959610980004626, 60.74413522332266524 ) ) ;
#46534 = CARTESIAN_POINT ( 'NONE',  ( -12.96755856236231885, -20.27663165334763917, 72.01473639041756769 ) ) ;
#46535 = B_SPLINE_CURVE_WITH_KNOTS ( 'NONE', 1,
 ( #14254, #7645 ),
 .UNSPECIFIED., .F., .F.,
 ( 2, 2 ),
 ( 0.000000000000000000, 1.000000000000000000 ),
 .UNSPECIFIED. ) ;
#46536 = CARTESIAN_POINT ( 'NONE',  ( -22.00117057250496444, -9.443090202341716477, 63.60642510345682155 ) ) ;
#46537 = DIRECTION ( 'NONE',  ( 0.9687793358424821033, -0.2479245821708678243, 0.000000000000000000 ) ) ;
#46538 = VECTOR ( 'NONE', #7524, 1000.000000000000000 ) ;
#46539 = ORIENTED_EDGE ( 'NONE', *, *, #43117, .F. ) ;
#46540 = CARTESIAN_POINT ( 'NONE',  ( -10.54357723031444216, -16.09736363853215479, 68.26302419364235163 ) ) ;
#46541 = CARTESIAN_POINT ( 'NONE',  ( -24.02329229792678689, -17.28986148198579187, 69.41339790474248161 ) ) ;
#46542 = EDGE_CURVE ( 'NONE', #32302, #11500, #29772, .T. ) ;
#46543 = VECTOR ( 'NONE', #40413, 1000.000000000000000 ) ;
#46544 = VERTEX_POINT ( 'NONE', #29836 ) ;
#46545 = CARTESIAN_POINT ( 'NONE',  ( -22.62539314545485780, -20.14320100466526497, 69.31384596586300972 ) ) ;
#46546 = CARTESIAN_POINT ( 'NONE',  ( -24.22220026926100545, -16.48362040234153625, 59.35162391529105008 ) ) ;
#46547 = VERTEX_POINT ( 'NONE', #26879 ) ;
#46548 = B_SPLINE_CURVE_WITH_KNOTS ( 'NONE', 3,
 ( #40398, #28365, #39917, #25617, #2246, #6187, #10125, #47071, #2495, #25148 ),
 .UNSPECIFIED., .F., .F.,
 ( 4, 2, 2, 2, 4 ),
 ( 0.000000000000000000, 0.2500000000000000000, 0.5000000000000000000, 0.7500000000000000000, 1.000000000000000000 ),
 .UNSPECIFIED. ) ;
#46549 = CARTESIAN_POINT ( 'NONE',  ( -18.92409385541305511, -15.80920654474410725, 48.99999999999997868 ) ) ;
#46550 = ORIENTED_EDGE ( 'NONE', *, *, #24708, .F. ) ;
#46551 = DIRECTION ( 'NONE',  ( 0.9687793358424821033, -0.2479245821708680464, 0.000000000000000000 ) ) ;
#46553 = CARTESIAN_POINT ( 'NONE',  ( -17.43166586245951422, -7.359124596637800053, 67.13544155391683432 ) ) ;
#46552 = VECTOR ( 'NONE', #37282, 1000.000000000000114 ) ;
#46554 = VERTEX_POINT ( 'NONE', #45600 ) ;
#46555 = CARTESIAN_POINT ( 'NONE',  ( -10.69843886630479624, -16.92312086968962603, 57.68760564129097901 ) ) ;
#46556 = CARTESIAN_POINT ( 'NONE',  ( -15.58034385650551634, -6.424090610841176385, 49.80797279389978627 ) ) ;
#46557 = ORIENTED_EDGE ( 'NONE', *, *, #36111, .F. ) ;
#46558 = CARTESIAN_POINT ( 'NONE',  ( -17.86643106983121498, -7.822757629381109190, 60.36444193307492156 ) ) ;
#46559 =( BOUNDED_SURFACE ( )  B_SPLINE_SURFACE ( 3, 1, ( 
 ( #38516, #15612 ),
 ( #11949, #41982 ),
 ( #860, #4542 ),
 ( #12181, #27198 ),
 ( #42223, #23516 ),
 ( #38761, #4798 ),
 ( #19823, #34819 ) ),
 .UNSPECIFIED., .T., .F., .F. ) 
 B_SPLINE_SURFACE_WITH_KNOTS ( ( 4, 3, 4 ),
 ( 2, 2 ),
 ( 0.000000000000000000, 0.5000000000000000000, 1.000000000000000000 ),
 ( 0.000000000000000000, 1.000000000000000000 ),
 .UNSPECIFIED. ) 
 GEOMETRIC_REPRESENTATION_ITEM ( )  RATIONAL_B_SPLINE_SURFACE ( (
 ( 1.000000000000000000, 1.000000000000000000),
 ( 0.3333333333333335369, 0.3333333333333330373),
 ( 0.3333333333333335369, 0.3333333333333330373),
 ( 1.000000000000000000, 1.000000000000000000),
 ( 0.3333333333333333703, 0.3333333333333333703),
 ( 0.3333333333333333703, 0.3333333333333333703),
 ( 1.000000000000000000, 1.000000000000000000) ) ) 
 REPRESENTATION_ITEM ( '' )  SURFACE ( )  );
#46560 = CARTESIAN_POINT ( 'NONE',  ( -15.28630342961327138, -8.082779564739171363, 56.99432743296591042 ) ) ;
#46561 = DIRECTION ( 'NONE',  ( -5.731567514496413899E-31, -1.020425574103664789E-16, -1.000000000000000000 ) ) ;
#46562 = EDGE_LOOP ( 'NONE', ( #35555, #1972, #36676, #3023, #18418 ) ) ;
#46563 = CARTESIAN_POINT ( 'NONE',  ( -21.53861794036900079, -21.02004141303368101, 72.63951040967180006 ) ) ;
#46564 = CARTESIAN_POINT ( 'NONE',  ( -10.29385348138020539, -12.64970417265235803, 64.38340698725603772 ) ) ;
#46565 = CARTESIAN_POINT ( 'NONE',  ( -11.73296596577226936, -10.64774513788296417, 74.72412863062541533 ) ) ;
#46566 = CARTESIAN_POINT ( 'NONE',  ( -35.32409385541306079, -25.10920654474410441, 52.29999999999998295 ) ) ;
#46567 = CARTESIAN_POINT ( 'NONE',  ( -12.46122051107220408, -19.81685944811288991, 64.88146935704573082 ) ) ;
#46568 = ORIENTED_EDGE ( 'NONE', *, *, #27071, .T. ) ;
#46569 = ORIENTED_EDGE ( 'NONE', *, *, #39883, .T. ) ;
#46570 = CARTESIAN_POINT ( 'NONE',  ( -20.54979492810923603, -8.489990406890694175, 63.46121512946601229 ) ) ;
#46571 = CARTESIAN_POINT ( 'NONE',  ( -24.28086713618749570, -13.15448386353826926, 66.39426969126174072 ) ) ;
#46572 = ORIENTED_EDGE ( 'NONE', *, *, #36498, .F. ) ;
#46573 = CARTESIAN_POINT ( 'NONE',  ( -10.40860991809309155, -15.50898095412354571, 57.85320721669017985 ) ) ;
#46574 = CARTESIAN_POINT ( 'NONE',  ( -19.41474593944376537, -21.52019035999878938, 61.99503644832097393 ) ) ;
#46575 = CARTESIAN_POINT ( 'NONE',  ( -22.61159385759798823, -8.990409506049200417, 49.61344411288074951 ) ) ;
#46576 = CARTESIAN_POINT ( 'NONE',  ( -13.08279692198261479, -8.754610786518940202, 64.07093076773905693 ) ) ;
#46577 = CARTESIAN_POINT ( 'NONE',  ( -11.22844613476422282, -11.44458948612160221, 64.43409918096024569 ) ) ;
#46578 =( BOUNDED_CURVE ( )  B_SPLINE_CURVE ( 3, ( #19109, #173, #639, #45466 ),
 .UNSPECIFIED., .F., .F. ) 
 B_SPLINE_CURVE_WITH_KNOTS ( ( 4, 4 ),
 ( 4.712388980384689674, 4.921828490624010399 ),
 .UNSPECIFIED. ) 
 CURVE ( )  GEOMETRIC_REPRESENTATION_ITEM ( )  RATIONAL_B_SPLINE_CURVE ( ( 1.000000000000000000, 0.9963479302455154896, 0.9963479302455154896, 1.000000000000000000 ) ) 
 REPRESENTATION_ITEM ( '' )  );
#46579 = EDGE_LOOP ( 'NONE', ( #28176, #17598, #45958, #42548, #17374 ) ) ;
#46580 = EDGE_CURVE ( 'NONE', #42076, #28542, #41553, .T. ) ;
#46581 = CARTESIAN_POINT ( 'NONE',  ( -19.17403394478084522, -7.567564808342563509, 63.47443287871421091 ) ) ;
#46582 = LINE ( 'NONE', #9389, #44420 ) ;
#46583 = CARTESIAN_POINT ( 'NONE',  ( -22.85860156586533165, -9.713020250643273457, 73.64307581635257804 ) ) ;
#46584 = CARTESIAN_POINT ( 'NONE',  ( -12.10131192688100477, -10.18592936015514638, 64.31442259820508411 ) ) ;
#46585 = VERTEX_POINT ( 'NONE', #41389 ) ;
#46586 = ORIENTED_EDGE ( 'NONE', *, *, #2872, .F. ) ;
#46587 =( BOUNDED_SURFACE ( )  B_SPLINE_SURFACE ( 3, 1, ( 
 ( #17800, #32825 ),
 ( #47863, #29147 ),
 ( #44197, #25455 ),
 ( #7243, #22246 ),
 ( #6983, #331 ),
 ( #7731, #34282 ),
 ( #37000, #37735 ) ),
 .UNSPECIFIED., .T., .F., .F. ) 
 B_SPLINE_SURFACE_WITH_KNOTS ( ( 4, 3, 4 ),
 ( 2, 2 ),
 ( 0.000000000000000000, 0.5000000000000000000, 1.000000000000000000 ),
 ( 0.000000000000000000, 1.000000000000000000 ),
 .UNSPECIFIED. ) 
 GEOMETRIC_REPRESENTATION_ITEM ( )  RATIONAL_B_SPLINE_SURFACE ( (
 ( 1.000000000000000000, 1.000000000000000000),
 ( 0.3333333333333335369, 0.3333333333333330373),
 ( 0.3333333333333335369, 0.3333333333333330373),
 ( 1.000000000000000000, 1.000000000000000000),
 ( 0.3333333333333333703, 0.3333333333333333703),
 ( 0.3333333333333333703, 0.3333333333333333703),
 ( 1.000000000000000000, 1.000000000000000000) ) ) 
 REPRESENTATION_ITEM ( '' )  SURFACE ( )  );
#46588 = EDGE_CURVE ( 'NONE', #2110, #3303, #8166, .T. ) ;
#46589 = EDGE_CURVE ( 'NONE', #30760, #37238, #7681, .T. ) ;
#46590 = VERTEX_POINT ( 'NONE', #18735 ) ;
#46591 = CARTESIAN_POINT ( 'NONE',  ( -17.83128375312269753, -10.14042954887026049, 49.52966884056655772 ) ) ;
#46592 = ADVANCED_FACE ( 'NONE', ( #26373 ), #11119, .T. ) ;
#46593 = DIRECTION ( 'NONE',  ( -5.731567514496413899E-31, -1.020425574103664789E-16, -1.000000000000000000 ) ) ;
#46594 = ADVANCED_FACE ( 'NONE', ( #7928 ), #22692, .T. ) ;
#46595 = ORIENTED_EDGE ( 'NONE', *, *, #40163, .F. ) ;
#46596 = CARTESIAN_POINT ( 'NONE',  ( -21.84891708756835982, -9.316868653145983004, 67.07638807817237137 ) ) ;
#46597 = DIRECTION ( 'NONE',  ( 1.000000000000000000, -4.164305804376849172E-17, 1.614929280266638808E-16 ) ) ;
#46598 = EDGE_CURVE ( 'NONE', #28666, #6771, #40, .T. ) ;
#46599 = ORIENTED_EDGE ( 'NONE', *, *, #19708, .F. ) ;
#46600 = CARTESIAN_POINT ( 'NONE',  ( -23.12302852889638061, -18.95946475466559633, 62.65406880579606508 ) ) ;
#46601 = CARTESIAN_POINT ( 'NONE',  ( -19.37616744185158879, -21.99900390342548206, 58.71002665166666645 ) ) ;
#46602 = ORIENTED_EDGE ( 'NONE', *, *, #40191, .T. ) ;
#46603 = CARTESIAN_POINT ( 'NONE',  ( -11.37640567311080453, -11.28103864939108902, 64.33809173091806599 ) ) ;
#46604 = ORIENTED_EDGE ( 'NONE', *, *, #11375, .T. ) ;
#46605 = CARTESIAN_POINT ( 'NONE',  ( -10.58039871790519726, -13.33820790931908284, 71.39931681139518105 ) ) ;
#46606 = ORIENTED_EDGE ( 'NONE', *, *, #31582, .F. ) ;
#46607 = CARTESIAN_POINT ( 'NONE',  ( -24.43113015230203544, -15.58634353390661964, 73.15303748141660378 ) ) ;
#46608 = CARTESIAN_POINT ( 'NONE',  ( -16.85302834907681557, -22.23803867529147738, 68.80905311428833215 ) ) ;
#46609 = CARTESIAN_POINT ( 'NONE',  ( -20.84119746710918974, -20.97572115929791892, 62.11471400470772863 ) ) ;
#46610 = VERTEX_POINT ( 'NONE', #30088 ) ;
#46611 = CARTESIAN_POINT ( 'NONE',  ( -24.23636277187043220, -17.82529184948975498, 62.58865552117998021 ) ) ;
#46612 = CARTESIAN_POINT ( 'NONE',  ( -24.42218830512229388, -14.64588455312011739, 63.01296487252135137 ) ) ;
#46613 = CARTESIAN_POINT ( 'NONE',  ( -24.08281607949275127, -11.46758912624300919, 63.09071781931947953 ) ) ;
#46614 = CARTESIAN_POINT ( 'NONE',  ( -10.46375287308303648, -15.55739392218797512, 61.05405700252866552 ) ) ;
#46615 = CARTESIAN_POINT ( 'NONE',  ( -20.64396844604977233, -21.02470390210128670, 58.64475165022597025 ) ) ;
#46616 = ORIENTED_EDGE ( 'NONE', *, *, #30362, .F. ) ;
#46617 = CARTESIAN_POINT ( 'NONE',  ( -17.45675080712947036, -7.809221453984609873, 63.77730436730185914 ) ) ;
#46618 = CARTESIAN_POINT ( 'NONE',  ( -11.68775437312510235, -10.05546324315060858, 67.54250946422081370 ) ) ;
#46619 = CARTESIAN_POINT ( 'NONE',  ( -50.42609385541305755, -14.90920654474411577, 58.00588235294116402 ) ) ;
#46620 = CARTESIAN_POINT ( 'NONE',  ( -14.54749350918766204, -8.372447261038935551, 64.07506791522041567 ) ) ;
#46621 = CARTESIAN_POINT ( 'NONE',  ( -19.97822118923243195, -21.80783213648190610, 69.05669729689820713 ) ) ;
#46622 = CARTESIAN_POINT ( 'NONE',  ( -15.83034385650551634, -9.794322478646142471, 51.19202720610083190 ) ) ;
#46623 = ORIENTED_EDGE ( 'NONE', *, *, #6962, .T. ) ;
#46624 = PLANE ( 'NONE',  #27470 ) ;
#46625 = DIRECTION ( 'NONE',  ( 0.000000000000000000, 0.000000000000000000, 1.000000000000000000 ) ) ;
#46626 = VERTEX_POINT ( 'NONE', #22948 ) ;
#46627 = FACE_OUTER_BOUND ( 'NONE', #40400, .T. ) ;
#46628 = CARTESIAN_POINT ( 'NONE',  ( -12.21634942047498384, -14.14445252980938861, 49.52966884056655772 ) ) ;
#46629 = CARTESIAN_POINT ( 'NONE',  ( -17.92307556733882379, -22.24252716037962330, 62.06874222216396220 ) ) ;
#46630 = DIRECTION ( 'NONE',  ( -1.224646799147353207E-16, -1.000000000000000000, 1.912410701131276611E-32 ) ) ;
#46631 = CARTESIAN_POINT ( 'NONE',  ( -17.42409385541305511, -14.80920654474410725, 52.21286476528345588 ) ) ;
#46632 = ADVANCED_FACE ( 'NONE', ( #37689 ), #45509, .T. ) ;
#46633 = ORIENTED_EDGE ( 'NONE', *, *, #22565, .F. ) ;
#46634 = CARTESIAN_POINT ( 'NONE',  ( -24.80967279009360027, -15.78810072853396917, 69.69340815245216447 ) ) ;
#46635 = DIRECTION ( 'NONE',  ( 0.5022914217388751990, -0.8646984027090225400, -6.766381832589513682E-08 ) ) ;
#46636 = CARTESIAN_POINT ( 'NONE',  ( -19.02482722938969317, -7.994625824363213340, 63.71623835456152563 ) ) ;
#46637 = EDGE_CURVE ( 'NONE', #39973, #22327, #40814, .T. ) ;
#46638 = ORIENTED_EDGE ( 'NONE', *, *, #11941, .T. ) ;
#46639 = CARTESIAN_POINT ( 'NONE',  ( -16.86460949297358525, -7.773444642497263857, 70.64603134899243742 ) ) ;
#46640 = CARTESIAN_POINT ( 'NONE',  ( -23.49719359612965519, -11.32496190889342813, 73.55120448430523084 ) ) ;
#46641 = CARTESIAN_POINT ( 'NONE',  ( -36.42409385541304800, -6.859212275519750435, 50.50378509014258555 ) ) ;
#46642 = CARTESIAN_POINT ( 'NONE',  ( -15.68875476689939852, -7.563362019294005201, 70.79645224690898431 ) ) ;
#46643 = CARTESIAN_POINT ( 'NONE',  ( -14.67111564601650997, -7.886426081561471513, 60.43500846974642116 ) ) ;
#46644 = EDGE_LOOP ( 'NONE', ( #4133, #8874 ) ) ;
#46645 = EDGE_LOOP ( 'NONE', ( #41066, #37531 ) ) ;
#46646 = CARTESIAN_POINT ( 'NONE',  ( -21.84909385541304161, -8.112991634885936776, 51.74999426922421719 ) ) ;
#46647 = CARTESIAN_POINT ( 'NONE',  ( -23.07906183844443859, -9.958936969296642516, 66.72677665813928627 ) ) ;
#46648 = VECTOR ( 'NONE', #24512, 1000.000000000000227 ) ;
#46649 = EDGE_CURVE ( 'NONE', #16353, #31311, #19762, .T. ) ;
#46650 = CARTESIAN_POINT ( 'NONE',  ( -20.64396844604977233, -21.02470390210128670, 58.64475165022597025 ) ) ;
#46651 = ADVANCED_FACE ( 'NONE', ( #23669 ), #1967, .T. ) ;
#46652 = CARTESIAN_POINT ( 'NONE',  ( -11.45751978572037011, -19.27057081285444085, 71.87181161472111057 ) ) ;
#46653 = EDGE_CURVE ( 'NONE', #42260, #16178, #20960, .T. ) ;
#46654 = CARTESIAN_POINT ( 'NONE',  ( -24.45013009618349642, -14.22792902121458170, 69.95275266250405366 ) ) ;
#46655 = CARTESIAN_POINT ( 'NONE',  ( -24.32775969560190177, -17.60956452435454622, 66.14368435521323875 ) ) ;
#46656 = CARTESIAN_POINT ( 'NONE',  ( -24.05420634179087358, -17.20676946999824608, 69.69867738674849988 ) ) ;
#46657 = EDGE_CURVE ( 'NONE', #23568, #37066, #5472, .T. ) ;
#46658 = ORIENTED_EDGE ( 'NONE', *, *, #10435, .T. ) ;
#46659 = CARTESIAN_POINT ( 'NONE',  ( -17.92409385541305511, -14.80920654474410547, 48.99999999999997868 ) ) ;
#46660 = ORIENTED_EDGE ( 'NONE', *, *, #47184, .F. ) ;
#46661 = CARTESIAN_POINT ( 'NONE',  ( -10.35650339757981442, -17.16777133705972602, 57.80105215977741295 ) ) ;
#46662 = DIRECTION ( 'NONE',  ( 0.09332174201254196666, 0.9956360040033428449, 0.000000000000000000 ) ) ;
#46663 = ORIENTED_EDGE ( 'NONE', *, *, #22545, .T. ) ;
#46664 = CARTESIAN_POINT ( 'NONE',  ( -17.79108452803360763, -21.84994637594637723, 58.69081321602850920 ) ) ;
#46665 = CARTESIAN_POINT ( 'NONE',  ( -24.65877048445197417, -13.03101829210932827, 62.98264174300280160 ) ) ;
#46666 = CARTESIAN_POINT ( 'NONE',  ( -24.72409385541305582, -14.80920654474418896, 65.04705882352939739 ) ) ;
#46667 = CARTESIAN_POINT ( 'NONE',  ( -24.72409385541305582, -14.80920654474417830, 64.94117647058821774 ) ) ;
#46668 = ORIENTED_EDGE ( 'NONE', *, *, #29678, .F. ) ;
#46669 = DIRECTION ( 'NONE',  ( -3.071710424422018668E-17, 6.404604876783312462E-16, 1.000000000000000000 ) ) ;
#46670 = CARTESIAN_POINT ( 'NONE',  ( 18.57590614458706924, 1.890747609047893185, 50.53028072113869484 ) ) ;
#46671 = DIRECTION ( 'NONE',  ( -3.071710424422018668E-17, 6.404604876783312462E-16, 1.000000000000000000 ) ) ;
#46672 = LINE ( 'NONE', #5068, #38377 ) ;
#46673 = DIRECTION ( 'NONE',  ( -3.071710424422018668E-17, 6.404604876783312462E-16, 1.000000000000000000 ) ) ;
#46674 = AXIS2_PLACEMENT_3D ( 'NONE', #23957, #39201, #5235 ) ;
#46675 = DIRECTION ( 'NONE',  ( -0.9000732436326449593, -0.4357386327795698122, 2.072980810273451456E-08 ) ) ;
#46676 = ORIENTED_EDGE ( 'NONE', *, *, #32853, .F. ) ;
#46677 = CARTESIAN_POINT ( 'NONE',  ( -21.15336504700141163, -20.73310185707507713, 69.05450185101547333 ) ) ;
#46678 = FACE_OUTER_BOUND ( 'NONE', #37050, .T. ) ;
#46679 = CARTESIAN_POINT ( 'NONE',  ( -12.46122051107220230, -19.81685944811288635, 64.88146935704573082 ) ) ;
#46680 = EDGE_CURVE ( 'NONE', #47436, #15459, #36893, .T. ) ;
#46681 = ORIENTED_EDGE ( 'NONE', *, *, #38911, .T. ) ;
#46682 = LINE ( 'NONE', #27719, #13661 ) ;
#46683 = FACE_BOUND ( 'NONE', #7618, .T. ) ;
#46684 = ORIENTED_EDGE ( 'NONE', *, *, #15150, .F. ) ;
#46685 = ORIENTED_EDGE ( 'NONE', *, *, #37769, .F. ) ;
#46686 = EDGE_LOOP ( 'NONE', ( #45040, #1231 ) ) ;
#46687 = APPLICATION_CONTEXT ( 'automotive_design' ) ;
#46688 = DIRECTION ( 'NONE',  ( 3.071710424422018668E-17, -6.404604876783312462E-16, -1.000000000000000000 ) ) ;
#46689 = CARTESIAN_POINT ( 'NONE',  ( -12.88340866885723912, -8.902872279917016130, 67.57953991358206736 ) ) ;
#46690 =( BOUNDED_SURFACE ( )  B_SPLINE_SURFACE ( 3, 1, ( 
 ( #6934, #14292 ),
 ( #2987, #21953 ),
 ( #3475, #36692 ),
 ( #33490, #40189 ),
 ( #48531, #10631 ),
 ( #6462, #44613 ),
 ( #9910, #44152 ) ),
 .UNSPECIFIED., .T., .F., .F. ) 
 B_SPLINE_SURFACE_WITH_KNOTS ( ( 4, 3, 4 ),
 ( 2, 2 ),
 ( 0.000000000000000000, 0.5000000000000000000, 1.000000000000000000 ),
 ( 0.000000000000000000, 1.000000000000000000 ),
 .UNSPECIFIED. ) 
 GEOMETRIC_REPRESENTATION_ITEM ( )  RATIONAL_B_SPLINE_SURFACE ( (
 ( 1.000000000000000000, 1.000000000000000000),
 ( 0.3333333333333335369, 0.3333333333333330373),
 ( 0.3333333333333335369, 0.3333333333333330373),
 ( 1.000000000000000000, 1.000000000000000000),
 ( 0.3333333333333333703, 0.3333333333333333703),
 ( 0.3333333333333333703, 0.3333333333333333703),
 ( 1.000000000000000000, 1.000000000000000000) ) ) 
 REPRESENTATION_ITEM ( '' )  SURFACE ( )  );
#46691 = DIRECTION ( 'NONE',  ( 1.224646799147353207E-16, 1.000000000000000000, -1.912410701131276611E-32 ) ) ;
#46692 = CARTESIAN_POINT ( 'NONE',  ( -13.79205357149631084, -8.762576837000361607, 57.06148030867162646 ) ) ;
#46693 = CARTESIAN_POINT ( 'NONE',  ( -22.66727051383977809, -10.09628829486277546, 70.31178520457007153 ) ) ;
#46694 = ORIENTED_EDGE ( 'NONE', *, *, #6492, .F. ) ;
#46695 = ORIENTED_EDGE ( 'NONE', *, *, #36550, .T. ) ;
#46696 = CARTESIAN_POINT ( 'NONE',  ( -22.38659385650551670, -9.302874398569244363, 51.68646062012417985 ) ) ;
#46697 = B_SPLINE_CURVE_WITH_KNOTS ( 'NONE', 3,
 ( #42346, #34940, #1208, #16212, #5163, #46285, #12538, #14212, #37860, #37355 ),
 .UNSPECIFIED., .F., .F.,
 ( 4, 2, 2, 2, 4 ),
 ( 0.1272669073658217465, 0.2522669073463153500, 0.3772669073268088979, 0.5022669073073025015, 0.6272669072877961050 ),
 .UNSPECIFIED. ) ;
#46698 = ADVANCED_FACE ( 'NONE', ( #2207 ), #30411, .T. ) ;
#46699 = FACE_OUTER_BOUND ( 'NONE', #48400, .T. ) ;
#46700 = LINE ( 'NONE', #9271, #10289 ) ;
#46701 = FACE_OUTER_BOUND ( 'NONE', #24501, .T. ) ;
#46702 =( BOUNDED_CURVE ( )  B_SPLINE_CURVE ( 3, ( #40631, #48268, #22669, #22929 ),
 .UNSPECIFIED., .F., .F. ) 
 B_SPLINE_CURVE_WITH_KNOTS ( ( 4, 4 ),
 ( 0.000000000000000000, 0.4074455897393636228 ),
 .UNSPECIFIED. ) 
 CURVE ( )  GEOMETRIC_REPRESENTATION_ITEM ( )  RATIONAL_B_SPLINE_CURVE ( ( 1.000000000000000000, 0.4567392136813349657, 0.3561768502900314326, 0.6983129098260894008 ) ) 
 REPRESENTATION_ITEM ( '' )  );
#46703 = CARTESIAN_POINT ( 'NONE',  ( -21.37409385650551741, -9.792211528768504536, 50.49490371617623197 ) ) ;
#46704 = VERTEX_POINT ( 'NONE', #23909 ) ;
#46705 = ADVANCED_FACE ( 'NONE', ( #13272 ), #43627, .T. ) ;
#46706 = LINE ( 'NONE', #24303, #21770 ) ;
#46707 = CYLINDRICAL_SURFACE ( 'NONE', #44974, 5.500000000000000000 ) ;
#46708 = AXIS2_PLACEMENT_3D ( 'NONE', #2025, #17020, #35986 ) ;
#46709 = CARTESIAN_POINT ( 'NONE',  ( -24.48810908846319734, -17.17637088580320537, 73.06831457992643664 ) ) ;
#46710 = ADVANCED_FACE ( 'NONE', ( #16495 ), #5437, .F. ) ;
#46711 = ORIENTED_EDGE ( 'NONE', *, *, #22793, .T. ) ;
#46712 = DIRECTION ( 'NONE',  ( -5.731567514496413899E-31, -1.020425574103664789E-16, -1.000000000000000000 ) ) ;
#46713 =( BOUNDED_CURVE ( )  B_SPLINE_CURVE ( 3, ( #31506, #46541, #5659, #42836 ),
 .UNSPECIFIED., .F., .F. ) 
 B_SPLINE_CURVE_WITH_KNOTS ( ( 4, 4 ),
 ( 0.4074455897393680082, 0.5000000000000000000 ),
 .UNSPECIFIED. ) 
 CURVE ( )  GEOMETRIC_REPRESENTATION_ITEM ( )  RATIONAL_B_SPLINE_CURVE ( ( 0.6983129098260871803, 0.7760317562606960928, 0.8765941196520011802, 1.000000000000004663 ) ) 
 REPRESENTATION_ITEM ( '' )  );
#46714 = CARTESIAN_POINT ( 'NONE',  ( -9.974481508125691676, -14.72588544478808181, 71.37136786695171509 ) ) ;
#46715 = DIRECTION ( 'NONE',  ( 0.9687793358424821033, -0.2479245821708677133, 0.000000000000000000 ) ) ;
#46716 = CARTESIAN_POINT ( 'NONE',  ( -22.08699904183838214, -20.10091237387970153, 66.11910372887342646 ) ) ;
#46717 = ORIENTED_EDGE ( 'NONE', *, *, #9497, .F. ) ;
#46718 = CARTESIAN_POINT ( 'NONE',  ( -16.13432406759100601, -21.74052631579560568, 58.30057715624173653 ) ) ;
#46719 = EDGE_CURVE ( 'NONE', #31278, #36791, #9126, .T. ) ;
#46720 = CARTESIAN_POINT ( 'NONE',  ( -24.04044854132572340, -11.23863070794140384, 54.02312124697527906 ) ) ;
#46721 = DIRECTION ( 'NONE',  ( 0.9687793358424821033, -0.2479245821708679909, 0.000000000000000000 ) ) ;
#46722 = VERTEX_POINT ( 'NONE', #5910 ) ;
#46723 = CYLINDRICAL_SURFACE ( 'NONE', #12587, 0.1499999999999986899 ) ;
#46724 = ADVANCED_FACE ( 'NONE', ( #38670 ), #39640, .T. ) ;
#46725 = VERTEX_POINT ( 'NONE', #20452 ) ;
#46726 = CARTESIAN_POINT ( 'NONE',  ( -22.33376602745314798, -19.86903051493498040, 69.18890041286789483 ) ) ;
#46727 = CARTESIAN_POINT ( 'NONE',  ( -14.59831579263453527, -7.915781757621413561, 60.44183550242978242 ) ) ;
#46728 = ORIENTED_EDGE ( 'NONE', *, *, #11941, .F. ) ;
#46729 = EDGE_CURVE ( 'NONE', #35496, #33105, #26657, .T. ) ;
#46730 = CARTESIAN_POINT ( 'NONE',  ( -16.05981277502693416, -21.73406819447767901, 61.90001277639490951 ) ) ;
#46731 = CARTESIAN_POINT ( 'NONE',  ( -10.76785811675246940, -12.48515291162924434, 57.61385273545094066 ) ) ;
#46732 = CARTESIAN_POINT ( 'NONE',  ( -17.01596658974409593, -7.370308080546169371, 74.07522964315150205 ) ) ;
#46733 = FACE_OUTER_BOUND ( 'NONE', #32347, .T. ) ;
#46734 = ORIENTED_EDGE ( 'NONE', *, *, #22009, .F. ) ;
#46735 = CARTESIAN_POINT ( 'NONE',  ( -13.38462805196022920, -20.58720062598995426, 58.34650077712428384 ) ) ;
#46736 = LINE ( 'NONE', #28007, #20337 ) ;
#46737 = CARTESIAN_POINT ( 'NONE',  ( -23.44028840568416783, -19.20329456582437899, 62.55418086402786315 ) ) ;
#46738 = EDGE_LOOP ( 'NONE', ( #33751, #3438, #43694, #33646 ) ) ;
#46739 = CARTESIAN_POINT ( 'NONE',  ( -17.42409385541299471, -14.80920654474435771, 49.52966884056655772 ) ) ;
#46740 = VECTOR ( 'NONE', #4062, 1000.000000000000000 ) ;
#46741 = DIRECTION ( 'NONE',  ( 2.866981220435666553E-17, -1.000000000000000000, -1.190614954331866791E-16 ) ) ;
#46742 = ORIENTED_EDGE ( 'NONE', *, *, #13490, .T. ) ;
#46743 = ORIENTED_EDGE ( 'NONE', *, *, #40033, .T. ) ;
#46744 = CARTESIAN_POINT ( 'NONE',  ( -14.78519852893282582, -21.29287441001463677, 58.46617891049388760 ) ) ;
#46745 = CARTESIAN_POINT ( 'NONE',  ( -21.91034545428830782, -20.18261758176410936, 58.76442899736473180 ) ) ;
#46746 = CARTESIAN_POINT ( 'NONE',  ( -11.35719102664687874, -18.40077844947705543, 58.09242476654641507 ) ) ;
#46747 = CARTESIAN_POINT ( 'NONE',  ( -17.63034385650551528, -9.794322478646142471, 51.19202720610083901 ) ) ;
#46748 = CARTESIAN_POINT ( 'NONE',  ( -18.79049830835916524, -7.892586073225762000, 70.38540174208183942 ) ) ;
#46749 = B_SPLINE_CURVE_WITH_KNOTS ( 'NONE', 3,
 ( #48455, #33929, #223, #29760, #26070, #15201, #48708, #30259, #45279, #22364 ),
 .UNSPECIFIED., .F., .F.,
 ( 4, 2, 2, 2, 4 ),
 ( 0.1272669073657906602, 0.2522669073462913691, 0.3772669073267920226, 0.5022669073072927315, 0.6272669072877934404 ),
 .UNSPECIFIED. ) ;
#46750 = CARTESIAN_POINT ( 'NONE',  ( -24.72409385541305582, -14.80920654474410902, 57.89999999999999147 ) ) ;
#46751 = CARTESIAN_POINT ( 'NONE',  ( -10.72530867274958410, -17.00760959713300835, 57.97288447305809456 ) ) ;
#46752 = CARTESIAN_POINT ( 'NONE',  ( -23.30016224357493826, -19.38910683590379236, 59.14056577394535452 ) ) ;
#46753 = ORIENTED_EDGE ( 'NONE', *, *, #48466, .T. ) ;
#46754 = VERTEX_POINT ( 'NONE', #34966 ) ;
#46755 = CARTESIAN_POINT ( 'NONE',  ( -10.61641629527463770, -11.78277212779517136, 74.74335553404092991 ) ) ;
#46756 = CARTESIAN_POINT ( 'NONE',  ( 0.000000000000000000, 0.000000000000000000, 0.000000000000000000 ) ) ;
#46757 = DIRECTION ( 'NONE',  ( -0.1922068328301543838, -0.9813544382196449645, 7.804899501296265607E-08 ) ) ;
#46758 = DIRECTION ( 'NONE',  ( 3.413470714839332458E-33, -1.190614954331866791E-16, 1.000000000000000000 ) ) ;
#46759 = FACE_OUTER_BOUND ( 'NONE', #18438, .T. ) ;
#46760 = B_SPLINE_CURVE_WITH_KNOTS ( 'NONE', 3,
 ( #31460, #39084, #465, #27766, #1413, #46497, #16176, #8832, #8105, #35143 ),
 .UNSPECIFIED., .F., .F.,
 ( 4, 2, 2, 2, 4 ),
 ( 0.000000000000000000, 0.2500000000000000000, 0.5000000000000000000, 0.7500000000000000000, 1.000000000000000000 ),
 .UNSPECIFIED. ) ;
#46761 = ORIENTED_EDGE ( 'NONE', *, *, #44217, .F. ) ;
#46762 = EDGE_CURVE ( 'NONE', #37103, #20782, #13521, .T. ) ;
#46763 = CARTESIAN_POINT ( 'NONE',  ( -14.96636237700334604, -21.36369153681597410, 61.93600446056886000 ) ) ;
#46764 = EDGE_CURVE ( 'NONE', #47392, #42844, #18021, .T. ) ;
#46765 = CARTESIAN_POINT ( 'NONE',  ( -15.48424059001683339, -21.53504990492328375, 72.04575460974366763 ) ) ;
#46766 = FACE_OUTER_BOUND ( 'NONE', #17674, .T. ) ;
#46767 = ORIENTED_EDGE ( 'NONE', *, *, #45880, .F. ) ;
#46768 = CARTESIAN_POINT ( 'NONE',  ( -10.13926443761864782, -13.24856975666061665, 74.85630413064295396 ) ) ;
#46769 = VECTOR ( 'NONE', #15228, 1000.000000000000114 ) ;
#46770 = CARTESIAN_POINT ( 'NONE',  ( -4.424093855413056886, -6.859206544744110623, 50.49999999999999289 ) ) ;
#46771 = CIRCLE ( 'NONE', #25529, 5.249999999999998224 ) ;
#46772 = CARTESIAN_POINT ( 'NONE',  ( -10.50893933415051507, -13.43540278197274063, 74.96345540680638919 ) ) ;
#46773 = CARTESIAN_POINT ( 'NONE',  ( -11.06572510127579356, -10.92528991087847068, 57.32247810849851533 ) ) ;
#46774 = CARTESIAN_POINT ( 'NONE',  ( -18.98647833766290915, -7.985345034418963373, 66.91688477291717163 ) ) ;
#46775 = ORIENTED_EDGE ( 'NONE', *, *, #40499, .T. ) ;
#46776 = EDGE_CURVE ( 'NONE', #8086, #48574, #21577, .T. ) ;
#46777 = ORIENTED_EDGE ( 'NONE', *, *, #11919, .F. ) ;
#46778 = CARTESIAN_POINT ( 'NONE',  ( -14.62409385759799108, -9.359200813967568422, 50.49621490985803263 ) ) ;
#46779 = CARTESIAN_POINT ( 'NONE',  ( -10.42496409799848323, -14.69883155267435626, 71.62782692796884021 ) ) ;
#46780 = EDGE_LOOP ( 'NONE', ( #42722, #20190, #4061, #47352, #26025 ) ) ;
#46781 = EDGE_CURVE ( 'NONE', #22937, #3266, #3086, .T. ) ;
#46782 = ADVANCED_FACE ( 'NONE', ( #47521 ), #21427, .F. ) ;
#46783 = EDGE_CURVE ( 'NONE', #48327, #14597, #7814, .T. ) ;
#46784 = DIRECTION ( 'NONE',  ( -9.593247862760507776E-06, -5.650837228699102996E-06, 0.9999999999380188020 ) ) ;
#46785 = CARTESIAN_POINT ( 'NONE',  ( -11.42962470904260464, -10.38539412368214521, 74.62380407152070916 ) ) ;
#46786 = ORIENTED_EDGE ( 'NONE', *, *, #29449, .F. ) ;
#46787 = CARTESIAN_POINT ( 'NONE',  ( -24.43362360091610697, -14.05489060867666851, 73.42271507725003232 ) ) ;
#46788 =( BOUNDED_CURVE ( )  B_SPLINE_CURVE ( 3, ( #46434, #34602, #4825, #16115 ),
 .UNSPECIFIED., .F., .F. ) 
 B_SPLINE_CURVE_WITH_KNOTS ( ( 4, 4 ),
 ( 0.4074455897393641779, 0.5000000000000000000 ),
 .UNSPECIFIED. ) 
 CURVE ( )  GEOMETRIC_REPRESENTATION_ITEM ( )  RATIONAL_B_SPLINE_CURVE ( ( 0.6983129098260966172, 0.7760317562607159658, 0.8765941196520214973, 1.000000000000023315 ) ) 
 REPRESENTATION_ITEM ( '' )  );
#46789 = CARTESIAN_POINT ( 'NONE',  ( -24.46812100523181144, -14.51191712007779699, 66.19764790277996269 ) ) ;
#46790 = CARTESIAN_POINT ( 'NONE',  ( -16.36834346081282732, -22.18410778960565466, 61.94063409281806543 ) ) ;
#46791 = ORIENTED_EDGE ( 'NONE', *, *, #35717, .F. ) ;
#46792 = CARTESIAN_POINT ( 'NONE',  ( -23.83833621072449560, -17.61232891644574394, 62.47360984984814536 ) ) ;
#46793 = CARTESIAN_POINT ( 'NONE',  ( -26.80819156775448420, -19.72453833035618942, 53.49999999999995026 ) ) ;
#46794 = CARTESIAN_POINT ( 'NONE',  ( -20.49499702560526870, -8.021383449398966192, 66.91957586719850326 ) ) ;
#46795 = CARTESIAN_POINT ( 'NONE',  ( -24.76540221579651302, -16.07765826482591365, 66.17829537637275905 ) ) ;
#46796 = EDGE_LOOP ( 'NONE', ( #37427, #38781, #4274, #24169, #45504 ) ) ;
#46797 = EDGE_LOOP ( 'NONE', ( #14023, #4156, #20927, #1890, #43018 ) ) ;
#46798 = CARTESIAN_POINT ( 'NONE',  ( -22.56207008003183745, -19.63703213565221617, 72.92928497383269359 ) ) ;
#46799 = CARTESIAN_POINT ( 'NONE',  ( -10.46944733747312917, -15.96661384539355133, 67.99239968927004441 ) ) ;
#46800 = ORIENTED_EDGE ( 'NONE', *, *, #43522, .F. ) ;
#46801 = PLANE ( 'NONE',  #48340 ) ;
#46802 = CARTESIAN_POINT ( 'NONE',  ( -17.66159385759798894, -7.228003583438117552, 51.38655588711986155 ) ) ;
#46803 = CARTESIAN_POINT ( 'NONE',  ( -10.42807964966673495, -15.04539577713889287, 74.98882032444942070 ) ) ;
#46804 = B_SPLINE_CURVE_WITH_KNOTS ( 'NONE', 3,
 ( #20179, #31511, #27327, #42357, #31262, #35191, #46546, #27808, #16713, #35434 ),
 .UNSPECIFIED., .F., .F.,
 ( 4, 2, 2, 2, 4 ),
 ( 0.000000000000000000, 0.2500000000000000000, 0.5000000000000000000, 0.7500000000000000000, 1.000000000000000000 ),
 .UNSPECIFIED. ) ;
#46805 = CARTESIAN_POINT ( 'NONE',  ( -12.12786991918758339, -13.32596279628197600, 54.07175714974879099 ) ) ;
#46806 = LINE ( 'NONE', #9385, #45174 ) ;
#46807 = CIRCLE ( 'NONE', #35783, 2.000000000000001332 ) ;
#46808 = EDGE_LOOP ( 'NONE', ( #15058, #48621, #38555, #18347 ) ) ;
#46809 = CARTESIAN_POINT ( 'NONE',  ( -22.68532657142340980, -20.08396690885253477, 69.21772085510332317 ) ) ;
#46810 = EDGE_CURVE ( 'NONE', #5613, #32492, #42164, .T. ) ;
#46811 = AXIS2_PLACEMENT_3D ( 'NONE', #6878, #34858, #23555 ) ;
#46812 = CARTESIAN_POINT ( 'NONE',  ( -20.82057359985130773, -8.686965325372206337, 60.06955151264084236 ) ) ;
#46813 = LINE ( 'NONE', #9870, #22475 ) ;
#46814 = DIRECTION ( 'NONE',  ( 1.616182858256114592E-16, 0.003028072113811714535, -0.9999954153791273948 ) ) ;
#46815 = ORIENTED_EDGE ( 'NONE', *, *, #14910, .T. ) ;
#46816 = VERTEX_POINT ( 'NONE', #47751 ) ;
#46817 = ORIENTED_EDGE ( 'NONE', *, *, #16023, .T. ) ;
#46818 = DIRECTION ( 'NONE',  ( 0.4182840851231335866, -0.9083162577718748576, 8.112345261759808545E-09 ) ) ;
#46819 = EDGE_CURVE ( 'NONE', #6686, #5083, #35418, .T. ) ;
#46820 = FACE_OUTER_BOUND ( 'NONE', #4029, .T. ) ;
#46821 = VERTEX_POINT ( 'NONE', #33620 ) ;
#46822 = CARTESIAN_POINT ( 'NONE',  ( -10.43726484089306439, -14.35454122530442511, 67.96873162560321191 ) ) ;
#46823 = CARTESIAN_POINT ( 'NONE',  ( -10.38078067960954520, -14.50222210708341564, 68.15800126083217947 ) ) ;
#46824 = ORIENTED_EDGE ( 'NONE', *, *, #43943, .T. ) ;
#46825 = DIRECTION ( 'NONE',  ( 0.3124635249310679375, 0.8422251632096487972, 0.4393441931380594467 ) ) ;
#46826 = ORIENTED_EDGE ( 'NONE', *, *, #23275, .F. ) ;
#46827 =( BOUNDED_CURVE ( )  B_SPLINE_CURVE ( 3, ( #36020, #9466, #2303, #1574 ),
 .UNSPECIFIED., .F., .F. ) 
 B_SPLINE_CURVE_WITH_KNOTS ( ( 4, 4 ),
 ( 1.570796326794896558, 1.780235837034218394 ),
 .UNSPECIFIED. ) 
 CURVE ( )  GEOMETRIC_REPRESENTATION_ITEM ( )  RATIONAL_B_SPLINE_CURVE ( ( 1.000000000000000000, 0.9963479302455153785, 0.9963479302455153785, 1.000000000000000000 ) ) 
 REPRESENTATION_ITEM ( '' )  );
#46828 = CARTESIAN_POINT ( 'NONE',  ( -15.84612626051299600, -7.989255239880060699, 67.44007225974215203 ) ) ;
#46829 = ORIENTED_EDGE ( 'NONE', *, *, #10035, .T. ) ;
#46830 = CARTESIAN_POINT ( 'NONE',  ( -13.49112199889614594, -21.13648260148447378, 65.08654642282640168 ) ) ;
#46831 = AXIS2_PLACEMENT_3D ( 'NONE', #23502, #19552, #27674 ) ;
#46832 = ORIENTED_EDGE ( 'NONE', *, *, #39494, .F. ) ;
#46833 = FACE_OUTER_BOUND ( 'NONE', #31065, .T. ) ;
#46834 = CARTESIAN_POINT ( 'NONE',  ( -10.70566866894272984, -16.94585410378973123, 57.98760548748136046 ) ) ;
#46835 = CARTESIAN_POINT ( 'NONE',  ( -36.42409385541304800, -8.109206544743658540, 50.50000000000030553 ) ) ;
#46836 = ORIENTED_EDGE ( 'NONE', *, *, #26430, .F. ) ;
#46837 = FACE_OUTER_BOUND ( 'NONE', #1652, .T. ) ;
#46838 = EDGE_CURVE ( 'NONE', #23803, #8529, #16450, .T. ) ;
#46839 = ADVANCED_FACE ( 'NONE', ( #37823 ), #14904, .T. ) ;
#46840 = CARTESIAN_POINT ( 'NONE',  ( -11.30361205576526196, -11.41219277671509147, 64.44882039656690154 ) ) ;
#46841 = CYLINDRICAL_SURFACE ( 'NONE', #23439, 5.249999999999998224 ) ;
#46842 = CARTESIAN_POINT ( 'NONE',  ( -14.57536025382065148, -8.356334209363122767, 60.31996305705101236 ) ) ;
#46843 = CARTESIAN_POINT ( 'NONE',  ( -13.14551704304688684, -16.75068433397604295, 49.52966884056655772 ) ) ;
#46844 = CARTESIAN_POINT ( 'NONE',  ( -19.28939690137687535, -8.062307696266060475, 59.96092997387292201 ) ) ;
#46845 = VERTEX_POINT ( 'NONE', #17697 ) ;
#46847 = PLANE ( 'NONE',  #19177 ) ;
#46846 =( BOUNDED_CURVE ( )  B_SPLINE_CURVE ( 3, ( #18480, #22434, #10626, #41149 ),
 .UNSPECIFIED., .F., .F. ) 
 B_SPLINE_CURVE_WITH_KNOTS ( ( 4, 4 ),
 ( 0.4074455897393672310, 0.5000000000000000000 ),
 .UNSPECIFIED. ) 
 CURVE ( )  GEOMETRIC_REPRESENTATION_ITEM ( )  RATIONAL_B_SPLINE_CURVE ( ( 0.6983129098260973944, 0.7760317562607038644, 0.8765941196520053991, 1.000000000000003109 ) ) 
 REPRESENTATION_ITEM ( '' )  );
#46848 = DIRECTION ( 'NONE',  ( -5.854827030937197869E-31, -1.020425574103664912E-16, -1.000000000000000000 ) ) ;
#46849 = LINE ( 'NONE', #47093, #7838 ) ;
#46850 = ADVANCED_FACE ( 'NONE', ( #7560 ), #20040, .T. ) ;
#46851 = EDGE_CURVE ( 'NONE', #42645, #33357, #13113, .T. ) ;
#46852 = CARTESIAN_POINT ( 'NONE',  ( -15.20895699419056335, -21.92244470331527850, 68.71446411004870924 ) ) ;
#46853 = CARTESIAN_POINT ( 'NONE',  ( -18.11159385759799179, -8.990409506049200417, 49.61344411288074951 ) ) ;
#46854 = CARTESIAN_POINT ( 'NONE',  ( -16.78659385650551883, -9.302874398569244363, 51.68646062012417985 ) ) ;
#46856 = EDGE_CURVE ( 'NONE', #8086, #25610, #40452, .T. ) ;
#46855 = ORIENTED_EDGE ( 'NONE', *, *, #10170, .F. ) ;
#46857 = DIRECTION ( 'NONE',  ( 3.071710424422018668E-17, -6.404604876783312462E-16, -1.000000000000000000 ) ) ;
#46858 = CARTESIAN_POINT ( 'NONE',  ( -24.45381059137804058, -15.38184444469599299, 72.88814935371863157 ) ) ;
#46859 = EDGE_LOOP ( 'NONE', ( #28803, #5331 ) ) ;
#46860 = CARTESIAN_POINT ( 'NONE',  ( -11.33385179977767265, -19.10019906511433518, 68.26043675633501095 ) ) ;
#46861 = CARTESIAN_POINT ( 'NONE',  ( -14.44809135640554487, -8.473323881223761234, 67.55975083863336295 ) ) ;
#46862 = CARTESIAN_POINT ( 'NONE',  ( -12.73947787985187574, -9.016276410220392279, 71.10571287364943771 ) ) ;
#46863 = DIRECTION ( 'NONE',  ( 0.000000000000000000, 1.000000000000000000, -0.000000000000000000 ) ) ;
#46864 = DIRECTION ( 'NONE',  ( -1.000000000000000000, 0.000000000000000000, 0.000000000000000000 ) ) ;
#46865 = VERTEX_POINT ( 'NONE', #19602 ) ;
#46866 = CYLINDRICAL_SURFACE ( 'NONE', #31796, 0.1500000000000008826 ) ;
#46867 = CARTESIAN_POINT ( 'NONE',  ( -12.10131192688100299, -10.18592936015514816, 64.31442259820508411 ) ) ;
#46868 = CARTESIAN_POINT ( 'NONE',  ( -20.69509252757554307, -8.115601716887088202, 63.49616818922779515 ) ) ;
#46869 = EDGE_CURVE ( 'NONE', #44032, #10945, #1516, .T. ) ;
#46870 = EDGE_LOOP ( 'NONE', ( #33369, #39135 ) ) ;
#46871 = CARTESIAN_POINT ( 'NONE',  ( -13.33011785382929304, -9.069340661520646663, 63.92418669539090814 ) ) ;
#46872 = CARTESIAN_POINT ( 'NONE',  ( -13.30711473254145716, -9.147892019113847084, 63.90946529584681457 ) ) ;
#46873 = FACE_OUTER_BOUND ( 'NONE', #32673, .T. ) ;
#46874 = CARTESIAN_POINT ( 'NONE',  ( -16.81784385759798894, -6.860780111191492558, 51.02154966934378422 ) ) ;
#46875 = CARTESIAN_POINT ( 'NONE',  ( -45.92409385541306222, -14.20017296387473316, 71.05663168951063824 ) ) ;
#46876 = ORIENTED_EDGE ( 'NONE', *, *, #31552, .T. ) ;
#46877 = ORIENTED_EDGE ( 'NONE', *, *, #37651, .T. ) ;
#46878 = VECTOR ( 'NONE', #1263, 1000.000000000000114 ) ;
#46879 = CARTESIAN_POINT ( 'NONE',  ( -18.69909385541304303, -8.105421454601382081, 49.25000573077640098 ) ) ;
#46880 = B_SPLINE_CURVE_WITH_KNOTS ( 'NONE', 1,
 ( #35255, #31089 ),
 .UNSPECIFIED., .F., .F.,
 ( 2, 2 ),
 ( 0.000000000000000000, 1.000000000000000000 ),
 .UNSPECIFIED. ) ;
#46881 = CARTESIAN_POINT ( 'NONE',  ( -15.06092214208368141, -7.686424710462701704, 53.76173960638114124 ) ) ;
#46882 = DIRECTION ( 'NONE',  ( 3.071710424422018668E-17, -6.404604876783312462E-16, -1.000000000000000000 ) ) ;
#46883 = CARTESIAN_POINT ( 'NONE',  ( -24.45201636468676654, -14.25170757634699825, 69.95275273439749242 ) ) ;
#46884 = LINE ( 'NONE', #9943, #15151 ) ;
#46885 = ORIENTED_EDGE ( 'NONE', *, *, #47728, .T. ) ;
#46886 = CYLINDRICAL_SURFACE ( 'NONE', #6371, 0.1499999999999971634 ) ;
#46887 = CARTESIAN_POINT ( 'NONE',  ( -24.25527139147240518, -17.78202422108329017, 62.67349770570701395 ) ) ;
#46888 = EDGE_CURVE ( 'NONE', #48469, #24724, #16123, .T. ) ;
#46889 = EDGE_LOOP ( 'NONE', ( #30061, #1782 ) ) ;
#46890 = CARTESIAN_POINT ( 'NONE',  ( -21.89826351590202336, -8.852228842849337198, 66.84645279485334868 ) ) ;
#46891 = CARTESIAN_POINT ( 'NONE',  ( -16.32745258320347759, -21.77369344365219561, 61.77040269689842944 ) ) ;
#46893 = VERTEX_POINT ( 'NONE', #1358 ) ;
#46892 =( BOUNDED_CURVE ( )  B_SPLINE_CURVE ( 3, ( #19336, #23288, #5063, #1598 ),
 .UNSPECIFIED., .F., .F. ) 
 B_SPLINE_CURVE_WITH_KNOTS ( ( 4, 4 ),
 ( 0.000000000000000000, 0.4074455897269660953 ),
 .UNSPECIFIED. ) 
 CURVE ( )  GEOMETRIC_REPRESENTATION_ITEM ( )  RATIONAL_B_SPLINE_CURVE ( ( 1.000000000000000000, 0.4567392136978657424, 0.3561768502961514260, 0.6983129097948570507 ) ) 
 REPRESENTATION_ITEM ( '' )  );
#46894 = CARTESIAN_POINT ( 'NONE',  ( -10.53536195276627829, -13.30851587854854579, 74.69289754060230280 ) ) ;
#46895 = CARTESIAN_POINT ( 'NONE',  ( -22.92319839529956838, -10.39759132684999265, 63.22185995336808162 ) ) ;
#46896 = ORIENTED_EDGE ( 'NONE', *, *, #22009, .T. ) ;
#46897 = CARTESIAN_POINT ( 'NONE',  ( -17.77761167241057549, -22.25089262147902147, 58.44907471483963946 ) ) ;
#46898 = EDGE_CURVE ( 'NONE', #3283, #26502, #10426, .T. ) ;
#46899 = CARTESIAN_POINT ( 'NONE',  ( -42.92262326717776943, -14.90920654474412643, 59.01176470588234224 ) ) ;
#46900 = CARTESIAN_POINT ( 'NONE',  ( -16.76036020169118146, -21.82793338258416327, 68.69560668698967731 ) ) ;
#46901 = ORIENTED_EDGE ( 'NONE', *, *, #31495, .F. ) ;
#46902 = CARTESIAN_POINT ( 'NONE',  ( -10.33481637538221243, -12.51883299443452202, 60.84207650303104487 ) ) ;
#46903 = DIRECTION ( 'NONE',  ( 6.446466753401607987E-06, -1.047023822510701943E-05, -0.9999999999244085780 ) ) ;
#46904 = CARTESIAN_POINT ( 'NONE',  ( -21.55883939963115026, -8.611815437115641458, 73.78624134823098757 ) ) ;
#46905 = AXIS2_PLACEMENT_3D ( 'NONE', #27920, #25381, #44577 ) ;
#46906 = AXIS2_PLACEMENT_3D ( 'NONE', #30545, #15237, #27314 ) ;
#46907 = CARTESIAN_POINT ( 'NONE',  ( -12.04584144946014312, -10.25080825636289816, 67.50456653540463492 ) ) ;
#46908 = EDGE_CURVE ( 'NONE', #48314, #24620, #19213, .T. ) ;
#46909 = CYLINDRICAL_SURFACE ( 'NONE', #14803, 4.686499999999997002 ) ;
#46910 = FACE_OUTER_BOUND ( 'NONE', #35028, .T. ) ;
#46911 = EDGE_CURVE ( 'NONE', #3548, #1447, #30458, .T. ) ;
#46912 = DIRECTION ( 'NONE',  ( 2.866981220435666553E-17, -1.000000000000000000, -1.190614954331866791E-16 ) ) ;
#46913 = ORIENTED_EDGE ( 'NONE', *, *, #6379, .F. ) ;
#46914 = CARTESIAN_POINT ( 'NONE',  ( -13.84778738435022305, -8.273584231232366193, 74.32141925404624772 ) ) ;
#46915 = EDGE_CURVE ( 'NONE', #14217, #27480, #23796, .T. ) ;
#46916 = CARTESIAN_POINT ( 'NONE',  ( -15.15660932275500272, -21.48492473237050859, 65.39124617759186719 ) ) ;
#46917 = CARTESIAN_POINT ( 'NONE',  ( -19.20714268997449281, -19.15619313305651161, 49.52966884056656482 ) ) ;
#46918 = VERTEX_POINT ( 'NONE', #34123 ) ;
#46919 = DIRECTION ( 'NONE',  ( -3.071710424422018668E-17, 6.404604876783312462E-16, 1.000000000000000000 ) ) ;
#46920 = ORIENTED_EDGE ( 'NONE', *, *, #11792, .F. ) ;
#46921 = ORIENTED_EDGE ( 'NONE', *, *, #23970, .F. ) ;
#46922 = ORIENTED_EDGE ( 'NONE', *, *, #25100, .F. ) ;
#46923 = CARTESIAN_POINT ( 'NONE',  ( -15.68503317936312236, -7.977064329016499755, 70.60989839961001735 ) ) ;
#46924 = LINE ( 'NONE', #25004, #31087 ) ;
#46925 = CARTESIAN_POINT ( 'NONE',  ( -21.76243611580424897, -17.76577320756515022, 49.52966884056655772 ) ) ;
#46926 = CARTESIAN_POINT ( 'NONE',  ( -15.18659385759799108, -7.222650657624104298, 49.61879703869476543 ) ) ;
#46927 = CARTESIAN_POINT ( 'NONE',  ( -13.46747565276156422, -9.034678650756244878, 60.73950277887485072 ) ) ;
#46928 = ORIENTED_EDGE ( 'NONE', *, *, #36586, .F. ) ;
#46929 = ORIENTED_EDGE ( 'NONE', *, *, #19794, .T. ) ;
#46930 = CARTESIAN_POINT ( 'NONE',  ( -21.82409385650551670, -6.426201560718813433, 50.50509628382439331 ) ) ;
#46931 = PLANE ( 'NONE',  #36964 ) ;
#46932 = CARTESIAN_POINT ( 'NONE',  ( -20.94265863490610258, -21.37680627582274795, 62.30126734817043399 ) ) ;
#46933 = CARTESIAN_POINT ( 'NONE',  ( -23.23812175398343172, -18.70765974062167203, 66.10924015431194789 ) ) ;
#46934 = CARTESIAN_POINT ( 'NONE',  ( -21.26159385650551314, -9.295667164867525756, 49.30633214617472504 ) ) ;
#46935 = VECTOR ( 'NONE', #21280, 1000.000000000000000 ) ;
#46936 = EDGE_LOOP ( 'NONE', ( #41826, #7262, #12105, #3211, #9056 ) ) ;
#46937 = FACE_OUTER_BOUND ( 'NONE', #1237, .T. ) ;
#46938 = DIRECTION ( 'NONE',  ( -3.071710424422018668E-17, 6.404604876783312462E-16, 1.000000000000000000 ) ) ;
#46939 = LINE ( 'NONE', #6786, #14175 ) ;
#46940 = VECTOR ( 'NONE', #10285, 1000.000000000000000 ) ;
#46941 = EDGE_CURVE ( 'NONE', #8650, #15655, #30704, .T. ) ;
#46942 = ORIENTED_EDGE ( 'NONE', *, *, #7275, .T. ) ;
#46943 = FACE_OUTER_BOUND ( 'NONE', #41270, .T. ) ;
#46944 = CARTESIAN_POINT ( 'NONE',  ( -11.04141120970326462, -11.93494789359697883, 74.55840195308121565 ) ) ;
#46945 = CARTESIAN_POINT ( 'NONE',  ( -24.47401588851211329, -14.84236380343934592, 59.24300237059242136 ) ) ;
#46946 = VERTEX_POINT ( 'NONE', #896 ) ;
#46947 = CARTESIAN_POINT ( 'NONE',  ( -45.92409385541306222, -14.20920654474410760, 70.50000000000000000 ) ) ;
#46948 = CARTESIAN_POINT ( 'NONE',  ( -22.88419684932020459, -10.42887832691348926, 63.37185995611467604 ) ) ;
#46949 = CARTESIAN_POINT ( 'NONE',  ( -18.11396434131172128, -21.77512919714542150, 65.34532159443909904 ) ) ;
#46950 = ORIENTED_EDGE ( 'NONE', *, *, #18691, .F. ) ;
#46951 = FACE_OUTER_BOUND ( 'NONE', #25873, .T. ) ;
#46952 = VERTEX_POINT ( 'NONE', #34360 ) ;
#46953 = CARTESIAN_POINT ( 'NONE',  ( -13.54823083431842612, -20.69819501703281617, 61.66646323538943619 ) ) ;
#46954 = CARTESIAN_POINT ( 'NONE',  ( -16.32142643024854678, -21.72225621288954400, 61.77184823017776694 ) ) ;
#46955 = VERTEX_POINT ( 'NONE', #15895 ) ;
#46956 = CARTESIAN_POINT ( 'NONE',  ( -24.17271927670314113, -12.95015993349377048, 66.30246741691458112 ) ) ;
#46957 = CARTESIAN_POINT ( 'NONE',  ( -21.91034708787274710, -20.18261625685872218, 59.06442899735736773 ) ) ;
#46958 = CARTESIAN_POINT ( 'NONE',  ( -13.30028440927262068, -8.603736347584243660, 60.62605674953037749 ) ) ;
#46959 = EDGE_CURVE ( 'NONE', #37312, #48665, #16845, .T. ) ;
#46960 = DIRECTION ( 'NONE',  ( 0.9687793358424821033, -0.2479245821708680464, 0.000000000000000000 ) ) ;
#46961 = VERTEX_POINT ( 'NONE', #23551 ) ;
#46962 = CARTESIAN_POINT ( 'NONE',  ( -23.94599579101543796, -17.50730996363388314, 59.15945600998260545 ) ) ;
#46963 = EDGE_CURVE ( 'NONE', #44379, #10553, #2204, .T. ) ;
#46964 =( BOUNDED_CURVE ( )  B_SPLINE_CURVE ( 3, ( #40654, #44376, #25639, #17995 ),
 .UNSPECIFIED., .F., .F. ) 
 B_SPLINE_CURVE_WITH_KNOTS ( ( 4, 4 ),
 ( 0.5000000000000000000, 0.9074455897393697290 ),
 .UNSPECIFIED. ) 
 CURVE ( )  GEOMETRIC_REPRESENTATION_ITEM ( )  RATIONAL_B_SPLINE_CURVE ( ( 1.000000000000002442, 0.4567392136813364645, 0.3561768502900302114, 0.6983129098260862921 ) ) 
 REPRESENTATION_ITEM ( '' )  );
#46965 = CARTESIAN_POINT ( 'NONE',  ( -11.35824946695446691, -11.21643166988602047, 60.82885780703593070 ) ) ;
#46966 = ORIENTED_EDGE ( 'NONE', *, *, #44929, .T. ) ;
#46967 = CARTESIAN_POINT ( 'NONE',  ( -11.22202139642810081, -18.93699991513116743, 64.92423932127240960 ) ) ;
#46968 = AXIS2_PLACEMENT_3D ( 'NONE', #31667, #8532, #15657 ) ;
#46969 = EDGE_CURVE ( 'NONE', #38652, #36016, #31660, .T. ) ;
#46970 = CARTESIAN_POINT ( 'NONE',  ( -11.10386593012501244, -18.75361831986885974, 61.32064883311096537 ) ) ;
#46971 = ORIENTED_EDGE ( 'NONE', *, *, #752, .F. ) ;
#46972 = EDGE_LOOP ( 'NONE', ( #120, #29277, #5652, #9151, #44335 ) ) ;
#46973 = CARTESIAN_POINT ( 'NONE',  ( -14.74690617566109019, -21.27702427001963414, 58.46617884968173229 ) ) ;
#46974 = CARTESIAN_POINT ( 'NONE',  ( -21.42336380182764088, -21.09487415076890215, 69.23945570945444672 ) ) ;
#46975 = CARTESIAN_POINT ( 'NONE',  ( 18.57590614458706924, 1.890747609047612077, 50.53028072113853142 ) ) ;
#46976 = AXIS2_PLACEMENT_3D ( 'NONE', #20241, #45875, #1525 ) ;
#46977 = CARTESIAN_POINT ( 'NONE',  ( -19.59909385650551883, -8.114302828567740988, 52.18300498402516041 ) ) ;
#46978 = CARTESIAN_POINT ( 'NONE',  ( -12.44869005970189058, -9.885249076858732664, 57.08935532200567309 ) ) ;
#46979 = EDGE_CURVE ( 'NONE', #37877, #41056, #3344, .T. ) ;
#46980 =( BOUNDED_CURVE ( )  B_SPLINE_CURVE ( 3, ( #44911, #22483, #37478, #3771 ),
 .UNSPECIFIED., .F., .F. ) 
 B_SPLINE_CURVE_WITH_KNOTS ( ( 4, 4 ),
 ( 0.000000000000000000, 0.4074455897393643444 ),
 .UNSPECIFIED. ) 
 CURVE ( )  GEOMETRIC_REPRESENTATION_ITEM ( )  RATIONAL_B_SPLINE_CURVE ( ( 1.000000000000000000, 0.4567392136813230308, 0.3561768502900269917, 0.6983129098261118273 ) ) 
 REPRESENTATION_ITEM ( '' )  );
#46981 = CARTESIAN_POINT ( 'NONE',  ( -13.11716721000957264, -9.290864365938665159, 67.67942741430334763 ) ) ;
#46982 =( BOUNDED_CURVE ( )  B_SPLINE_CURVE ( 3, ( #42288, #8550, #7840, #42041 ),
 .UNSPECIFIED., .F., .F. ) 
 B_SPLINE_CURVE_WITH_KNOTS ( ( 4, 4 ),
 ( 0.4074455897393652326, 0.5000000000000000000 ),
 .UNSPECIFIED. ) 
 CURVE ( )  GEOMETRIC_REPRESENTATION_ITEM ( )  RATIONAL_B_SPLINE_CURVE ( ( 0.6983129098260798528, 0.7760317562606897646, 0.8765941196519972944, 1.000000000000004663 ) ) 
 REPRESENTATION_ITEM ( '' )  );
#46983 = EDGE_CURVE ( 'NONE', #40794, #11434, #10227, .T. ) ;
#46984 = DIRECTION ( 'NONE',  ( 1.224646799147353207E-16, 1.000000000000000000, -1.912410701131276611E-32 ) ) ;
#46985 = VERTEX_POINT ( 'NONE', #9975 ) ;
#46986 = EDGE_LOOP ( 'NONE', ( #23791, #27939, #10940, #41457, #29023 ) ) ;
#46987 = LINE ( 'NONE', #12286, #8485 ) ;
#46988 = DIRECTION ( 'NONE',  ( 1.000000000000000000, 0.000000000000000000, 0.000000000000000000 ) ) ;
#46989 = CARTESIAN_POINT ( 'NONE',  ( -23.63039969342750979, -11.57141254907242534, 66.72214533111647938 ) ) ;
#46990 = LINE ( 'NONE', #6110, #40963 ) ;
#46991 = CARTESIAN_POINT ( 'NONE',  ( -22.38860293988961558, -19.74596265805258710, 72.71570726583541955 ) ) ;
#46992 = CARTESIAN_POINT ( 'NONE',  ( -20.81921488491704864, -21.44071703825394692, 58.75979854551385984 ) ) ;
#46993 =( BOUNDED_CURVE ( )  B_SPLINE_CURVE ( 3, ( #17448, #28779, #24614, #13968 ),
 .UNSPECIFIED., .F., .F. ) 
 B_SPLINE_CURVE_WITH_KNOTS ( ( 4, 4 ),
 ( 0.000000000000000000, 0.4074455897393687298 ),
 .UNSPECIFIED. ) 
 CURVE ( )  GEOMETRIC_REPRESENTATION_ITEM ( )  RATIONAL_B_SPLINE_CURVE ( ( 1.000000000000000000, 0.4567392136813349657, 0.3561768502900314326, 0.6983129098260894008 ) ) 
 REPRESENTATION_ITEM ( '' )  );
#46994 = EDGE_LOOP ( 'NONE', ( #5139, #3456, #28747, #45274 ) ) ;
#46995 = CARTESIAN_POINT ( 'NONE',  ( -12.27604185553471616, -19.62628656662749549, 58.21210303282668264 ) ) ;
#46996 = CARTESIAN_POINT ( 'NONE',  ( -10.21566995694600166, -12.92691906471870311, 67.91549220782184193 ) ) ;
#46997 = CARTESIAN_POINT ( 'NONE',  ( -11.78595478178340805, -10.57665929355158241, 74.43885099124366889 ) ) ;
#46998 = CARTESIAN_POINT ( 'NONE',  ( -24.48810873059073856, -17.17637193698283582, 73.06831349224263761 ) ) ;
#46999 = ADVANCED_FACE ( 'NONE', ( #35343 ), #39764, .T. ) ;
#47000 = EDGE_LOOP ( 'NONE', ( #19464, #36118, #32009, #27007, #7489 ) ) ;
#47001 = CARTESIAN_POINT ( 'NONE',  ( -10.14076703847185001, -13.24135396021726763, 74.81784294846195849 ) ) ;
#47002 = VECTOR ( 'NONE', #4664, 1000.000000000000000 ) ;
#47003 = CARTESIAN_POINT ( 'NONE',  ( -13.18474066807476675, -20.93551553819402855, 58.23145462665691241 ) ) ;
#47004 = DIRECTION ( 'NONE',  ( -2.866981220435666553E-17, 1.000000000000000000, 1.190614954331866791E-16 ) ) ;
#47005 = CARTESIAN_POINT ( 'NONE',  ( -18.65633144910794883, -7.917218216242548401, 74.06894365739631780 ) ) ;
#47006 = DIRECTION ( 'NONE',  ( -0.9687793358424817702, 0.2479245821708684905, 0.000000000000000000 ) ) ;
#47007 = CARTESIAN_POINT ( 'NONE',  ( -14.79922817013080483, -7.836842635312091687, 57.03495431467663224 ) ) ;
#47008 = ORIENTED_EDGE ( 'NONE', *, *, #43310, .T. ) ;
#47009 = EDGE_CURVE ( 'NONE', #23317, #6093, #37959, .T. ) ;
#47010 = CARTESIAN_POINT ( 'NONE',  ( -10.48584376121421791, -13.88064436164177984, 57.74825077270041618 ) ) ;
#47011 = AXIS2_PLACEMENT_3D ( 'NONE', #30527, #22896, #34682 ) ;
#47012 = VERTEX_POINT ( 'NONE', #46679 ) ;
#47013 = CARTESIAN_POINT ( 'NONE',  ( -10.01355597153913024, -14.04293878122132178, 61.11159607317906506 ) ) ;
#47014 = B_SPLINE_CURVE_WITH_KNOTS ( 'NONE', 3,
 ( #13584, #24214, #12873, #17532, #28630, #28862, #24466, #31840, #32557, #39471 ),
 .UNSPECIFIED., .F., .F.,
 ( 4, 2, 2, 2, 4 ),
 ( 0.000000000000000000, 0.2500000000000000000, 0.5000000000000000000, 0.7500000000000000000, 1.000000000000000000 ),
 .UNSPECIFIED. ) ;
#47015 = CARTESIAN_POINT ( 'NONE',  ( -12.50766595982653584, -19.86205097402751463, 65.01674886870775083 ) ) ;
#47016 = ORIENTED_EDGE ( 'NONE', *, *, #3307, .T. ) ;
#47017 = CARTESIAN_POINT ( 'NONE',  ( -10.29584670662963752, -12.64300724171409662, 64.44648870780133620 ) ) ;
#47018 = CARTESIAN_POINT ( 'NONE',  ( -14.23034385650551492, -9.794322478646142471, 51.19202720610083190 ) ) ;
#47019 = ORIENTED_EDGE ( 'NONE', *, *, #38149, .F. ) ;
#47020 = CARTESIAN_POINT ( 'NONE',  ( -15.19548991633585011, -21.91815178685365595, 68.76088227238139439 ) ) ;
#47021 = CARTESIAN_POINT ( 'NONE',  ( -24.46479343890040425, -14.44719913075708995, 66.48292729247951627 ) ) ;
#47022 = CARTESIAN_POINT ( 'NONE',  ( -14.73525069530193399, -21.75714069359356984, 61.89246344873641448 ) ) ;
#47023 = ORIENTED_EDGE ( 'NONE', *, *, #42062, .T. ) ;
#47024 = CARTESIAN_POINT ( 'NONE',  ( -16.12205861630594939, -7.931364996939863410, 60.39131567725520711 ) ) ;
#47025 = CARTESIAN_POINT ( 'NONE',  ( -45.92409385541305511, -15.80920654474410725, 70.50000000000000000 ) ) ;
#47026 = B_SPLINE_CURVE_WITH_KNOTS ( 'NONE', 1,
 ( #16852, #40478 ),
 .UNSPECIFIED., .F., .F.,
 ( 2, 2 ),
 ( 0.000000000000000000, 1.000000000000000000 ),
 .UNSPECIFIED. ) ;
#47027 = ADVANCED_FACE ( 'NONE', ( #17348 ), #43232, .T. ) ;
#47028 = CARTESIAN_POINT ( 'NONE',  ( -17.42409385541299471, -14.80920654474435771, 49.52966884056655772 ) ) ;
#47029 = CARTESIAN_POINT ( 'NONE',  ( -42.07024770156689897, -15.80920654474410725, 65.83076923076922071 ) ) ;
#47030 = ORIENTED_EDGE ( 'NONE', *, *, #23952, .F. ) ;
#47031 = VERTEX_POINT ( 'NONE', #16623 ) ;
#47032 = EDGE_CURVE ( 'NONE', #6412, #9098, #43814, .T. ) ;
#47033 = DIRECTION ( 'NONE',  ( 0.7248509490090242480, -0.6889057277456162032, 1.880377065355303572E-09 ) ) ;
#47034 = CARTESIAN_POINT ( 'NONE',  ( -24.22092292145011072, -12.93687797069017975, 66.60246741374322710 ) ) ;
#47035 = ORIENTED_EDGE ( 'NONE', *, *, #33718, .F. ) ;
#47037 = CARTESIAN_POINT ( 'NONE',  ( -10.00132051839154457, -15.44646819276786154, 57.82438731113803243 ) ) ;
#47036 = AXIS2_PLACEMENT_3D ( 'NONE', #42362, #25282, #17861 ) ;
#47038 = CARTESIAN_POINT ( 'NONE',  ( -23.16117746674104438, -18.90708040007733359, 62.63934749780565880 ) ) ;
#47039 = EDGE_CURVE ( 'NONE', #2068, #25341, #28458, .T. ) ;
#47040 = CARTESIAN_POINT ( 'NONE',  ( -17.38034385759798894, -9.360768649639302552, 51.01397948905922419 ) ) ;
#47041 = CARTESIAN_POINT ( 'NONE',  ( -13.43921731646364925, -8.993429882417945720, 60.43950277494440115 ) ) ;
#47042 = CIRCLE ( 'NONE', #16375, 4.686499999999998778 ) ;
#47043 = CARTESIAN_POINT ( 'NONE',  ( -17.42409385541299471, -14.80920654474435771, 49.52966884056655772 ) ) ;
#47044 = FACE_OUTER_BOUND ( 'NONE', #19407, .T. ) ;
#47045 = AXIS2_PLACEMENT_3D ( 'NONE', #22015, #7255, #37012 ) ;
#47046 = AXIS2_PLACEMENT_3D ( 'NONE', #36296, #43711, #9499 ) ;
#47047 = VERTEX_POINT ( 'NONE', #12926 ) ;
#47048 = CARTESIAN_POINT ( 'NONE',  ( -22.68646401470678953, -20.08284273627726435, 69.35913316877790180 ) ) ;
#47049 = DIRECTION ( 'NONE',  ( 1.000000000000000000, 1.669677910507523057E-21, 6.493791346278465266E-22 ) ) ;
#47050 = B_SPLINE_CURVE_WITH_KNOTS ( 'NONE', 3,
 ( #567, #16048, #19036, #11400, #27155, #34782, #330, #11900, #26424, #42177 ),
 .UNSPECIFIED., .F., .F.,
 ( 4, 2, 2, 2, 4 ),
 ( 0.1272669073658120598, 0.2522669073463025269, 0.3772669073267930218, 0.5022669073072834056, 0.6272669072877739005 ),
 .UNSPECIFIED. ) ;
#47051 = CARTESIAN_POINT ( 'NONE',  ( -24.47371109942907808, -14.90716652360855754, 59.25772288469824645 ) ) ;
#47052 = CARTESIAN_POINT ( 'NONE',  ( -13.45042189503786645, -20.57396435267970247, 61.70573509705739923 ) ) ;
#47053 = EDGE_CURVE ( 'NONE', #20228, #19518, #38581, .T. ) ;
#47054 = B_SPLINE_CURVE_WITH_KNOTS ( 'NONE', 3,
 ( #5732, #31820, #35504, #13325, #20739, #11966, #23050, #11712, #47085, #43402 ),
 .UNSPECIFIED., .F., .F.,
 ( 4, 2, 2, 2, 4 ),
 ( 0.6272669072877935514, 0.7522669073072928425, 0.8772669073267920226, 1.002266907346291314, 1.127266907365790605 ),
 .UNSPECIFIED. ) ;
#47056 = VERTEX_POINT ( 'NONE', #20584 ) ;
#47055 = ADVANCED_FACE ( 'NONE', ( #27953 ), #42981, .T. ) ;
#47057 = ORIENTED_EDGE ( 'NONE', *, *, #35349, .F. ) ;
#47058 = ORIENTED_EDGE ( 'NONE', *, *, #30697, .T. ) ;
#47059 = EDGE_CURVE ( 'NONE', #166, #12496, #18147, .T. ) ;
#47060 = EDGE_CURVE ( 'NONE', #7630, #37913, #8602, .T. ) ;
#47061 = CARTESIAN_POINT ( 'NONE',  ( -24.86960059988683014, -14.52975442119237748, 62.82641240410487171 ) ) ;
#47062 = CARTESIAN_POINT ( 'NONE',  ( -12.50766578132126838, -19.86205079821699115, 65.16674886870754335 ) ) ;
#47063 = CARTESIAN_POINT ( 'NONE',  ( -21.69127741654737918, -9.260229650215405783, 63.38256923939299270 ) ) ;
#47064 = ORIENTED_EDGE ( 'NONE', *, *, #2607, .F. ) ;
#47065 = CARTESIAN_POINT ( 'NONE',  ( -21.70267066777908838, -12.86772875551264050, 49.52966884056655772 ) ) ;
#47066 = DIRECTION ( 'NONE',  ( -1.000000000000000000, -2.866981220435666553E-17, 0.000000000000000000 ) ) ;
#47067 = ORIENTED_EDGE ( 'NONE', *, *, #46030, .F. ) ;
#47068 = CARTESIAN_POINT ( 'NONE',  ( -11.49287318421094817, -18.63485491799402993, 57.96281551145487043 ) ) ;
#47069 = AXIS2_PLACEMENT_3D ( 'NONE', #42625, #9123, #8885 ) ;
#47070 =( BOUNDED_SURFACE ( )  B_SPLINE_SURFACE ( 3, 1, ( 
 ( #42928, #9200 ),
 ( #39227, #36705 ),
 ( #18497, #7447 ),
 ( #43910, #10163 ),
 ( #48066, #21963 ),
 ( #3249, #22454 ),
 ( #40916, #14303 ) ),
 .UNSPECIFIED., .T., .F., .F. ) 
 B_SPLINE_SURFACE_WITH_KNOTS ( ( 4, 3, 4 ),
 ( 2, 2 ),
 ( 0.000000000000000000, 0.5000000000000000000, 1.000000000000000000 ),
 ( 0.000000000000000000, 1.000000000000000000 ),
 .UNSPECIFIED. ) 
 GEOMETRIC_REPRESENTATION_ITEM ( )  RATIONAL_B_SPLINE_SURFACE ( (
 ( 1.000000000000000000, 1.000000000000000000),
 ( 0.3333333333333335369, 0.3333333333333330373),
 ( 0.3333333333333335369, 0.3333333333333330373),
 ( 1.000000000000000000, 1.000000000000000000),
 ( 0.3333333333333333703, 0.3333333333333333703),
 ( 0.3333333333333333703, 0.3333333333333333703),
 ( 1.000000000000000000, 1.000000000000000000) ) ) 
 REPRESENTATION_ITEM ( '' )  SURFACE ( )  );
#47071 = CARTESIAN_POINT ( 'NONE',  ( -12.93830821282824317, -9.435326670572035113, 71.13459971530836867 ) ) ;
#47072 = VERTEX_POINT ( 'NONE', #14115 ) ;
#47073 = CARTESIAN_POINT ( 'NONE',  ( -15.81170465868504316, -7.997374279965050903, 67.42541861783800528 ) ) ;
#47074 = ORIENTED_EDGE ( 'NONE', *, *, #16284, .F. ) ;
#47075 = CARTESIAN_POINT ( 'NONE',  ( -13.54527334699669261, -21.17000357857808979, 65.12482326698327029 ) ) ;
#47076 = AXIS2_PLACEMENT_3D ( 'NONE', #17587, #17819, #47164 ) ;
#47077 = AXIS2_PLACEMENT_3D ( 'NONE', #26687, #12382, #45662 ) ;
#47078 = VERTEX_POINT ( 'NONE', #6765 ) ;
#47079 = CARTESIAN_POINT ( 'NONE',  ( -24.87351451566537364, -14.94990356866029657, 59.42955486997114178 ) ) ;
#47080 = CARTESIAN_POINT ( 'NONE',  ( -23.34481426128875015, -18.63642081788813343, 69.29371984264746231 ) ) ;
#47081 = FACE_OUTER_BOUND ( 'NONE', #40852, .T. ) ;
#47082 = ORIENTED_EDGE ( 'NONE', *, *, #15123, .T. ) ;
#47083 = CARTESIAN_POINT ( 'NONE',  ( -24.26805285345972152, -17.75277705495486558, 62.65077900732924121 ) ) ;
#47084 = EDGE_CURVE ( 'NONE', #1918, #1214, #7508, .T. ) ;
#47085 = CARTESIAN_POINT ( 'NONE',  ( -24.68443261157628754, -16.47976694508638573, 59.23058295855666699 ) ) ;
#47086 = CARTESIAN_POINT ( 'NONE',  ( -23.77312771997254615, -18.70709664074277612, 72.87872845841107505 ) ) ;
#47087 = CIRCLE ( 'NONE', #32155, 1.250000000000001110 ) ;
#47088 = CARTESIAN_POINT ( 'NONE',  ( -15.18259368501833961, -19.55664553709809894, 49.52966884056656482 ) ) ;
#47089 = CARTESIAN_POINT ( 'NONE',  ( -45.92409385541306222, 12.69079345525585545, 68.00000000000000000 ) ) ;
#47090 = ORIENTED_EDGE ( 'NONE', *, *, #13467, .F. ) ;
#47091 = DIRECTION ( 'NONE',  ( -0.9687793358424819923, 0.2479245821708680464, 0.000000000000000000 ) ) ;
#47092 = LINE ( 'NONE', #13333, #18732 ) ;
#47093 = CARTESIAN_POINT ( 'NONE',  ( -15.68503317936312236, -7.977064329016500643, 70.60989839961001735 ) ) ;
#47094 = DIRECTION ( 'NONE',  ( 1.000000000000000000, -6.938893903907222067E-14, 0.000000000000000000 ) ) ;
#47095 = EDGE_CURVE ( 'NONE', #18567, #24527, #10694, .T. ) ;
#47096 = CARTESIAN_POINT ( 'NONE',  ( -46.29409385541305966, -14.20920654474410760, 71.05212771298751306 ) ) ;
#47097 = DIRECTION ( 'NONE',  ( -0.000000000000000000, -1.000000000000000000, -0.000000000000000000 ) ) ;
#47098 = ORIENTED_EDGE ( 'NONE', *, *, #2445, .F. ) ;
#47099 = CARTESIAN_POINT ( 'NONE',  ( -21.18536505927766456, -21.24010891514583221, 65.84099883884408655 ) ) ;
#47100 = FACE_OUTER_BOUND ( 'NONE', #9725, .T. ) ;
#47101 = ORIENTED_EDGE ( 'NONE', *, *, #38111, .T. ) ;
#47102 = DIRECTION ( 'NONE',  ( 3.071710424422018668E-17, -6.404604876783312462E-16, -1.000000000000000000 ) ) ;
#47103 = CARTESIAN_POINT ( 'NONE',  ( -10.58454466348024425, -16.55148359085594478, 71.60317204484042009 ) ) ;
#47104 = CARTESIAN_POINT ( 'NONE',  ( -24.72409385541305582, -14.80920654474419962, 66.95294117647057419 ) ) ;
#47105 = CARTESIAN_POINT ( 'NONE',  ( -19.37638992839121954, -7.619477365241829503, 60.00447059577386710 ) ) ;
#47106 = CARTESIAN_POINT ( 'NONE',  ( -16.19814381282456495, -21.75179583453235210, 58.58585572026736088 ) ) ;
#47107 = ORIENTED_EDGE ( 'NONE', *, *, #19836, .T. ) ;
#47108 = CARTESIAN_POINT ( 'NONE',  ( -23.70135507383723805, -11.71146680393053607, 62.95218278684509983 ) ) ;
#47109 = CYLINDRICAL_SURFACE ( 'NONE', #13902, 0.1500000000000000222 ) ;
#47110 = CARTESIAN_POINT ( 'NONE',  ( -20.36536858953947515, -8.398766899984980938, 63.19632798853695022 ) ) ;
#47111 = EDGE_LOOP ( 'NONE', ( #12692, #3799, #25300, #7270, #23853 ) ) ;
#47112 =( LENGTH_UNIT ( ) NAMED_UNIT ( * ) SI_UNIT ( .MILLI., .METRE. ) );
#47113 = VECTOR ( 'NONE', #9443, 1000.000000000000000 ) ;
#47114 = CARTESIAN_POINT ( 'NONE',  ( -10.42782603960657895, -12.24862780158598596, 57.50670067860124135 ) ) ;
#47115 = CARTESIAN_POINT ( 'NONE',  ( -24.27556694116850977, -13.13524334109580671, 66.71735578995932769 ) ) ;
#47116 = DIRECTION ( 'NONE',  ( 0.9687793358424821033, -0.2479245821708678243, 0.000000000000000000 ) ) ;
#47117 = B_SPLINE_CURVE_WITH_KNOTS ( 'NONE', 3,
 ( #44622, #33020, #14777, #21961, #48296, #36958, #18746, #2755, #2997, #25900 ),
 .UNSPECIFIED., .F., .F.,
 ( 4, 2, 2, 2, 4 ),
 ( 0.000000000000000000, 0.2500000000000000000, 0.5000000000000000000, 0.7500000000000000000, 1.000000000000000000 ),
 .UNSPECIFIED. ) ;
#47118 = CARTESIAN_POINT ( 'NONE',  ( -20.97184585037232196, -20.90166497323120609, 65.59013753914614142 ) ) ;
#47119 = CONICAL_SURFACE ( 'NONE', #7800, 0.5560000000000009379, 0.06981317007976595157 ) ;
#47120 = CIRCLE ( 'NONE', #21177, 1.999999999999999112 ) ;
#47121 = ORIENTED_EDGE ( 'NONE', *, *, #13952, .F. ) ;
#47122 = VERTEX_POINT ( 'NONE', #37259 ) ;
#47123 = CARTESIAN_POINT ( 'NONE',  ( -16.78659385541304161, -7.222650657624104298, 49.61879703869476543 ) ) ;
#47124 = EDGE_CURVE ( 'NONE', #6337, #22785, #3546, .T. ) ;
#47125 = EDGE_CURVE ( 'NONE', #15992, #24162, #15617, .T. ) ;
#47126 = PLANE ( 'NONE',  #2817 ) ;
#47127 = CARTESIAN_POINT ( 'NONE',  ( -14.10880350886743173, -8.137386945752117740, 70.90770375044263574 ) ) ;
#47128 = VECTOR ( 'NONE', #31462, 1000.000000000000114 ) ;
#47129 =( BOUNDED_CURVE ( )  B_SPLINE_CURVE ( 3, ( #18819, #41224, #14595, #33827 ),
 .UNSPECIFIED., .F., .F. ) 
 B_SPLINE_CURVE_WITH_KNOTS ( ( 4, 4 ),
 ( 1.570796326794896780, 1.780235837034210622 ),
 .UNSPECIFIED. ) 
 CURVE ( )  GEOMETRIC_REPRESENTATION_ITEM ( )  RATIONAL_B_SPLINE_CURVE ( ( 1.000000000000000000, 0.9963479302455156006, 0.9963479302455156006, 1.000000000000000000 ) ) 
 REPRESENTATION_ITEM ( '' )  );
#47130 = ADVANCED_FACE ( 'NONE', ( #14590 ), #2813, .T. ) ;
#47131 = EDGE_CURVE ( 'NONE', #1174, #4066, #48357, .T. ) ;
#47132 = CARTESIAN_POINT ( 'NONE',  ( -22.95715174103553835, -10.52130167614524758, 59.88738023529671040 ) ) ;
#47133 = LINE ( 'NONE', #13615, #25398 ) ;
#47134 = ORIENTED_EDGE ( 'NONE', *, *, #38916, .T. ) ;
#47135 = CARTESIAN_POINT ( 'NONE',  ( -24.40217300928714650, -14.25566238011515274, 69.65275273531472067 ) ) ;
#47136 = B_SPLINE_CURVE_WITH_KNOTS ( 'NONE', 3,
 ( #21445, #16986, #17238, #32031, #24413, #31793, #32744, #47768, #35951, #35705 ),
 .UNSPECIFIED., .F., .F.,
 ( 4, 2, 2, 2, 4 ),
 ( 0.6272669072976915228, 0.7522669073147286722, 0.8772669073317658217, 1.002266907348802860, 1.127266907365840121 ),
 .UNSPECIFIED. ) ;
#47137 = DIRECTION ( 'NONE',  ( -0.9950649908465213356, -0.09922531930717198856, 4.894557008102619459E-08 ) ) ;
#47138 = ORIENTED_EDGE ( 'NONE', *, *, #25170, .T. ) ;
#47139 = CARTESIAN_POINT ( 'NONE',  ( -19.14114274275229377, -7.967774638140072696, 66.99252055880820933 ) ) ;
#47140 =( BOUNDED_CURVE ( )  B_SPLINE_CURVE ( 3, ( #5560, #20576, #16611, #6271 ),
 .UNSPECIFIED., .F., .F. ) 
 B_SPLINE_CURVE_WITH_KNOTS ( ( 4, 4 ),
 ( 0.5000000000000000000, 0.9074455897393635118 ),
 .UNSPECIFIED. ) 
 CURVE ( )  GEOMETRIC_REPRESENTATION_ITEM ( )  RATIONAL_B_SPLINE_CURVE ( ( 1.000000000000012657, 0.4567392136813371306, 0.3561768502900231614, 0.6983129098260846268 ) ) 
 REPRESENTATION_ITEM ( '' )  );
#47141 = CARTESIAN_POINT ( 'NONE',  ( -12.90644018576984386, -9.461596219648651385, 74.60306486165157480 ) ) ;
#47142 = EDGE_LOOP ( 'NONE', ( #8633, #14233 ) ) ;
#47143 = CARTESIAN_POINT ( 'NONE',  ( -12.85799447202792045, -15.86467737382985277, 52.02966884056656482 ) ) ;
#47144 = CARTESIAN_POINT ( 'NONE',  ( -10.75331705403316818, -16.93070056221711184, 57.98760548944069626 ) ) ;
#47145 = ORIENTED_EDGE ( 'NONE', *, *, #38795, .T. ) ;
#47146 = ADVANCED_FACE ( 'NONE', ( #3306 ), #10944, .T. ) ;
#47147 = CARTESIAN_POINT ( 'NONE',  ( -23.33759473803162621, -18.55732873115717041, 72.99198201251103058 ) ) ;
#47148 = VECTOR ( 'NONE', #15159, 1000.000000000000000 ) ;
#47149 = CARTESIAN_POINT ( 'NONE',  ( -24.71173182865732443, -13.26207253172215950, 59.46993791559596332 ) ) ;
#47150 = ORIENTED_EDGE ( 'NONE', *, *, #18161, .T. ) ;
#47151 = CARTESIAN_POINT ( 'NONE',  ( -17.81243367693841151, -24.25303685828974665, 53.49999999999995026 ) ) ;
#47152 = CYLINDRICAL_SURFACE ( 'NONE', #26617, 0.1500000000000032419 ) ;
#47153 = VECTOR ( 'NONE', #35464, 1000.000000000000000 ) ;
#47155 = CARTESIAN_POINT ( 'NONE',  ( -15.48424059001683339, -21.53504990492328375, 72.04575460974366763 ) ) ;
#47154 = CIRCLE ( 'NONE', #25921, 2.499999999999999556 ) ;
#47156 = CARTESIAN_POINT ( 'NONE',  ( -12.05806040642128707, -10.23620046216302448, 67.51368956197082127 ) ) ;
#47157 = CARTESIAN_POINT ( 'NONE',  ( -13.17364477763805652, -9.395196358873663556, 49.41429196092195042 ) ) ;
#47158 = DIRECTION ( 'NONE',  ( -0.000000000000000000, -1.000000000000000000, 0.000000000000000000 ) ) ;
#47159 = LINE ( 'NONE', #28200, #34562 ) ;
#47160 = CARTESIAN_POINT ( 'NONE',  ( -45.92409385541306222, -13.51240245935757578, 72.90425531914894464 ) ) ;
#47161 = ORIENTED_EDGE ( 'NONE', *, *, #19995, .F. ) ;
#47162 = CARTESIAN_POINT ( 'NONE',  ( -10.71495554099518088, -12.81234323494808436, 64.56836111193433680 ) ) ;
#47163 = CIRCLE ( 'NONE', #18824, 2.000000000000000000 ) ;
#47164 = DIRECTION ( 'NONE',  ( 9.444166279764887802E-07, -1.975884206576272611E-06, -0.9999999999976019183 ) ) ;
#47165 = EDGE_LOOP ( 'NONE', ( #24063, #22396, #16099, #37805, #43900 ) ) ;
#47166 = LINE ( 'NONE', #16379, #9800 ) ;
#47167 = ORIENTED_EDGE ( 'NONE', *, *, #24780, .F. ) ;
#47168 = ORIENTED_EDGE ( 'NONE', *, *, #35045, .F. ) ;
#47169 = ORIENTED_EDGE ( 'NONE', *, *, #20479, .T. ) ;
#47170 = DIRECTION ( 'NONE',  ( 0.000000000000000000, 0.000000000000000000, 1.000000000000000000 ) ) ;
#47171 = CARTESIAN_POINT ( 'NONE',  ( -17.42409385541305511, -14.80920654474410725, 47.99999999999998579 ) ) ;
#47172 = CARTESIAN_POINT ( 'NONE',  ( -16.07865488608826254, -7.939723797651444315, 63.67011030349581091 ) ) ;
#47173 = CARTESIAN_POINT ( 'NONE',  ( -16.91478550490786503, -21.84108428878278119, 72.18015306840750611 ) ) ;
#47174 = CARTESIAN_POINT ( 'NONE',  ( -16.28362587665221639, -22.17156497440846152, 61.91714677727144078 ) ) ;
#47175 = ORIENTED_EDGE ( 'NONE', *, *, #36128, .T. ) ;
#47176 = ORIENTED_EDGE ( 'NONE', *, *, #15990, .F. ) ;
#47177 = CARTESIAN_POINT ( 'NONE',  ( -18.11159385650551457, -6.922745924619793101, 51.69366785382590024 ) ) ;
#47178 = EDGE_CURVE ( 'NONE', #43657, #35776, #646, .T. ) ;
#47179 = CIRCLE ( 'NONE', #35361, 2.000000000000000000 ) ;
#47180 = DIRECTION ( 'NONE',  ( 3.549360974554993999E-17, -6.371834667797928663E-18, -1.000000000000000000 ) ) ;
#47181 = CARTESIAN_POINT ( 'NONE',  ( -24.06394650331561635, -17.02597731989300556, 72.88336026101553955 ) ) ;
#47182 = CARTESIAN_POINT ( 'NONE',  ( -18.50534385650551883, -8.801233750844183135, 48.81488406609782515 ) ) ;
#47183 = AXIS2_PLACEMENT_3D ( 'NONE', #37093, #18136, #6593 ) ;
#47184 = EDGE_CURVE ( 'NONE', #35420, #33399, #30539, .T. ) ;
#47186 = ORIENTED_EDGE ( 'NONE', *, *, #23072, .T. ) ;
#47185 = EDGE_CURVE ( 'NONE', #40875, #22320, #21777, .T. ) ;
#47187 = LINE ( 'NONE', #13182, #8037 ) ;
#47188 = B_SPLINE_CURVE_WITH_KNOTS ( 'NONE', 3,
 ( #35007, #16283, #42897, #9168, #39191, #20494, #30619, #1776, #11895, #23222 ),
 .UNSPECIFIED., .F., .F.,
 ( 4, 2, 2, 2, 4 ),
 ( 0.000000000000000000, 0.2500000000000000000, 0.5000000000000000000, 0.7500000000000000000, 1.000000000000000000 ),
 .UNSPECIFIED. ) ;
#47189 = ADVANCED_FACE ( 'NONE', ( #26208 ), #41219, .F. ) ;
#47190 = CARTESIAN_POINT ( 'NONE',  ( -24.37817933763783529, -15.98629254845087466, 69.94796348494512017 ) ) ;
#47191 = AXIS2_PLACEMENT_3D ( 'NONE', #34013, #33764, #18010 ) ;
#47192 = ADVANCED_FACE ( 'NONE', ( #30159 ), #21898, .T. ) ;
#47193 = ORIENTED_EDGE ( 'NONE', *, *, #9948, .F. ) ;
#47194 = DIRECTION ( 'NONE',  ( 0.7437128929774847741, -0.6684991644116392573, 1.736198598216997869E-08 ) ) ;
#47195 = PLANE ( 'NONE',  #22123 ) ;
#47196 = CARTESIAN_POINT ( 'NONE',  ( -16.24762640633412758, -21.70976015997750963, 58.28585518769421014 ) ) ;
#47197 = CARTESIAN_POINT ( 'NONE',  ( -14.45970594486164806, -7.974362378399544760, 63.89004585484453713 ) ) ;
#47198 = EDGE_CURVE ( 'NONE', #19672, #46068, #45899, .T. ) ;
#47199 = ORIENTED_EDGE ( 'NONE', *, *, #33706, .T. ) ;
#47200 = PLANE ( 'NONE',  #15529 ) ;
#47201 = CARTESIAN_POINT ( 'NONE',  ( -22.79874446983080816, -10.32434671450250008, 63.14473989550985067 ) ) ;
#47202 = CARTESIAN_POINT ( 'NONE',  ( -18.07488560852729975, -21.77899938210117980, 65.34532180047121130 ) ) ;
#47203 = ORIENTED_EDGE ( 'NONE', *, *, #30460, .T. ) ;
#47204 = CARTESIAN_POINT ( 'NONE',  ( -19.04784696903935881, -9.816619457272704352, 52.02966884056656482 ) ) ;
#47205 = ORIENTED_EDGE ( 'NONE', *, *, #14219, .F. ) ;
#47206 = CARTESIAN_POINT ( 'NONE',  ( -14.65765131015531253, -21.78034674156931061, 53.49999999999994316 ) ) ;
#47207 = CARTESIAN_POINT ( 'NONE',  ( -14.59148033128425404, -7.918538076466720810, 60.48029674573233905 ) ) ;
#47208 = VERTEX_POINT ( 'NONE', #45416 ) ;
#47209 = CARTESIAN_POINT ( 'NONE',  ( -10.33531692083374587, -17.10115316349580894, 57.87255846826901262 ) ) ;
#47210 = CARTESIAN_POINT ( 'NONE',  ( -10.85938897953544924, -12.23054697885984510, 57.74345952600154419 ) ) ;
#47211 = CARTESIAN_POINT ( 'NONE',  ( -16.87480544004084493, -7.378732441012598287, 74.07362965403005717 ) ) ;
#47212 = AXIS2_PLACEMENT_3D ( 'NONE', #23403, #5173, #12552 ) ;
#47213 = DIRECTION ( 'NONE',  ( -1.000000000000000000, 4.164305804376849172E-17, -1.614929280266638808E-16 ) ) ;
#47214 = ORIENTED_EDGE ( 'NONE', *, *, #16347, .T. ) ;
#47215 = CARTESIAN_POINT ( 'NONE',  ( -17.42409385541299471, -14.80920654474435771, 49.52966884056655772 ) ) ;
#47216 = AXIS2_PLACEMENT_3D ( 'NONE', #32994, #15257, #48513 ) ;
#47217 = CARTESIAN_POINT ( 'NONE',  ( -23.74454562765497556, -11.67923450027144305, 59.36747125042367657 ) ) ;
#47218 = DIRECTION ( 'NONE',  ( -3.071710424422018668E-17, 6.404604876783312462E-16, 1.000000000000000000 ) ) ;
#47219 = VERTEX_POINT ( 'NONE', #8235 ) ;
#47220 = CARTESIAN_POINT ( 'NONE',  ( -9.982716906467198115, -14.44908523835941594, 67.97304809435139816 ) ) ;
#47221 = CARTESIAN_POINT ( 'NONE',  ( -11.96084906401204506, -9.743958800322932490, 60.74413413563605957 ) ) ;
#47222 = ORIENTED_EDGE ( 'NONE', *, *, #21938, .F. ) ;
#47223 = ORIENTED_EDGE ( 'NONE', *, *, #6785, .T. ) ;
#47224 = CARTESIAN_POINT ( 'NONE',  ( -24.08977912471840810, -11.48169904069885661, 62.99572364416607684 ) ) ;
#47225 = DIRECTION ( 'NONE',  ( -3.071710424422018668E-17, 6.404604876783312462E-16, 1.000000000000000000 ) ) ;
#47226 = DIRECTION ( 'NONE',  ( 0.4439273849576908515, 0.8960627639203775363, -9.143653603063708001E-17 ) ) ;
#47227 = VECTOR ( 'NONE', #4788, 1000.000000000000000 ) ;
#47228 = CARTESIAN_POINT ( 'NONE',  ( -19.14909385650551954, -8.104110260919579645, 48.81699501597546487 ) ) ;
#47229 = CARTESIAN_POINT ( 'NONE',  ( -11.89179040387956832, -10.43929601004734486, 70.96893105543333036 ) ) ;
#47230 = CARTESIAN_POINT ( 'NONE',  ( -19.45448041399064110, -21.50840410520018509, 62.29503609332071079 ) ) ;
#47231 = EDGE_CURVE ( 'NONE', #44513, #21655, #11671, .T. ) ;
#47232 = CARTESIAN_POINT ( 'NONE',  ( -12.31380134045779506, -10.02538898168817916, 60.55918086676557976 ) ) ;
#47233 = CARTESIAN_POINT ( 'NONE',  ( -12.69763806180496601, -20.04058448603118592, 68.62185382311069759 ) ) ;
#47234 = CARTESIAN_POINT ( 'NONE',  ( -23.38560432932743538, -19.27844084936127800, 58.99755287451023378 ) ) ;
#47235 = ORIENTED_EDGE ( 'NONE', *, *, #36262, .T. ) ;
#47236 = EDGE_LOOP ( 'NONE', ( #35106, #13628, #14450, #4734 ) ) ;
#47237 = CARTESIAN_POINT ( 'NONE',  ( -24.42398663107514523, -15.65075326911586906, 73.01775867260030850 ) ) ;
#47238 = EDGE_CURVE ( 'NONE', #22618, #41894, #19801, .T. ) ;
#47239 = AXIS2_PLACEMENT_3D ( 'NONE', #25422, #11549, #37637 ) ;
#47240 = CARTESIAN_POINT ( 'NONE',  ( -21.94214292921110143, -20.15606996381378480, 58.76442870697494669 ) ) ;
#47241 = FACE_OUTER_BOUND ( 'NONE', #47957, .T. ) ;
#47242 = DIRECTION ( 'NONE',  ( -1.674255585786183705E-21, 0.9999746924698832418, 0.007114381193220235301 ) ) ;
#47243 = CARTESIAN_POINT ( 'NONE',  ( -10.57990114081760957, -13.11695186304740979, 71.22300718686658172 ) ) ;
#47244 = CARTESIAN_POINT ( 'NONE',  ( -21.23034385650552025, -9.794322478646142471, 51.19202720610083901 ) ) ;
#47245 = ORIENTED_EDGE ( 'NONE', *, *, #16541, .F. ) ;
#47246 = B_SPLINE_CURVE_WITH_KNOTS ( 'NONE', 3,
 ( #44400, #43436, #10182, #33273, #6719, #29126, #44177, #40682, #48082, #21017 ),
 .UNSPECIFIED., .F., .F.,
 ( 4, 2, 2, 2, 4 ),
 ( 0.000000000000000000, 0.2500000000000000000, 0.5000000000000000000, 0.7500000000000000000, 1.000000000000000000 ),
 .UNSPECIFIED. ) ;
#47247 = CYLINDRICAL_SURFACE ( 'NONE', #7626, 1.249999999999999334 ) ;
#47248 = CARTESIAN_POINT ( 'NONE',  ( -10.23610968374255314, -12.85046669463587143, 67.85336945107273721 ) ) ;
#47249 = EDGE_CURVE ( 'NONE', #42405, #15728, #11550, .T. ) ;
#47250 = CIRCLE ( 'NONE', #33840, 4.686500000000000554 ) ;
#47251 = CARTESIAN_POINT ( 'NONE',  ( -24.72409385541305582, -14.80920654474423159, 69.07058823529411029 ) ) ;
#47252 = CARTESIAN_POINT ( 'NONE',  ( -10.49189908542464700, -16.09426454567519116, 68.26295692486267797 ) ) ;
#47253 = EDGE_CURVE ( 'NONE', #6766, #26691, #26818, .T. ) ;
#47254 = EDGE_LOOP ( 'NONE', ( #5101, #27171 ) ) ;
#47255 = CIRCLE ( 'NONE', #7974, 5.000000000000000000 ) ;
#47256 = CARTESIAN_POINT ( 'NONE',  ( -24.41403467353552514, -14.40519207544021540, 69.84202309558250477 ) ) ;
#47257 = EDGE_CURVE ( 'NONE', #37730, #29698, #1304, .T. ) ;
#47258 = CYLINDRICAL_SURFACE ( 'NONE', #26724, 0.1500000000000081268 ) ;
#47259 = LINE ( 'NONE', #39378, #42410 ) ;
#47260 =( NAMED_UNIT ( * ) SI_UNIT ( $, .STERADIAN. ) SOLID_ANGLE_UNIT ( ) );
#47261 = CARTESIAN_POINT ( 'NONE',  ( -15.47038646904106329, -21.58309222549749506, 72.34575460768671462 ) ) ;
#47262 = EDGE_CURVE ( 'NONE', #1356, #7607, #23852, .T. ) ;
#47263 =( BOUNDED_CURVE ( )  B_SPLINE_CURVE ( 3, ( #19809, #27672, #34809, #19550 ),
 .UNSPECIFIED., .F., .F. ) 
 B_SPLINE_CURVE_WITH_KNOTS ( ( 4, 4 ),
 ( 0.000000000000000000, 0.4074455897393669535 ),
 .UNSPECIFIED. ) 
 CURVE ( )  GEOMETRIC_REPRESENTATION_ITEM ( )  RATIONAL_B_SPLINE_CURVE ( ( 1.000000000000000000, 0.4567392136813270276, 0.3561768502900284905, 0.6983129098261043888 ) ) 
 REPRESENTATION_ITEM ( '' )  );
#47264 = CARTESIAN_POINT ( 'NONE',  ( -24.45201636468676654, -14.25170757634699825, 69.95275273439749242 ) ) ;
#47265 = CARTESIAN_POINT ( 'NONE',  ( -11.43624710438022340, -19.24183451059727545, 71.83685881853561739 ) ) ;
#47266 = ORIENTED_EDGE ( 'NONE', *, *, #38227, .F. ) ;
#47267 = CYLINDRICAL_SURFACE ( 'NONE', #38518, 0.1500000000000051015 ) ;
#47268 = EDGE_LOOP ( 'NONE', ( #9132, #17168 ) ) ;
#47269 = CARTESIAN_POINT ( 'NONE',  ( -18.98390459359973548, -7.933620001262258192, 66.91543923465640376 ) ) ;
#47270 = CARTESIAN_POINT ( 'NONE',  ( -11.28563465779866526, -19.03109355880862452, 68.35656306278301031 ) ) ;
#47271 = ORIENTED_EDGE ( 'NONE', *, *, #45488, .F. ) ;
#47272 = CARTESIAN_POINT ( 'NONE',  ( -16.29760673242258306, -22.17363489859456038, 61.87072740723333197 ) ) ;
#47273 = VECTOR ( 'NONE', #17130, 1000.000000000000114 ) ;
#47274 = CARTESIAN_POINT ( 'NONE',  ( -13.33034385650551812, -9.794322478646142471, 51.19202720610083190 ) ) ;
#47275 = ORIENTED_EDGE ( 'NONE', *, *, #19760, .T. ) ;
#47276 = CARTESIAN_POINT ( 'NONE',  ( 23.62590614458706639, 1.890747609047893185, 50.53028072113869484 ) ) ;
#47277 = CARTESIAN_POINT ( 'NONE',  ( -20.74681640280920192, -8.591282160409747348, 59.84125268094840067 ) ) ;
#47278 = CARTESIAN_POINT ( 'NONE',  ( -16.32745258320347759, -21.77369344365219561, 61.77040269689842944 ) ) ;
#47279 = ORIENTED_EDGE ( 'NONE', *, *, #29131, .T. ) ;
#47281 = CARTESIAN_POINT ( 'NONE',  ( -19.74037869399712619, -21.88997799075047368, 65.61486212479920255 ) ) ;
#47280 =( BOUNDED_SURFACE ( )  B_SPLINE_SURFACE ( 3, 1, ( 
 ( #18885, #22332 ),
 ( #11258, #10529 ),
 ( #25535, #37331 ),
 ( #15407, #45252 ),
 ( #3618, #40797 ),
 ( #37576, #10760 ),
 ( #11494, #40548 ) ),
 .UNSPECIFIED., .T., .F., .F. ) 
 B_SPLINE_SURFACE_WITH_KNOTS ( ( 4, 3, 4 ),
 ( 2, 2 ),
 ( 0.000000000000000000, 0.5000000000000000000, 1.000000000000000000 ),
 ( 0.000000000000000000, 1.000000000000000000 ),
 .UNSPECIFIED. ) 
 GEOMETRIC_REPRESENTATION_ITEM ( )  RATIONAL_B_SPLINE_SURFACE ( (
 ( 1.000000000000000000, 1.000000000000000000),
 ( 0.3333333333333335369, 0.3333333333333330373),
 ( 0.3333333333333335369, 0.3333333333333330373),
 ( 1.000000000000000000, 1.000000000000000000),
 ( 0.3333333333333333703, 0.3333333333333333703),
 ( 0.3333333333333333703, 0.3333333333333333703),
 ( 1.000000000000000000, 1.000000000000000000) ) ) 
 REPRESENTATION_ITEM ( '' )  SURFACE ( )  );
#47282 = CARTESIAN_POINT ( 'NONE',  ( -20.78451513435706133, -21.00713107796517320, 62.12943504870421663 ) ) ;
#47283 = CARTESIAN_POINT ( 'NONE',  ( -23.65624121974494543, -11.51332442490694774, 66.42214514605622355 ) ) ;
#47284 = VECTOR ( 'NONE', #10367, 1000.000000000000114 ) ;
#47285 = CYLINDRICAL_SURFACE ( 'NONE', #41989, 2.500000000000000444 ) ;
#47286 = ORIENTED_EDGE ( 'NONE', *, *, #5756, .T. ) ;
#47287 = ORIENTED_EDGE ( 'NONE', *, *, #16384, .F. ) ;
#47288 = B_SPLINE_CURVE_WITH_KNOTS ( 'NONE', 3,
 ( #14773, #29843, #22703, #37438, #3480, #11126, #7200, #3986, #11364, #18246 ),
 .UNSPECIFIED., .F., .F.,
 ( 4, 2, 2, 2, 4 ),
 ( 0.000000000000000000, 0.2500000000000000000, 0.5000000000000000000, 0.7500000000000000000, 1.000000000000000000 ),
 .UNSPECIFIED. ) ;
#47289 = AXIS2_PLACEMENT_3D ( 'NONE', #14645, #11729, #33618 ) ;
#47290 = CARTESIAN_POINT ( 'NONE',  ( -23.81770139843839829, -18.63370553473270519, 72.92401558967065966 ) ) ;
#47291 = FACE_OUTER_BOUND ( 'NONE', #8466, .T. ) ;
#47292 = ORIENTED_EDGE ( 'NONE', *, *, #1728, .F. ) ;
#47293 = CARTESIAN_POINT ( 'NONE',  ( -17.71151671804478411, -7.815048565353869492, 60.36595428842180411 ) ) ;
#47294 = CARTESIAN_POINT ( 'NONE',  ( -24.90891992605694227, -15.28604896337863472, 53.49999999999994316 ) ) ;
#47295 = CARTESIAN_POINT ( 'NONE',  ( -20.24909385759799108, -8.112991634885936776, 51.74999426922421719 ) ) ;
#47296 = CARTESIAN_POINT ( 'NONE',  ( -12.48387464686926407, -19.84385436793359503, 68.42837419015026512 ) ) ;
#47297 = ADVANCED_FACE ( 'NONE', ( #38490 ), #5024, .T. ) ;
#47298 = CARTESIAN_POINT ( 'NONE',  ( -45.67409385541305511, -15.80920654474410725, 61.49999999999999289 ) ) ;
#47299 = CARTESIAN_POINT ( 'NONE',  ( -15.74783386771837890, -7.961078896070159061, 70.62461975990308360 ) ) ;
#47300 = AXIS2_PLACEMENT_3D ( 'NONE', #30677, #45700, #37055 ) ;
#47301 =( BOUNDED_SURFACE ( )  B_SPLINE_SURFACE ( 3, 1, ( 
 ( #32192, #13451 ),
 ( #39080, #13688 ),
 ( #31455, #28732 ),
 ( #28252, #43763 ),
 ( #43523, #43278 ),
 ( #28496, #43022 ),
 ( #24573, #42789 ) ),
 .UNSPECIFIED., .T., .F., .F. ) 
 B_SPLINE_SURFACE_WITH_KNOTS ( ( 4, 3, 4 ),
 ( 2, 2 ),
 ( 0.000000000000000000, 0.5000000000000000000, 1.000000000000000000 ),
 ( 0.000000000000000000, 1.000000000000000000 ),
 .UNSPECIFIED. ) 
 GEOMETRIC_REPRESENTATION_ITEM ( )  RATIONAL_B_SPLINE_SURFACE ( (
 ( 1.000000000000000000, 1.000000000000000000),
 ( 0.3333333333333335369, 0.3333333333333330373),
 ( 0.3333333333333335369, 0.3333333333333330373),
 ( 1.000000000000000000, 1.000000000000000000),
 ( 0.3333333333333333703, 0.3333333333333333703),
 ( 0.3333333333333333703, 0.3333333333333333703),
 ( 1.000000000000000000, 1.000000000000000000) ) ) 
 REPRESENTATION_ITEM ( '' )  SURFACE ( )  );
#47302 = VERTEX_POINT ( 'NONE', #22771 ) ;
#47303 = FACE_OUTER_BOUND ( 'NONE', #14095, .T. ) ;
#47304 = DIRECTION ( 'NONE',  ( -3.071710424422018668E-17, 6.404604876783312462E-16, 1.000000000000000000 ) ) ;
#47305 = VECTOR ( 'NONE', #6661, 1000.000000000000000 ) ;
#47306 = CARTESIAN_POINT ( 'NONE',  ( -12.76547314785493192, -9.517330534081262172, 74.60450883341005124 ) ) ;
#47307 = DIRECTION ( 'NONE',  ( 0.9687793358424821033, -0.2479245821708677133, 0.000000000000000000 ) ) ;
#47308 = B_SPLINE_CURVE_WITH_KNOTS ( 'NONE', 1,
 ( #25195, #9700 ),
 .UNSPECIFIED., .F., .F.,
 ( 2, 2 ),
 ( 0.000000000000000000, 1.000000000000000000 ),
 .UNSPECIFIED. ) ;
#47309 = ORIENTED_EDGE ( 'NONE', *, *, #2472, .T. ) ;
#47310 = ORIENTED_EDGE ( 'NONE', *, *, #39545, .T. ) ;
#47311 = CARTESIAN_POINT ( 'NONE',  ( -17.49728986656368335, -7.358816873484950172, 63.66401766577892118 ) ) ;
#47312 = CARTESIAN_POINT ( 'NONE',  ( -13.88293259567353743, -20.90532631576516565, 68.45625136994867432 ) ) ;
#47313 = EDGE_CURVE ( 'NONE', #9420, #10431, #25803, .T. ) ;
#47314 = CARTESIAN_POINT ( 'NONE',  ( -50.42609385541305755, -14.90920654474426499, 72.08823529411763786 ) ) ;
#47315 = ORIENTED_EDGE ( 'NONE', *, *, #8829, .F. ) ;
#47316 = DIRECTION ( 'NONE',  ( -1.000000000000000000, -1.669677910507523057E-21, -6.493791346278465266E-22 ) ) ;
#47317 = EDGE_CURVE ( 'NONE', #30116, #3548, #14976, .T. ) ;
#47318 = AXIS2_PLACEMENT_3D ( 'NONE', #12059, #2177, #29010 ) ;
#47319 = DIRECTION ( 'NONE',  ( 3.840743001415272461E-07, -4.934726759164745929E-06, 0.9999999999877503543 ) ) ;
#47320 = ORIENTED_EDGE ( 'NONE', *, *, #32412, .T. ) ;
#47321 = AXIS2_PLACEMENT_3D ( 'NONE', #7639, #14718, #37387 ) ;
#47322 = CARTESIAN_POINT ( 'NONE',  ( -11.35719102664687874, -18.40077844947705543, 58.09242476654641507 ) ) ;
#47323 = EDGE_CURVE ( 'NONE', #37416, #166, #31975, .T. ) ;
#47324 = FACE_OUTER_BOUND ( 'NONE', #38194, .T. ) ;
#47325 = ORIENTED_EDGE ( 'NONE', *, *, #30311, .F. ) ;
#47326 = CARTESIAN_POINT ( 'NONE',  ( -45.92409385541306222, -14.20017296387473316, 71.05663168951063824 ) ) ;
#47327 = ORIENTED_EDGE ( 'NONE', *, *, #12961, .T. ) ;
#47328 = DIRECTION ( 'NONE',  ( 0.000000000000000000, 1.000000000000000000, -0.000000000000000000 ) ) ;
#47329 = ORIENTED_EDGE ( 'NONE', *, *, #28283, .F. ) ;
#47330 = LINE ( 'NONE', #13794, #34678 ) ;
#47331 = CARTESIAN_POINT ( 'NONE',  ( -23.31997331754326197, -18.67484999725029127, 69.29931808629288525 ) ) ;
#47332 = FACE_OUTER_BOUND ( 'NONE', #7544, .T. ) ;
#47333 = ORIENTED_EDGE ( 'NONE', *, *, #6617, .F. ) ;
#47334 = FACE_OUTER_BOUND ( 'NONE', #28117, .T. ) ;
#47335 = CARTESIAN_POINT ( 'NONE',  ( -20.17401961043511704, -21.73324369436076964, 72.58195652652476326 ) ) ;
#47336 = DIRECTION ( 'NONE',  ( -0.3996021513128670266, -0.9166886716143755054, -9.834836654444679756E-09 ) ) ;
#47337 = VECTOR ( 'NONE', #11631, 1000.000000000000000 ) ;
#47338 = ADVANCED_FACE ( 'NONE', ( #23747 ), #45219, .T. ) ;
#47339 = CARTESIAN_POINT ( 'NONE',  ( -13.74195337878076018, -8.854397186113205365, 57.04138123197974863 ) ) ;
#47340 = CARTESIAN_POINT ( 'NONE',  ( -13.92409385541305511, -10.10920654474410618, 80.49999999999998579 ) ) ;
#47341 = CARTESIAN_POINT ( 'NONE',  ( -10.40647260758111869, -17.31080661122752673, 61.31776488722727692 ) ) ;
#47342 = ORIENTED_EDGE ( 'NONE', *, *, #28571, .T. ) ;
#47343 = CARTESIAN_POINT ( 'NONE',  ( -17.59211729576255934, -7.811223397794364587, 63.55057029380298417 ) ) ;
#47344 = ADVANCED_FACE ( 'NONE', ( #32561 ), #35529, .F. ) ;
#47345 = CARTESIAN_POINT ( 'NONE',  ( -11.81178692268928643, -10.62566621335946770, 74.43885052268630886 ) ) ;
#47346 = FACE_OUTER_BOUND ( 'NONE', #27263, .T. ) ;
#47347 = CARTESIAN_POINT ( 'NONE',  ( -13.60236376389480384, -20.73382277062339085, 61.80174179654961364 ) ) ;
#47348 = B_SPLINE_CURVE_WITH_KNOTS ( 'NONE', 1,
 ( #34974, #23919 ),
 .UNSPECIFIED., .F., .F.,
 ( 2, 2 ),
 ( 0.000000000000000000, 1.000000000000000000 ),
 .UNSPECIFIED. ) ;
#47349 = CARTESIAN_POINT ( 'NONE',  ( -19.91150868914413508, -21.83174586793584382, 69.04208316193926009 ) ) ;
#47350 = EDGE_CURVE ( 'NONE', #15944, #8174, #6526, .T. ) ;
#47351 = CARTESIAN_POINT ( 'NONE',  ( -11.89178903705324686, -10.43929771899554737, 71.26893105542536944 ) ) ;
#47352 = ORIENTED_EDGE ( 'NONE', *, *, #1209, .F. ) ;
#47353 = VERTEX_POINT ( 'NONE', #27663 ) ;
#47354 = CARTESIAN_POINT ( 'NONE',  ( -20.72253465480533308, -21.04901898548487793, 65.72887014617839441 ) ) ;
#47355 = DIRECTION ( 'NONE',  ( -1.616182858256118536E-16, -0.003028072113822188795, 0.9999954153791273948 ) ) ;
#47356 = ORIENTED_EDGE ( 'NONE', *, *, #37709, .F. ) ;
#47357 = CARTESIAN_POINT ( 'NONE',  ( -10.37172597770583415, -14.90377323363781414, 71.21294082064301278 ) ) ;
#47358 = FACE_OUTER_BOUND ( 'NONE', #25515, .T. ) ;
#47359 = CARTESIAN_POINT ( 'NONE',  ( -17.91451193640577344, -22.24313339626381847, 61.99040498927033127 ) ) ;
#47360 = CARTESIAN_POINT ( 'NONE',  ( -18.97948276208418150, -7.924750873940990203, 60.11659987143988815 ) ) ;
#47361 = CARTESIAN_POINT ( 'NONE',  ( -21.17774041181681710, -8.837307456416409579, 73.80948465004701120 ) ) ;
#47362 = ORIENTED_EDGE ( 'NONE', *, *, #18725, .F. ) ;
#47363 = CARTESIAN_POINT ( 'NONE',  ( -17.26571734983926021, -20.32036725976781355, 53.88362224778186516 ) ) ;
#47364 = CARTESIAN_POINT ( 'NONE',  ( -17.06879511326789611, -7.767867012253359071, 73.97490359703523666 ) ) ;
#47365 = DIRECTION ( 'NONE',  ( -2.866981220435666553E-17, 1.000000000000000000, 1.190614954331866791E-16 ) ) ;
#47366 = ORIENTED_EDGE ( 'NONE', *, *, #30908, .T. ) ;
#47367 = DIRECTION ( 'NONE',  ( -3.071710424422018668E-17, 6.404604876783312462E-16, 1.000000000000000000 ) ) ;
#47368 = CARTESIAN_POINT ( 'NONE',  ( -47.12338083056222615, -12.91120565595569758, 70.87000000000000455 ) ) ;
#47369 = CIRCLE ( 'NONE', #33948, 5.249999999999998224 ) ;
#47370 = CARTESIAN_POINT ( 'NONE',  ( -10.42546210075913748, -12.25520342886974845, 57.44361899967025664 ) ) ;
#47371 = CARTESIAN_POINT ( 'NONE',  ( -13.85515746416932004, -20.83112733177175713, 65.05916827336410790 ) ) ;
#47372 = CARTESIAN_POINT ( 'NONE',  ( -11.57411172585599424, -10.96269881181310701, 57.43733183567105982 ) ) ;
#47373 = ORIENTED_EDGE ( 'NONE', *, *, #36866, .T. ) ;
#47374 = VERTEX_POINT ( 'NONE', #35758 ) ;
#47375 = CARTESIAN_POINT ( 'NONE',  ( -16.28034385541304019, -9.360768649639302552, 51.01397948905922419 ) ) ;
#47376 = CARTESIAN_POINT ( 'NONE',  ( -10.91676103024768985, -17.53123951026858407, 64.62739371368721208 ) ) ;
#47377 = CARTESIAN_POINT ( 'NONE',  ( -10.37497031036790851, -14.69804325442274617, 71.47782692816423378 ) ) ;
#47378 =( BOUNDED_CURVE ( )  B_SPLINE_CURVE ( 3, ( #147, #15129, #30186, #37792 ),
 .UNSPECIFIED., .F., .F. ) 
 B_SPLINE_CURVE_WITH_KNOTS ( ( 4, 4 ),
 ( 0.4074455897393610693, 0.5000000000000000000 ),
 .UNSPECIFIED. ) 
 CURVE ( )  GEOMETRIC_REPRESENTATION_ITEM ( )  RATIONAL_B_SPLINE_CURVE ( ( 0.6983129098260949519, 0.7760317562606977582, 0.8765941196519987377, 0.9999999999999965583 ) ) 
 REPRESENTATION_ITEM ( '' )  );
#47379 = B_SPLINE_CURVE_WITH_KNOTS ( 'NONE', 1,
 ( #26811, #27283 ),
 .UNSPECIFIED., .F., .F.,
 ( 2, 2 ),
 ( 0.000000000000000000, 1.000000000000000000 ),
 .UNSPECIFIED. ) ;
#47380 = ADVANCED_FACE ( 'NONE', ( #16803 ), #13105, .T. ) ;
#47381 = CARTESIAN_POINT ( 'NONE',  ( -14.14027996024632117, -8.627251641784368985, 70.83843686035393716 ) ) ;
#47382 = CARTESIAN_POINT ( 'NONE',  ( -13.90805003106573068, -20.86209311441256986, 68.75625137331327608 ) ) ;
#47383 = ORIENTED_EDGE ( 'NONE', *, *, #30701, .F. ) ;
#47384 = CARTESIAN_POINT ( 'NONE',  ( -17.42260713176972686, -20.05920633423509258, 50.77966884056656482 ) ) ;
#47385 = LINE ( 'NONE', #41428, #42233 ) ;
#47386 = EDGE_LOOP ( 'NONE', ( #28096, #32152, #45727, #18551, #29306 ) ) ;
#47387 = CARTESIAN_POINT ( 'NONE',  ( -18.00016368654587851, -22.23706993494688788, 62.03569299701934625 ) ) ;
#47388 = CARTESIAN_POINT ( 'NONE',  ( -12.96069280291159309, -9.414713786589372191, 74.50850143233944323 ) ) ;
#47389 = ORIENTED_EDGE ( 'NONE', *, *, #30957, .F. ) ;
#47390 = FACE_OUTER_BOUND ( 'NONE', #46217, .T. ) ;
#47391 = CARTESIAN_POINT ( 'NONE',  ( -12.16754818860568932, -19.43427171616090376, 58.11609390261931196 ) ) ;
#47392 = VERTEX_POINT ( 'NONE', #23980 ) ;
#47393 = FACE_OUTER_BOUND ( 'NONE', #2698, .T. ) ;
#47394 = CARTESIAN_POINT ( 'NONE',  ( -24.39774143530919304, -13.72145442755526545, 73.27838554735291154 ) ) ;
#47395 = DIRECTION ( 'NONE',  ( -0.7658821528503489962, -0.6346126762488695228, 0.1033986416233894090 ) ) ;
#47396 = LINE ( 'NONE', #46667, #1679 ) ;
#47397 = ORIENTED_EDGE ( 'NONE', *, *, #27944, .T. ) ;
#47398 = CARTESIAN_POINT ( 'NONE',  ( -22.27803375191225399, -20.46189896727856095, 62.42094464928214848 ) ) ;
#47399 = DIRECTION ( 'NONE',  ( -4.116680906418232674E-07, -3.835121148322460978E-07, -0.9999999999998417932 ) ) ;
#47400 = EDGE_CURVE ( 'NONE', #38546, #33912, #36984, .T. ) ;
#47401 = CARTESIAN_POINT ( 'NONE',  ( -19.78055771692377363, -21.45376424143257310, 68.93482482294113822 ) ) ;
#47402 = B_SPLINE_CURVE_WITH_KNOTS ( 'NONE', 3,
 ( #1955, #35439, #13743, #17202, #16717, #28786, #40121, #1724, #18659, #22616 ),
 .UNSPECIFIED., .F., .F.,
 ( 4, 2, 2, 2, 4 ),
 ( 0.1272669073658322658, 0.2522669073463165712, 0.3772669073268009043, 0.5022669073072851820, 0.6272669072877694596 ),
 .UNSPECIFIED. ) ;
#47403 = EDGE_CURVE ( 'NONE', #10587, #2752, #21096, .T. ) ;
#47404 = EDGE_CURVE ( 'NONE', #41130, #46821, #42044, .T. ) ;
#47405 = DIRECTION ( 'NONE',  ( 0.9687793358424821033, -0.2479245821708678243, 0.000000000000000000 ) ) ;
#47406 = FACE_OUTER_BOUND ( 'NONE', #23595, .T. ) ;
#47407 = DIRECTION ( 'NONE',  ( -3.549360974551883545E-17, 6.371834667872732552E-18, 1.000000000000000000 ) ) ;
#47408 = DIRECTION ( 'NONE',  ( 0.9687793358424802159, -0.2479245821708749020, 0.000000000000000000 ) ) ;
#47409 = ORIENTED_EDGE ( 'NONE', *, *, #31798, .F. ) ;
#47410 = LINE ( 'NONE', #47642, #23757 ) ;
#47411 = CARTESIAN_POINT ( 'NONE',  ( 18.57590614458706924, 1.644457370994464540, 49.30478444670960414 ) ) ;
#47412 = DIRECTION ( 'NONE',  ( -1.000000000000000000, -2.866981220435666553E-17, -0.000000000000000000 ) ) ;
#47413 = ORIENTED_EDGE ( 'NONE', *, *, #32893, .T. ) ;
#47414 = CARTESIAN_POINT ( 'NONE',  ( -45.55409385541305767, -14.20920654474410760, 69.94787228701220272 ) ) ;
#47415 = ORIENTED_EDGE ( 'NONE', *, *, #40294, .T. ) ;
#47416 = ORIENTED_EDGE ( 'NONE', *, *, #21152, .F. ) ;
#47417 = EDGE_LOOP ( 'NONE', ( #15100, #4608 ) ) ;
#47418 = DIRECTION ( 'NONE',  ( 1.224646799147353207E-16, 1.000000000000000000, -1.912410701131276611E-32 ) ) ;
#47419 = DIRECTION ( 'NONE',  ( -0.6538427738826437796, -0.7566304428460742804, 5.916677973164435741E-08 ) ) ;
#47420 =( BOUNDED_SURFACE ( )  B_SPLINE_SURFACE ( 3, 1, ( 
 ( #45276, #37360 ),
 ( #10789, #41569 ),
 ( #18651, #48706 ),
 ( #22131, #34161 ),
 ( #3399, #3645 ),
 ( #11523, #456 ),
 ( #14947, #30007 ) ),
 .UNSPECIFIED., .T., .F., .F. ) 
 B_SPLINE_SURFACE_WITH_KNOTS ( ( 4, 3, 4 ),
 ( 2, 2 ),
 ( 0.000000000000000000, 0.5000000000000000000, 1.000000000000000000 ),
 ( 0.000000000000000000, 1.000000000000000000 ),
 .UNSPECIFIED. ) 
 GEOMETRIC_REPRESENTATION_ITEM ( )  RATIONAL_B_SPLINE_SURFACE ( (
 ( 1.000000000000000000, 1.000000000000000000),
 ( 0.3333333333333335369, 0.3333333333333330373),
 ( 0.3333333333333335369, 0.3333333333333330373),
 ( 1.000000000000000000, 1.000000000000000000),
 ( 0.3333333333333333703, 0.3333333333333333703),
 ( 0.3333333333333333703, 0.3333333333333333703),
 ( 1.000000000000000000, 1.000000000000000000) ) ) 
 REPRESENTATION_ITEM ( '' )  SURFACE ( )  );
#47421 = CARTESIAN_POINT ( 'NONE',  ( -16.07865109465781117, -7.939724484389961034, 63.97011030347106697 ) ) ;
#47422 = CARTESIAN_POINT ( 'NONE',  ( -21.82409385759798681, -9.359200813967568422, 50.49621490985803263 ) ) ;
#47423 = ORIENTED_EDGE ( 'NONE', *, *, #7123, .T. ) ;
#47424 = ORIENTED_EDGE ( 'NONE', *, *, #18017, .T. ) ;
#47425 = B_SPLINE_CURVE_WITH_KNOTS ( 'NONE', 3,
 ( #28212, #31905, #32154, #13887, #24769, #24537, #17829, #21063, #28929, #36066 ),
 .UNSPECIFIED., .F., .F.,
 ( 4, 2, 2, 2, 4 ),
 ( 0.000000000000000000, 0.2500000000000000000, 0.5000000000000000000, 0.7500000000000000000, 1.000000000000000000 ),
 .UNSPECIFIED. ) ;
#47426 = CARTESIAN_POINT ( 'NONE',  ( -17.83034385650551457, -9.794322478646142471, 51.19202720610083901 ) ) ;
#47427 = EDGE_CURVE ( 'NONE', #17956, #29624, #9446, .T. ) ;
#47428 = CARTESIAN_POINT ( 'NONE',  ( -20.72450927900464634, -21.03929139025762751, 58.93003081252663833 ) ) ;
#47429 = CARTESIAN_POINT ( 'NONE',  ( -23.23831428902490259, -18.70736991730898424, 65.83891806926222046 ) ) ;
#47430 = CARTESIAN_POINT ( 'NONE',  ( -18.95534385650551457, -7.417179338643134834, 52.18511593390279302 ) ) ;
#47431 =( BOUNDED_CURVE ( )  B_SPLINE_CURVE ( 3, ( #40416, #47573, #40185, #33006 ),
 .UNSPECIFIED., .F., .F. ) 
 B_SPLINE_CURVE_WITH_KNOTS ( ( 4, 4 ),
 ( 4.712388980384690562, 4.921828490624011287 ),
 .UNSPECIFIED. ) 
 CURVE ( )  GEOMETRIC_REPRESENTATION_ITEM ( )  RATIONAL_B_SPLINE_CURVE ( ( 1.000000000000000000, 0.9963479302455154896, 0.9963479302455154896, 1.000000000000000000 ) ) 
 REPRESENTATION_ITEM ( '' )  );
#47432 = VERTEX_POINT ( 'NONE', #9692 ) ;
#47433 = CARTESIAN_POINT ( 'NONE',  ( -10.37382936219775154, -14.83089353207902228, 74.81251018390588570 ) ) ;
#47434 = EDGE_CURVE ( 'NONE', #29684, #26512, #34992, .T. ) ;
#47435 = DIRECTION ( 'NONE',  ( 0.9687793358424821033, -0.2479245821708680464, 0.000000000000000000 ) ) ;
#47436 = VERTEX_POINT ( 'NONE', #38982 ) ;
#47437 = DIRECTION ( 'NONE',  ( 1.000000000000000000, 2.866981220435666553E-17, 0.000000000000000000 ) ) ;
#47438 = VERTEX_POINT ( 'NONE', #8962 ) ;
#47439 = DIRECTION ( 'NONE',  ( 0.9687793358424811041, -0.2479245821708714881, 0.000000000000000000 ) ) ;
#47440 = LINE ( 'NONE', #36335, #23427 ) ;
#47441 = CARTESIAN_POINT ( 'NONE',  ( -22.48237781098097798, -19.73147542146173450, 65.85988959519353614 ) ) ;
#47442 = VECTOR ( 'NONE', #15802, 1000.000000000000000 ) ;
#47443 = ORIENTED_EDGE ( 'NONE', *, *, #19223, .T. ) ;
#47444 = CARTESIAN_POINT ( 'NONE',  ( -45.92409385541306222, -14.20920654474410760, 70.50000000000000000 ) ) ;
#47445 = CARTESIAN_POINT ( 'NONE',  ( -18.48574975592938330, -21.77885183246672796, 72.28510966583125708 ) ) ;
#47446 = DIRECTION ( 'NONE',  ( 0.9441784275685842776, -0.3294345108122635479, -1.993146885056044100E-08 ) ) ;
#47447 = ORIENTED_EDGE ( 'NONE', *, *, #37163, .F. ) ;
#47448 = CARTESIAN_POINT ( 'NONE',  ( -24.72409385541305582, -14.80920654474423159, 69.07058823529411029 ) ) ;
#47449 = FACE_OUTER_BOUND ( 'NONE', #20317, .T. ) ;
#47450 = EDGE_LOOP ( 'NONE', ( #39190, #37217, #475, #37820, #46237 ) ) ;
#47451 = CARTESIAN_POINT ( 'NONE',  ( -13.49267557974227394, -8.956801037788498121, 60.45422421514565059 ) ) ;
#47452 = CARTESIAN_POINT ( 'NONE',  ( -9.983332390312334326, -14.43496380782568522, 68.01946623190198693 ) ) ;
#47453 = EDGE_LOOP ( 'NONE', ( #8335, #2398, #32355, #11320 ) ) ;
#47454 = EDGE_CURVE ( 'NONE', #36141, #23362, #24472, .T. ) ;
#47455 = EDGE_CURVE ( 'NONE', #5810, #18099, #5257, .T. ) ;
#47456 = DIRECTION ( 'NONE',  ( -0.9132646967824438189, 0.4073666574609055568, -8.344532079829881716E-09 ) ) ;
#47457 = CARTESIAN_POINT ( 'NONE',  ( -13.93897074462874919, -20.93787812888889377, 68.74153005185598886 ) ) ;
#47458 = CARTESIAN_POINT ( 'NONE',  ( -16.94458744105653381, -7.374567917109038362, 74.14513580114275726 ) ) ;
#47459 = CARTESIAN_POINT ( 'NONE',  ( -21.17797108042288912, -21.24447908004819041, 65.76266720218958994 ) ) ;
#47460 = VERTEX_POINT ( 'NONE', #16564 ) ;
#47461 = CARTESIAN_POINT ( 'NONE',  ( -19.71801720247071543, -10.72249662993226060, 49.52966884056655772 ) ) ;
#47462 = CARTESIAN_POINT ( 'NONE',  ( -19.05423358200063433, -7.539568773092505616, 67.06218330876637879 ) ) ;
#47463 = FACE_OUTER_BOUND ( 'NONE', #35233, .T. ) ;
#47464 = ORIENTED_EDGE ( 'NONE', *, *, #9405, .F. ) ;
#47465 = CARTESIAN_POINT ( 'NONE',  ( -23.97453657302211028, -17.42552933921582436, 62.68181000447317786 ) ) ;
#47466 = ADVANCED_FACE ( 'NONE', ( #31605 ), #47070, .T. ) ;
#47467 = EDGE_CURVE ( 'NONE', #46391, #27633, #21493, .T. ) ;
#47468 = CARTESIAN_POINT ( 'NONE',  ( -15.65212752116712558, -9.867280269464721698, 52.02966884056656482 ) ) ;
#47469 = ORIENTED_EDGE ( 'NONE', *, *, #20495, .T. ) ;
#47470 = ORIENTED_EDGE ( 'NONE', *, *, #10979, .F. ) ;
#47471 = ADVANCED_FACE ( 'NONE', ( #11131 ), #8389, .T. ) ;
#47472 = CARTESIAN_POINT ( 'NONE',  ( -23.40706704545067041, -18.44294168544361057, 72.76368236816873036 ) ) ;
#47473 = DIRECTION ( 'NONE',  ( -3.071710424422018668E-17, 6.404604876783312462E-16, 1.000000000000000000 ) ) ;
#47474 = CARTESIAN_POINT ( 'NONE',  ( -15.95707209241614422, -7.504986913482371236, 63.85506412386598640 ) ) ;
#47475 = CARTESIAN_POINT ( 'NONE',  ( -16.73034385650551670, -9.794322478646142471, 51.19202720610083901 ) ) ;
#47476 = ADVANCED_FACE ( 'NONE', ( #44385 ), #25184, .T. ) ;
#47477 = CARTESIAN_POINT ( 'NONE',  ( -10.53536195276627829, -13.30851587854854401, 74.69289754060230280 ) ) ;
#47478 = CARTESIAN_POINT ( 'NONE',  ( -24.25486363958986757, -13.06355980472538469, 63.11792038370487035 ) ) ;
#47479 = CARTESIAN_POINT ( 'NONE',  ( -14.93036899495222869, -8.267093141589578309, 60.54826067984155458 ) ) ;
#47480 = CARTESIAN_POINT ( 'NONE',  ( 18.57590614458706924, 2.144561833755798563, 49.27104351578925900 ) ) ;
#47481 = CARTESIAN_POINT ( 'NONE',  ( -13.83108299072750391, -21.33561835983412891, 72.04112301026525245 ) ) ;
#47482 = EDGE_LOOP ( 'NONE', ( #985, #12763, #44033, #24812, #19485 ) ) ;
#47483 = ORIENTED_EDGE ( 'NONE', *, *, #36323, .F. ) ;
#47484 = CYLINDRICAL_SURFACE ( 'NONE', #32070, 1.999999999999999112 ) ;
#47485 = ADVANCED_FACE ( 'NONE', ( #3738 ), #13403, .T. ) ;
#47486 = VECTOR ( 'NONE', #15013, 1000.000000000000114 ) ;
#47487 = CARTESIAN_POINT ( 'NONE',  ( -17.00410685006708178, -7.771727545396207582, 73.96018273221115180 ) ) ;
#47488 = CARTESIAN_POINT ( 'NONE',  ( -14.80261092528313327, -21.30118148935308042, 61.86430222708096949 ) ) ;
#47489 = DIRECTION ( 'NONE',  ( 0.4749924142254752790, 0.8799898899579782219, 8.916637575808904455E-09 ) ) ;
#47490 = CARTESIAN_POINT ( 'NONE',  ( -11.10552337692560876, -11.79633671024259911, 71.38860856928842225 ) ) ;
#47491 = CARTESIAN_POINT ( 'NONE',  ( -19.54284385650551670, -8.811426318492348031, 52.18089403414751359 ) ) ;
#47492 = VERTEX_POINT ( 'NONE', #36478 ) ;
#47493 = CARTESIAN_POINT ( 'NONE',  ( -20.16691211377460391, -21.73601867580754288, 72.58974061177721637 ) ) ;
#47494 = CARTESIAN_POINT ( 'NONE',  ( -19.98813040044048606, -21.37641421727040125, 72.40478737316021807 ) ) ;
#47495 = DIRECTION ( 'NONE',  ( -3.071710424422018668E-17, 6.404604876783312462E-16, 1.000000000000000000 ) ) ;
#47496 = CARTESIAN_POINT ( 'NONE',  ( -10.51631473918724780, -16.23308084970759069, 67.86278957288837432 ) ) ;
#47497 = ORIENTED_EDGE ( 'NONE', *, *, #30594, .F. ) ;
#47498 = CARTESIAN_POINT ( 'NONE',  ( -13.47245494993759607, -21.12492725511472003, 65.10133600691351319 ) ) ;
#47499 = DIRECTION ( 'NONE',  ( 0.000000000000000000, 0.000000000000000000, -1.000000000000000000 ) ) ;
#47500 = CARTESIAN_POINT ( 'NONE',  ( -50.42609385541305755, -14.80920654474416942, 63.93529411764704662 ) ) ;
#47501 = EDGE_CURVE ( 'NONE', #30521, #38535, #14059, .T. ) ;
#47502 = DIRECTION ( 'NONE',  ( -3.071710424422018668E-17, 6.404604876783312462E-16, 1.000000000000000000 ) ) ;
#47503 = ORIENTED_EDGE ( 'NONE', *, *, #46637, .F. ) ;
#47504 = CARTESIAN_POINT ( 'NONE',  ( -19.24025795797341942, -7.996846695050864540, 60.24620885950562865 ) ) ;
#47505 = ORIENTED_EDGE ( 'NONE', *, *, #33405, .T. ) ;
#47506 = CIRCLE ( 'NONE', #32567, 2.000000000000001776 ) ;
#47507 = B_SPLINE_CURVE_WITH_KNOTS ( 'NONE', 1,
 ( #25802, #22121 ),
 .UNSPECIFIED., .F., .F.,
 ( 2, 2 ),
 ( 0.000000000000000000, 1.000000000000000000 ),
 .UNSPECIFIED. ) ;
#47508 = CARTESIAN_POINT ( 'NONE',  ( -12.87649578556737318, -13.67667219862661021, 49.52966884056655772 ) ) ;
#47509 = CARTESIAN_POINT ( 'NONE',  ( -11.28985232898421742, -19.03713839270133690, 68.39502420285157314 ) ) ;
#47510 = ORIENTED_EDGE ( 'NONE', *, *, #7232, .T. ) ;
#47511 = EDGE_CURVE ( 'NONE', #7864, #26003, #2118, .T. ) ;
#47512 = CARTESIAN_POINT ( 'NONE',  ( -23.08280660609100110, -10.60377317445056811, 59.61675562601556067 ) ) ;
#47513 = AXIS2_PLACEMENT_3D ( 'NONE', #26930, #577, #45660 ) ;
#47514 = CARTESIAN_POINT ( 'NONE',  ( -15.24284385650551599, -8.811426318492348031, 52.18089403414752070 ) ) ;
#47515 = ORIENTED_EDGE ( 'NONE', *, *, #42408, .T. ) ;
#47516 = CARTESIAN_POINT ( 'NONE',  ( -13.33738394060092070, -12.51528319768659436, 52.02966884056656482 ) ) ;
#47517 = CARTESIAN_POINT ( 'NONE',  ( -24.72409385541305582, -14.90920654474426321, 72.08823529411763786 ) ) ;
#47518 = CARTESIAN_POINT ( 'NONE',  ( -23.89200535028185612, -11.11192396016905448, 70.07706043178237110 ) ) ;
#47519 = EDGE_LOOP ( 'NONE', ( #15653, #9376, #31423, #38309, #27349 ) ) ;
#47520 = DIRECTION ( 'NONE',  ( 0.6562885720885137664, -0.7545099801500438907, -1.193821365372358186E-08 ) ) ;
#47521 = FACE_OUTER_BOUND ( 'NONE', #14563, .T. ) ;
#47522 = CARTESIAN_POINT ( 'NONE',  ( -12.05483347687720475, -10.31798811457585963, 67.79896870046731294 ) ) ;
#47523 = CARTESIAN_POINT ( 'NONE',  ( -23.24618082141521214, -10.81943526098172548, 59.74636554153219237 ) ) ;
#47524 = ORIENTED_EDGE ( 'NONE', *, *, #25919, .T. ) ;
#47525 = ORIENTED_EDGE ( 'NONE', *, *, #12416, .F. ) ;
#47526 = EDGE_CURVE ( 'NONE', #6762, #1918, #48541, .T. ) ;
#47527 = CARTESIAN_POINT ( 'NONE',  ( -20.02395964528090033, -18.70843468947692045, 49.52966884056656482 ) ) ;
#47528 = CARTESIAN_POINT ( 'NONE',  ( -14.97035482569482312, -21.41873484682592377, 61.92128389535452015 ) ) ;
#47529 = VERTEX_POINT ( 'NONE', #44879 ) ;
#47530 = CARTESIAN_POINT ( 'NONE',  ( -17.71116635333902778, -7.815035665054884007, 60.09563220684449192 ) ) ;
#47531 = CARTESIAN_POINT ( 'NONE',  ( -17.15534385759799108, -8.623186033802570094, 49.24843789510466507 ) ) ;
#47532 = EDGE_CURVE ( 'NONE', #41905, #35459, #20356, .T. ) ;
#47533 = CARTESIAN_POINT ( 'NONE',  ( -24.08907123645992243, -11.48026457312919391, 63.13713595337925000 ) ) ;
#47534 = CARTESIAN_POINT ( 'NONE',  ( -26.42409385541305511, -6.359206544744109735, 63.99999999999998579 ) ) ;
#47535 = CARTESIAN_POINT ( 'NONE',  ( -23.70394581819067170, -18.81767069530084058, 69.41559189047532641 ) ) ;
#47536 = ORIENTED_EDGE ( 'NONE', *, *, #22040, .T. ) ;
#47537 = CARTESIAN_POINT ( 'NONE',  ( -16.39155704513022016, -21.78318439201321866, 61.75568132354042916 ) ) ;
#47538 = CARTESIAN_POINT ( 'NONE',  ( -20.70232472158584969, -8.624289250480600799, 59.84125250310036392 ) ) ;
#47539 = DIRECTION ( 'NONE',  ( 2.168404344971008375E-16, 0.000000000000000000, -1.000000000000000000 ) ) ;
#47540 = LINE ( 'NONE', #6175, #15876 ) ;
#47541 = EDGE_CURVE ( 'NONE', #32972, #29603, #39714, .T. ) ;
#47542 = VERTEX_POINT ( 'NONE', #34746 ) ;
#47543 = AXIS2_PLACEMENT_3D ( 'NONE', #966, #12046, #46265 ) ;
#47544 = VERTEX_POINT ( 'NONE', #34246 ) ;
#47545 = PRODUCT_RELATED_PRODUCT_CATEGORY ( 'part', '', ( #42558 ) ) ;
#47546 = CARTESIAN_POINT ( 'NONE',  ( -24.87453101240845399, -14.74101577129048835, 62.89951734912977344 ) ) ;
#47547 = AXIS2_PLACEMENT_3D ( 'NONE', #40072, #3117, #48178 ) ;
#47548 =( LENGTH_UNIT ( ) NAMED_UNIT ( * ) SI_UNIT ( .MILLI., .METRE. ) );
#47549 = DIRECTION ( 'NONE',  ( -1.000000000000000000, -2.866981220435666553E-17, -0.000000000000000000 ) ) ;
#47550 =( BOUNDED_CURVE ( )  B_SPLINE_CURVE ( 3, ( #35024, #23239, #37993, #23965 ),
 .UNSPECIFIED., .F., .F. ) 
 B_SPLINE_CURVE_WITH_KNOTS ( ( 4, 4 ),
 ( 0.000000000000000000, 0.4074455897393653991 ),
 .UNSPECIFIED. ) 
 CURVE ( )  GEOMETRIC_REPRESENTATION_ITEM ( )  RATIONAL_B_SPLINE_CURVE ( ( 1.000000000000000000, 0.4567392136813279713, 0.3561768502900288236, 0.6983129098261023904 ) ) 
 REPRESENTATION_ITEM ( '' )  );
#47551 = ORIENTED_EDGE ( 'NONE', *, *, #46810, .T. ) ;
#47552 = CARTESIAN_POINT ( 'NONE',  ( -23.79034794155987598, -17.71981930740736999, 59.28913082385783895 ) ) ;
#47553 = ORIENTED_EDGE ( 'NONE', *, *, #23329, .T. ) ;
#47554 = CARTESIAN_POINT ( 'NONE',  ( -36.42409385541304800, -6.859212275519750435, 50.50378509014258555 ) ) ;
#47555 = CARTESIAN_POINT ( 'NONE',  ( -19.73055724314207282, -21.89319082171075337, 65.66497415329939713 ) ) ;
#47556 = CARTESIAN_POINT ( 'NONE',  ( -15.75511905958810033, -8.011018546364985227, 67.21295221587696744 ) ) ;
#47557 = EDGE_CURVE ( 'NONE', #22189, #6093, #23685, .T. ) ;
#47558 = VERTEX_POINT ( 'NONE', #4463 ) ;
#47559 =( BOUNDED_CURVE ( )  B_SPLINE_CURVE ( 3, ( #38632, #26587, #41606, #12289 ),
 .UNSPECIFIED., .F., .F. ) 
 B_SPLINE_CURVE_WITH_KNOTS ( ( 4, 4 ),
 ( 0.5000000000000000000, 0.9074455897393673975 ),
 .UNSPECIFIED. ) 
 CURVE ( )  GEOMETRIC_REPRESENTATION_ITEM ( )  RATIONAL_B_SPLINE_CURVE ( ( 1.000000000000042411, 0.4567392136813354098, 0.3561768502900019562, 0.6983129098260876244 ) ) 
 REPRESENTATION_ITEM ( '' )  );
#47560 = DIRECTION ( 'NONE',  ( 0.000000000000000000, 0.000000000000000000, 1.000000000000000000 ) ) ;
#47561 = VERTEX_POINT ( 'NONE', #12338 ) ;
#47562 = FACE_OUTER_BOUND ( 'NONE', #5016, .T. ) ;
#47563 = DIRECTION ( 'NONE',  ( 4.734277565933067533E-07, -1.363385193985295737E-06, -0.9999999999989586108 ) ) ;
#47564 = DIRECTION ( 'NONE',  ( 0.5327540375067998379, 0.8462701315302333382, 7.203825861310634525E-08 ) ) ;
#47565 = ORIENTED_EDGE ( 'NONE', *, *, #42342, .F. ) ;
#47566 = CARTESIAN_POINT ( 'NONE',  ( -15.15660932275500272, -21.48492473237050859, 65.39124617759186719 ) ) ;
#47567 = B_SPLINE_CURVE_WITH_KNOTS ( 'NONE', 3,
 ( #40522, #30201, #11464, #6800, #46178, #9000, #24023, #23052, #23536, #20071 ),
 .UNSPECIFIED., .F., .F.,
 ( 4, 2, 2, 2, 4 ),
 ( 0.000000000000000000, 0.2500000000000000000, 0.5000000000000000000, 0.7500000000000000000, 1.000000000000000000 ),
 .UNSPECIFIED. ) ;
#47568 = CARTESIAN_POINT ( 'NONE',  ( -45.55409385541306477, -12.76354662275040397, 71.04301729251712061 ) ) ;
#47569 = DIRECTION ( 'NONE',  ( 3.811252424767960347E-06, 6.838859004561632622E-06, 0.9999999999693520714 ) ) ;
#47570 = CARTESIAN_POINT ( 'NONE',  ( -11.64235026963700115, -18.84330375823651949, 68.21689631561287115 ) ) ;
#47571 = B_SPLINE_CURVE_WITH_KNOTS ( 'NONE', 1,
 ( #19896, #34903 ),
 .UNSPECIFIED., .F., .F.,
 ( 2, 2 ),
 ( 0.000000000000000000, 1.000000000000000000 ),
 .UNSPECIFIED. ) ;
#47572 = ORIENTED_EDGE ( 'NONE', *, *, #43538, .F. ) ;
#47573 = CARTESIAN_POINT ( 'NONE',  ( -12.02413026160302323, -13.69638637514736956, 53.69233794759168887 ) ) ;
#47574 =( BOUNDED_CURVE ( )  B_SPLINE_CURVE ( 2, ( #31500, #24363, #31254, #28297, #27564, #42829, #28039, #9345, #9102 ),
 .UNSPECIFIED., .F., .F. ) 
 B_SPLINE_CURVE_WITH_KNOTS ( ( 3, 2, 2, 2, 3 ),
 ( 0.08261480023356829183, 0.08359842501002882897, 0.08458204978648936612, 0.08556567456294990326, 0.08654929933941044040 ),
 .UNSPECIFIED. ) 
 CURVE ( )  GEOMETRIC_REPRESENTATION_ITEM ( )  RATIONAL_B_SPLINE_CURVE ( ( 0.9999999999998482325, 0.9238795325114385060, 1.000000000000000000, 0.9238795325112867385, 1.000000000000000000, 0.9238795325112867385, 1.000000000000000000, 0.9238795325112502121, 1.000000000000036415 ) ) 
 REPRESENTATION_ITEM ( '' )  );
#47575 = DIRECTION ( 'NONE',  ( 4.615129112206533859E-07, -1.699487772732772144E-08, 0.9999999999998934186 ) ) ;
#47576 = CARTESIAN_POINT ( 'NONE',  ( -22.66983630878679179, -20.09927642381470747, 69.27394370987401828 ) ) ;
#47577 = CONICAL_SURFACE ( 'NONE', #38927, 0.5560000000000009379, 0.06981317007976595157 ) ;
#47578 = CARTESIAN_POINT ( 'NONE',  ( -13.26809664353323726, -20.51382390604332784, 61.66079502706314486 ) ) ;
#47579 = CARTESIAN_POINT ( 'NONE',  ( -13.35534385650551492, -7.417179338643134834, 52.18511593390279302 ) ) ;
#47580 = CIRCLE ( 'NONE', #32636, 2.000000000000001332 ) ;
#47581 = ORIENTED_EDGE ( 'NONE', *, *, #18715, .T. ) ;
#47582 = ORIENTED_EDGE ( 'NONE', *, *, #22100, .F. ) ;
#47583 = EDGE_CURVE ( 'NONE', #28350, #12407, #37949, .T. ) ;
#47584 = CARTESIAN_POINT ( 'NONE',  ( -22.70923626323604694, -10.21920355281058157, 66.82716892541095888 ) ) ;
#47585 = FACE_OUTER_BOUND ( 'NONE', #20856, .T. ) ;
#47586 = VERTEX_POINT ( 'NONE', #16015 ) ;
#47587 = CARTESIAN_POINT ( 'NONE',  ( -22.10255287824656989, -12.42708119714673742, 50.77966884056655772 ) ) ;
#47589 = CARTESIAN_POINT ( 'NONE',  ( -13.22466687598806523, -9.790356633151166221, 49.88233999786937289 ) ) ;
#47588 = CARTESIAN_POINT ( 'NONE',  ( -13.49409790474204840, -20.66256726344224504, 61.53118467422925164 ) ) ;
#47590 = CARTESIAN_POINT ( 'NONE',  ( -13.12535629923256941, -9.217633289312832545, 71.26414145609075490 ) ) ;
#47591 = CARTESIAN_POINT ( 'NONE',  ( -18.81159385541304019, -8.990409506049205746, 49.61344411288074951 ) ) ;
#47592 = EDGE_CURVE ( 'NONE', #9250, #38102, #41900, .T. ) ;
#47593 = CARTESIAN_POINT ( 'NONE',  ( -12.00744322407076226, -19.92521668911118482, 61.58333889064303435 ) ) ;
#47594 = VERTEX_POINT ( 'NONE', #31059 ) ;
#47595 = FACE_BOUND ( 'NONE', #18730, .T. ) ;
#47596 = CARTESIAN_POINT ( 'NONE',  ( -46.47622156840087371, -14.20920654474410760, 70.13000000000000966 ) ) ;
#47597 = CARTESIAN_POINT ( 'NONE',  ( -10.42366005825797792, -14.81678892838547767, 75.08162374473462819 ) ) ;
#47598 = ADVANCED_FACE ( 'NONE', ( #30589 ), #45613, .F. ) ;
#47599 = CARTESIAN_POINT ( 'NONE',  ( -13.52486571068042487, -17.40907233461224735, 49.52966884056655772 ) ) ;
#47600 = EDGE_LOOP ( 'NONE', ( #36879, #8011 ) ) ;
#47601 = DIRECTION ( 'NONE',  ( -0.4007314504464637439, 0.1985303619678204790, 0.8944271909999157444 ) ) ;
#47602 = CARTESIAN_POINT ( 'NONE',  ( -21.79284385541302527, -8.630756214087140776, 51.74842643355251681 ) ) ;
#47603 = EDGE_CURVE ( 'NONE', #5915, #10474, #38573, .T. ) ;
#47604 = CARTESIAN_POINT ( 'NONE',  ( -13.33887460415658133, -9.124795780406598666, 63.90946578472572526 ) ) ;
#47605 = CARTESIAN_POINT ( 'NONE',  ( -18.69178539469224987, -19.32099559247695097, 49.52966884056656482 ) ) ;
#47606 = ADVANCED_FACE ( 'NONE', ( #38428 ), #38683, .T. ) ;
#47607 = CARTESIAN_POINT ( 'NONE',  ( -11.05034076241727625, -11.79557573020262318, 71.37388789199357575 ) ) ;
#47608 = ORIENTED_EDGE ( 'NONE', *, *, #4430, .F. ) ;
#47609 = ORIENTED_EDGE ( 'NONE', *, *, #20845, .F. ) ;
#47610 = CARTESIAN_POINT ( 'NONE',  ( -17.40534385541304374, -7.595227055684746986, 51.75156210489594599 ) ) ;
#47611 = CARTESIAN_POINT ( 'NONE',  ( -10.83536383905390998, -17.31742040078651357, 64.62739380450889826 ) ) ;
#47612 = CARTESIAN_POINT ( 'NONE',  ( -24.03078312051908227, -17.12275678261753953, 69.64013211569611883 ) ) ;
#47613 = ADVANCED_FACE ( 'NONE', ( #26890 ), #33759, .T. ) ;
#47614 = AXIS2_PLACEMENT_3D ( 'NONE', #18444, #37393, #40610 ) ;
#47615 = DIRECTION ( 'NONE',  ( 1.000000000000000000, 2.866981220435666553E-17, 0.000000000000000000 ) ) ;
#47616 = CARTESIAN_POINT ( 'NONE',  ( -16.02453559203015132, -22.12732798260191913, 58.47240968810538675 ) ) ;
#47617 = ORIENTED_EDGE ( 'NONE', *, *, #19176, .F. ) ;
#47618 = CARTESIAN_POINT ( 'NONE',  ( -14.28913879486226435, -8.050816564744696535, 67.37479651646088996 ) ) ;
#47619 = CARTESIAN_POINT ( 'NONE',  ( -23.19916440516392697, -19.59445054535707698, 54.27966884056655061 ) ) ;
#47620 = VERTEX_POINT ( 'NONE', #34494 ) ;
#47621 = CARTESIAN_POINT ( 'NONE',  ( -18.98390459359973548, -7.933620001262258192, 66.91543923465640376 ) ) ;
#47622 = EDGE_CURVE ( 'NONE', #3842, #27657, #36021, .T. ) ;
#47623 = CARTESIAN_POINT ( 'NONE',  ( -18.53748367693119192, -21.77439179387026869, 69.02334521062161343 ) ) ;
#47624 = VERTEX_POINT ( 'NONE', #45845 ) ;
#47625 = DIRECTION ( 'NONE',  ( 0.000000000000000000, 0.000000000000000000, 1.000000000000000000 ) ) ;
#47626 = CARTESIAN_POINT ( 'NONE',  ( -23.83043773139749533, -11.86620498678314561, 59.78235732590890450 ) ) ;
#47627 = ORIENTED_EDGE ( 'NONE', *, *, #27493, .T. ) ;
#47628 = CARTESIAN_POINT ( 'NONE',  ( -10.93244803288776090, -12.03909807633519513, 71.24428013274216198 ) ) ;
#47629 = FACE_OUTER_BOUND ( 'NONE', #45354, .T. ) ;
#47630 = CARTESIAN_POINT ( 'NONE',  ( -24.41553149706675896, -15.71832598455623398, 69.81835354388927328 ) ) ;
#47631 = CARTESIAN_POINT ( 'NONE',  ( -22.22619359738691003, -20.50513629785891823, 58.94938195453792673 ) ) ;
#47632 = ORIENTED_EDGE ( 'NONE', *, *, #20338, .F. ) ;
#47633 = CARTESIAN_POINT ( 'NONE',  ( -13.17588093101833557, -17.89387621085224822, 50.77966884056655772 ) ) ;
#47634 = EDGE_CURVE ( 'NONE', #9616, #26173, #44433, .T. ) ;
#47635 = DIRECTION ( 'NONE',  ( 1.000000000000000000, -4.164305804376849172E-17, 1.614929280266638808E-16 ) ) ;
#47636 = B_SPLINE_CURVE_WITH_KNOTS ( 'NONE', 3,
 ( #12033, #15703, #23356, #4637, #30991, #4170, #19172, #26315, #8585, #37624 ),
 .UNSPECIFIED., .F., .F.,
 ( 4, 2, 2, 2, 4 ),
 ( 0.6272669072877713470, 0.7522669073072923984, 0.8772669073268133388, 1.002266907346334390, 1.127266907365855442 ),
 .UNSPECIFIED. ) ;
#47637 = CARTESIAN_POINT ( 'NONE',  ( -17.42409385541305511, -14.80920654474411080, 47.99999999999997868 ) ) ;
#47638 = CARTESIAN_POINT ( 'NONE',  ( -22.86159385650551457, -9.295667164867525756, 49.30633214617472504 ) ) ;
#47639 = CARTESIAN_POINT ( 'NONE',  ( -16.71219989829967645, -22.22520177033091926, 68.81065352759269160 ) ) ;
#47640 = FACE_OUTER_BOUND ( 'NONE', #46780, .T. ) ;
#47641 = ORIENTED_EDGE ( 'NONE', *, *, #16105, .F. ) ;
#47642 = CARTESIAN_POINT ( 'NONE',  ( -45.37196614242555626, -14.20920654474410760, 70.87000000000000455 ) ) ;
#47643 = CARTESIAN_POINT ( 'NONE',  ( -14.29546348963859437, -8.047845817433223914, 67.43787819521311633 ) ) ;
#47644 = CARTESIAN_POINT ( 'NONE',  ( -13.41327670018355001, -20.54622194888242603, 58.34650078082590596 ) ) ;
#47645 = EDGE_LOOP ( 'NONE', ( #33309, #44158 ) ) ;
#47646 = EDGE_CURVE ( 'NONE', #14265, #30719, #6227, .T. ) ;
#47647 = ORIENTED_EDGE ( 'NONE', *, *, #40411, .F. ) ;
#47648 = ORIENTED_EDGE ( 'NONE', *, *, #44305, .T. ) ;
#47649 = ORIENTED_EDGE ( 'NONE', *, *, #11237, .T. ) ;
#47650 = EDGE_CURVE ( 'NONE', #4523, #4476, #1507, .T. ) ;
#47651 = CARTESIAN_POINT ( 'NONE',  ( -23.75246069176763442, -11.81711528745043971, 59.49738212070109711 ) ) ;
#47652 = CARTESIAN_POINT ( 'NONE',  ( -23.04367457972577427, -10.55211693511195215, 59.75203429192391269 ) ) ;
#47653 = CARTESIAN_POINT ( 'NONE',  ( -13.22576123393696967, -9.135673809461350103, 70.99358371225501685 ) ) ;
#47654 = VERTEX_POINT ( 'NONE', #1980 ) ;
#47655 = ORIENTED_EDGE ( 'NONE', *, *, #15039, .F. ) ;
#47656 = CARTESIAN_POINT ( 'NONE',  ( -20.08034385650552167, -6.424090610841176385, 49.80797279389977916 ) ) ;
#47657 = CARTESIAN_POINT ( 'NONE',  ( -27.42409385541305156, -15.80920654474410725, 47.99999999999997868 ) ) ;
#47658 = CARTESIAN_POINT ( 'NONE',  ( -10.84060798775485246, -17.18797739218483400, 61.17245566960979630 ) ) ;
#47660 = EDGE_CURVE ( 'NONE', #39323, #24815, #17847, .T. ) ;
#47659 = CARTESIAN_POINT ( 'NONE',  ( -17.15534385650551741, -7.417179338643134834, 52.18511593390279302 ) ) ;
#47661 = EDGE_CURVE ( 'NONE', #19851, #29482, #20209, .T. ) ;
#47662 = ORIENTED_EDGE ( 'NONE', *, *, #36235, .T. ) ;
#47663 = EDGE_CURVE ( 'NONE', #21219, #26756, #25569, .T. ) ;
#47664 = EDGE_CURVE ( 'NONE', #40988, #3865, #12547, .T. ) ;
#47665 = DIRECTION ( 'NONE',  ( -3.413470714839332458E-33, 1.190614954331866791E-16, -1.000000000000000000 ) ) ;
#47666 = CARTESIAN_POINT ( 'NONE',  ( -24.41553149706675896, -15.71832598455623398, 69.81835354388927328 ) ) ;
#47667 = ORIENTED_EDGE ( 'NONE', *, *, #20252, .T. ) ;
#47668 = CARTESIAN_POINT ( 'NONE',  ( -27.42409385541305511, -27.10920654474410796, 78.99999999999998579 ) ) ;
#47669 = VECTOR ( 'NONE', #38092, 1000.000000000000000 ) ;
#47670 = AXIS2_PLACEMENT_3D ( 'NONE', #22110, #37102, #10054 ) ;
#47671 = ORIENTED_EDGE ( 'NONE', *, *, #17309, .F. ) ;
#47672 = DIRECTION ( 'NONE',  ( 0.000000000000000000, 0.000000000000000000, 1.000000000000000000 ) ) ;
#47673 = CARTESIAN_POINT ( 'NONE',  ( -21.36489679027069499, -8.963475500412677377, 73.60128753237400190 ) ) ;
#47674 = CARTESIAN_POINT ( 'NONE',  ( -22.38767768884900988, -19.81996202295057330, 65.58933089874275879 ) ) ;
#47675 = ORIENTED_EDGE ( 'NONE', *, *, #1037, .F. ) ;
#47676 = CARTESIAN_POINT ( 'NONE',  ( -19.44222556512714917, -7.637678758653525968, 60.21738930846358073 ) ) ;
#47677 = CARTESIAN_POINT ( 'NONE',  ( -17.12409385541300111, -9.359200813967566646, 50.49621490985766314 ) ) ;
#47678 = CARTESIAN_POINT ( 'NONE',  ( -21.03177576320737785, -20.86624375009474974, 65.88453921249779910 ) ) ;
#47679 = ORIENTED_EDGE ( 'NONE', *, *, #26674, .F. ) ;
#47680 = DIRECTION ( 'NONE',  ( 0.5351595679979626041, 0.8447509909909748371, 0.000000000000000000 ) ) ;
#47681 = FACE_OUTER_BOUND ( 'NONE', #28149, .T. ) ;
#47682 = ORIENTED_EDGE ( 'NONE', *, *, #12386, .T. ) ;
#47683 = DIRECTION ( 'NONE',  ( 0.9687793358424819923, -0.2479245821708680464, 0.000000000000000000 ) ) ;
#47684 = VERTEX_POINT ( 'NONE', #38923 ) ;
#47685 = CARTESIAN_POINT ( 'NONE',  ( -13.20291541311068961, -8.670452210032964402, 60.53926637877078321 ) ) ;
#47687 = EDGE_CURVE ( 'NONE', #5074, #8993, #15554, .T. ) ;
#47686 = PLANE ( 'NONE',  #21604 ) ;
#47688 = DIRECTION ( 'NONE',  ( 0.000000000000000000, -0.9999954153791273948, -0.003028072113819838245 ) ) ;
#47689 = CARTESIAN_POINT ( 'NONE',  ( -23.19948571119275726, -18.85291137746750323, 65.83861571032234394 ) ) ;
#47690 = ORIENTED_EDGE ( 'NONE', *, *, #44679, .F. ) ;
#47691 = CARTESIAN_POINT ( 'NONE',  ( -12.73887154267113253, -15.16169402761810048, 49.52966884056655772 ) ) ;
#47692 = CARTESIAN_POINT ( 'NONE',  ( -14.78766009005058635, -21.34800739930362568, 58.45145834864037937 ) ) ;
#47693 =( BOUNDED_CURVE ( )  B_SPLINE_CURVE ( 3, ( #44022, #9793, #14402, #24807 ),
 .UNSPECIFIED., .F., .F. ) 
 B_SPLINE_CURVE_WITH_KNOTS ( ( 4, 4 ),
 ( 0.4074455897393646220, 0.5000000000000000000 ),
 .UNSPECIFIED. ) 
 CURVE ( )  GEOMETRIC_REPRESENTATION_ITEM ( )  RATIONAL_B_SPLINE_CURVE ( ( 0.6983129098260960621, 0.7760317562607046415, 0.8765941196520070644, 1.000000000000005995 ) ) 
 REPRESENTATION_ITEM ( '' )  );
#47694 = LINE ( 'NONE', #28743, #13299 ) ;
#47695 = VERTEX_POINT ( 'NONE', #47041 ) ;
#47696 = CARTESIAN_POINT ( 'NONE',  ( -11.22571687057108036, -18.94262312776799106, 64.90740396756440589 ) ) ;
#47697 = CARTESIAN_POINT ( 'NONE',  ( -24.68398957063837074, -13.13362340124566785, 63.01919566578877152 ) ) ;
#47698 = ORIENTED_EDGE ( 'NONE', *, *, #38080, .F. ) ;
#47699 = ORIENTED_EDGE ( 'NONE', *, *, #3831, .T. ) ;
#47700 = CARTESIAN_POINT ( 'NONE',  ( -15.69736356130078647, -8.025520047610617880, 70.90989840317035942 ) ) ;
#47701 = CARTESIAN_POINT ( 'NONE',  ( -16.47989802999360265, -19.41181990985090877, 49.52966884056656482 ) ) ;
#47702 = CARTESIAN_POINT ( 'NONE',  ( -10.53536195276627829, -13.30851587854854579, 74.69289754060230280 ) ) ;
#47703 = CARTESIAN_POINT ( 'NONE',  ( -24.80769062643263467, -15.80232089486973557, 69.71802876059763321 ) ) ;
#47704 = DIRECTION ( 'NONE',  ( 0.9687793358424821033, -0.2479245821708677133, 0.000000000000000000 ) ) ;
#47705 = CARTESIAN_POINT ( 'NONE',  ( -12.49855684652675514, -19.85736664535339813, 68.75146050727752822 ) ) ;
#47706 = CARTESIAN_POINT ( 'NONE',  ( -17.80019921555161844, -7.368697419278031902, 60.28049549549236019 ) ) ;
#47707 =( BOUNDED_CURVE ( )  B_SPLINE_CURVE ( 3, ( #31005, #42087, #15962, #7884 ),
 .UNSPECIFIED., .F., .F. ) 
 B_SPLINE_CURVE_WITH_KNOTS ( ( 4, 4 ),
 ( 0.000000000000000000, 0.4074455897393600701 ),
 .UNSPECIFIED. ) 
 CURVE ( )  GEOMETRIC_REPRESENTATION_ITEM ( )  RATIONAL_B_SPLINE_CURVE ( ( 1.000000000000000000, 0.4567392136813371861, 0.3561768502900322653, 0.6983129098260852929 ) ) 
 REPRESENTATION_ITEM ( '' )  );
#47708 = AXIS2_PLACEMENT_3D ( 'NONE', #11548, #4402, #30770 ) ;
#47709 = AXIS2_PLACEMENT_3D ( 'NONE', #43563, #12781, #31980 ) ;
#47710 = ORIENTED_EDGE ( 'NONE', *, *, #2661, .F. ) ;
#47711 = ORIENTED_EDGE ( 'NONE', *, *, #32710, .T. ) ;
#47712 = DIRECTION ( 'NONE',  ( 0.000000000000000000, 0.000000000000000000, 1.000000000000000000 ) ) ;
#47713 = CARTESIAN_POINT ( 'NONE',  ( -23.06976681795876161, -9.947994002224390897, 66.70215612779006165 ) ) ;
#47714 = FACE_OUTER_BOUND ( 'NONE', #13695, .T. ) ;
#47715 = CARTESIAN_POINT ( 'NONE',  ( -17.42409385541299471, -14.80920654474435594, 52.02966884056656482 ) ) ;
#47716 = CIRCLE ( 'NONE', #26486, 1.999999999999999556 ) ;
#47717 = CARTESIAN_POINT ( 'NONE',  ( -11.05952341788191617, -11.89506116984398609, 71.27964083260611972 ) ) ;
#47718 = CARTESIAN_POINT ( 'NONE',  ( -18.75534385650551528, -7.417179338643134834, 52.18511593390279302 ) ) ;
#47719 = ORIENTED_EDGE ( 'NONE', *, *, #47687, .T. ) ;
#47720 = EDGE_CURVE ( 'NONE', #27190, #23362, #22607, .T. ) ;
#47721 = EDGE_CURVE ( 'NONE', #23748, #38000, #31542, .T. ) ;
#47722 = CARTESIAN_POINT ( 'NONE',  ( -21.95894734753736088, -20.14334337125395180, 62.46269013518474367 ) ) ;
#47723 = LINE ( 'NONE', #39851, #37885 ) ;
#47724 = CARTESIAN_POINT ( 'NONE',  ( -16.94712425470457973, -14.65920654474411045, 47.99999999999998579 ) ) ;
#47725 = CARTESIAN_POINT ( 'NONE',  ( -18.13032352084594478, -22.22571048536470428, 65.45258006234271875 ) ) ;
#47726 = ORIENTED_EDGE ( 'NONE', *, *, #37842, .T. ) ;
#47727 = EDGE_CURVE ( 'NONE', #45804, #16655, #20943, .T. ) ;
#47728 = EDGE_CURVE ( 'NONE', #11393, #24008, #13531, .T. ) ;
#47729 = CARTESIAN_POINT ( 'NONE',  ( -13.99854101903132531, -20.98015058628177698, 65.14195714266269022 ) ) ;
#47730 = CARTESIAN_POINT ( 'NONE',  ( -12.73044152958719977, -14.59664269629646682, 49.52966884056655772 ) ) ;
#47731 = CYLINDRICAL_SURFACE ( 'NONE', #32987, 0.1499999999999971079 ) ;
#47732 = ORIENTED_EDGE ( 'NONE', *, *, #1987, .T. ) ;
#47733 = CARTESIAN_POINT ( 'NONE',  ( -22.96484172783137012, -19.08706962207428504, 58.88410642316259214 ) ) ;
#47734 = VECTOR ( 'NONE', #9024, 999.9999999999998863 ) ;
#47735 = AXIS2_PLACEMENT_3D ( 'NONE', #20840, #46470, #27976 ) ;
#47736 = ORIENTED_EDGE ( 'NONE', *, *, #13537, .F. ) ;
#47737 = DIRECTION ( 'NONE',  ( -0.9687793358424819923, 0.2479245821708680464, 0.000000000000000000 ) ) ;
#47738 = CARTESIAN_POINT ( 'NONE',  ( -10.23389218427744218, -12.85876097310435640, 67.93170662612612887 ) ) ;
#47739 = ORIENTED_EDGE ( 'NONE', *, *, #4316, .F. ) ;
#47740 = FACE_OUTER_BOUND ( 'NONE', #12646, .T. ) ;
#47741 = EDGE_CURVE ( 'NONE', #27084, #36955, #24878, .T. ) ;
#47742 = CARTESIAN_POINT ( 'NONE',  ( -12.56171917241870695, -20.45376946399996854, 71.99148991968543498 ) ) ;
#47743 = ORIENTED_EDGE ( 'NONE', *, *, #24534, .F. ) ;
#47744 = DIRECTION ( 'NONE',  ( -2.866981220435666553E-17, 1.000000000000000000, 1.190614954331866791E-16 ) ) ;
#47745 = VECTOR ( 'NONE', #17795, 1000.000000000000114 ) ;
#47746 = DIRECTION ( 'NONE',  ( -0.9687793358424819923, 0.2479245821708680464, 0.000000000000000000 ) ) ;
#47747 = CARTESIAN_POINT ( 'NONE',  ( -21.61101410369608899, -8.646988051702825473, 73.79467079059151047 ) ) ;
#47748 = ORIENTED_EDGE ( 'NONE', *, *, #30544, .F. ) ;
#47749 = B_SPLINE_CURVE_WITH_KNOTS ( 'NONE', 3,
 ( #4932, #30794, #12066, #15979, #11828, #986, #12540, #26851, #19444, #45574 ),
 .UNSPECIFIED., .F., .F.,
 ( 4, 2, 2, 2, 4 ),
 ( 0.000000000000000000, 0.2500000000000000000, 0.5000000000000000000, 0.7500000000000000000, 1.000000000000000000 ),
 .UNSPECIFIED. ) ;
#47750 = CARTESIAN_POINT ( 'NONE',  ( -13.49406902941962372, -21.13830689255522088, 65.18640088419860490 ) ) ;
#47751 = CARTESIAN_POINT ( 'NONE',  ( -16.09337498760136853, -22.13948385882417824, 58.40090183616962349 ) ) ;
#47752 = CARTESIAN_POINT ( 'NONE',  ( -12.05483428091225129, -10.31798718066989551, 67.49896870046983111 ) ) ;
#47753 = DIRECTION ( 'NONE',  ( 1.000000000000000000, 0.000000000000000000, 0.000000000000000000 ) ) ;
#47754 = VERTEX_POINT ( 'NONE', #16251 ) ;
#47755 = VERTEX_POINT ( 'NONE', #6645 ) ;
#47756 = FACE_OUTER_BOUND ( 'NONE', #24873, .T. ) ;
#47757 = CARTESIAN_POINT ( 'NONE',  ( -24.34586551078590233, -16.16342498662110572, 59.00843562520186936 ) ) ;
#47758 = ORIENTED_EDGE ( 'NONE', *, *, #12010, .T. ) ;
#47759 = CARTESIAN_POINT ( 'NONE',  ( -20.76602563802732604, -8.150687638125187817, 63.43404616943938379 ) ) ;
#47760 = CARTESIAN_POINT ( 'NONE',  ( -14.00534385759799427, -7.595227055684746986, 51.75156210489594599 ) ) ;
#47761 = CARTESIAN_POINT ( 'NONE',  ( -24.72409385541305582, -14.90920654474413709, 60.01764705882352047 ) ) ;
#47762 = CARTESIAN_POINT ( 'NONE',  ( -14.23443154292173674, -21.09974595518388440, 71.81118900415394535 ) ) ;
#47763 = CARTESIAN_POINT ( 'NONE',  ( -20.57913387270943417, -8.060128879191506002, 66.95916824008536139 ) ) ;
#47764 = CARTESIAN_POINT ( 'NONE',  ( -16.49028911930641428, -22.20062183403187106, 65.36531050670200216 ) ) ;
#47765 = ORIENTED_EDGE ( 'NONE', *, *, #21616, .F. ) ;
#47766 = DIRECTION ( 'NONE',  ( -9.941263206155103325E-06, -7.040377910290660294E-06, 0.9999999999258021299 ) ) ;
#47767 = CARTESIAN_POINT ( 'NONE',  ( -4.424093855413053333, -25.10920654474410441, 63.99999999999998579 ) ) ;
#47768 = CARTESIAN_POINT ( 'NONE',  ( -10.81855813007775957, -11.36397971161496301, 67.71890362106785233 ) ) ;
#47769 = AXIS2_PLACEMENT_3D ( 'NONE', #42525, #15911, #35109 ) ;
#47770 = ORIENTED_EDGE ( 'NONE', *, *, #36623, .T. ) ;
#47771 = CIRCLE ( 'NONE', #9231, 2.000000000000000444 ) ;
#47772 = VERTEX_POINT ( 'NONE', #18433 ) ;
#47773 = EDGE_CURVE ( 'NONE', #1012, #25345, #22157, .T. ) ;
#47774 = CARTESIAN_POINT ( 'NONE',  ( -20.63397896388913821, -8.588477125147733204, 59.85627665378241602 ) ) ;
#47775 = CARTESIAN_POINT ( 'NONE',  ( -17.81243367693841151, -24.25303685828974665, 53.49999999999995026 ) ) ;
#47776 = CARTESIAN_POINT ( 'NONE',  ( -23.88825063663133363, -11.10528180765545869, 70.06927628447702716 ) ) ;
#47777 =( BOUNDED_SURFACE ( )  B_SPLINE_SURFACE ( 3, 1, ( 
 ( #10654, #33268 ),
 ( #37209, #29605 ),
 ( #25430, #17774 ),
 ( #36487, #10889 ),
 ( #6714, #18761 ),
 ( #25911, #40926 ),
 ( #3006, #61 ) ),
 .UNSPECIFIED., .T., .F., .F. ) 
 B_SPLINE_SURFACE_WITH_KNOTS ( ( 4, 3, 4 ),
 ( 2, 2 ),
 ( 0.000000000000000000, 0.5000000000000000000, 1.000000000000000000 ),
 ( 0.000000000000000000, 1.000000000000000000 ),
 .UNSPECIFIED. ) 
 GEOMETRIC_REPRESENTATION_ITEM ( )  RATIONAL_B_SPLINE_SURFACE ( (
 ( 1.000000000000000000, 1.000000000000000000),
 ( 0.3333333333333335369, 0.3333333333333330373),
 ( 0.3333333333333335369, 0.3333333333333330373),
 ( 1.000000000000000000, 1.000000000000000000),
 ( 0.3333333333333333703, 0.3333333333333333703),
 ( 0.3333333333333333703, 0.3333333333333333703),
 ( 1.000000000000000000, 1.000000000000000000) ) ) 
 REPRESENTATION_ITEM ( '' )  SURFACE ( )  );
#47778 = VECTOR ( 'NONE', #3654, 1000.000000000000227 ) ;
#47779 = ORIENTED_EDGE ( 'NONE', *, *, #48308, .T. ) ;
#47780 = AXIS2_PLACEMENT_3D ( 'NONE', #13994, #18429, #7387 ) ;
#47781 = CARTESIAN_POINT ( 'NONE',  ( -24.24936666102675531, -13.25469412794844537, 59.64802506593036924 ) ) ;
#47782 = ADVANCED_FACE ( 'NONE', ( #43848 ), #14377, .T. ) ;
#47783 = CARTESIAN_POINT ( 'NONE',  ( -22.02798021202036693, -12.28596846334092163, 49.52966884056655772 ) ) ;
#47784 = ORIENTED_EDGE ( 'NONE', *, *, #24293, .T. ) ;
#47785 = ADVANCED_FACE ( 'NONE', ( #10101 ), #36124, .T. ) ;
#47786 = CARTESIAN_POINT ( 'NONE',  ( -14.84927081153347039, -21.37251255130113137, 61.65072491673618771 ) ) ;
#47787 = CARTESIAN_POINT ( 'NONE',  ( -24.87123163304818974, -14.59964195235338735, 62.89791815715346956 ) ) ;
#47788 = EDGE_CURVE ( 'NONE', #21704, #24396, #47042, .T. ) ;
#47789 = CARTESIAN_POINT ( 'NONE',  ( -23.34288328645119037, -19.33377384263253873, 59.06905932422779415 ) ) ;
#47790 = VERTEX_POINT ( 'NONE', #48238 ) ;
#47791 = CARTESIAN_POINT ( 'NONE',  ( -24.12942727696282219, -12.79922002830157268, 69.77243032624397756 ) ) ;
#47792 = VERTEX_POINT ( 'NONE', #47761 ) ;
#47793 = CARTESIAN_POINT ( 'NONE',  ( -15.87557486115802696, -7.931373420853706335, 67.44007279014866185 ) ) ;
#47794 = DIRECTION ( 'NONE',  ( -0.9441784275685841665, 0.3294345108122634369, 1.993146885055994800E-08 ) ) ;
#47795 = VERTEX_POINT ( 'NONE', #25124 ) ;
#47796 = CARTESIAN_POINT ( 'NONE',  ( -21.42927658580616068, -21.09115185931090508, 69.17637394757619518 ) ) ;
#47797 = CARTESIAN_POINT ( 'NONE',  ( -10.76763551407085373, -17.13171859787639661, 61.45743118825841833 ) ) ;
#47798 = DIRECTION ( 'NONE',  ( 0.8839923186919886877, -0.4675014229855999348, 2.842058574697910628E-08 ) ) ;
#47799 = AXIS2_PLACEMENT_3D ( 'NONE', #40889, #44851, #36452 ) ;
#47800 = CARTESIAN_POINT ( 'NONE',  ( -13.33852097861372421, -12.48893720396535301, 52.02966884056656482 ) ) ;
#47801 = CARTESIAN_POINT ( 'NONE',  ( -14.23827708255551627, -10.77544123782542229, 52.02966884056656482 ) ) ;
#47802 = DIRECTION ( 'NONE',  ( -3.071710424422018668E-17, 6.404604876783312462E-16, 1.000000000000000000 ) ) ;
#47803 = VERTEX_POINT ( 'NONE', #44561 ) ;
#47804 = LINE ( 'NONE', #13807, #1881 ) ;
#47805 = AXIS2_PLACEMENT_3D ( 'NONE', #18358, #41029, #29699 ) ;
#47806 = VECTOR ( 'NONE', #17127, 1000.000000000000000 ) ;
#47807 = FACE_OUTER_BOUND ( 'NONE', #46247, .T. ) ;
#47808 = CYLINDRICAL_SURFACE ( 'NONE', #20412, 2.000000000000001332 ) ;
#47809 = CARTESIAN_POINT ( 'NONE',  ( -13.18474066807476675, -20.93551553819402855, 58.23145462665691241 ) ) ;
#47810 = B_SPLINE_CURVE_WITH_KNOTS ( 'NONE', 3,
 ( #37056, #40515, #11225, #36558, #18848, #154, #15134, #3089, #18584, #7297 ),
 .UNSPECIFIED., .F., .F.,
 ( 4, 2, 2, 2, 4 ),
 ( 0.1272669073659000727, 0.2522669073463680856, 0.3772669073268360984, 0.5022669073073040558, 0.6272669072877721241 ),
 .UNSPECIFIED. ) ;
#47811 = CARTESIAN_POINT ( 'NONE',  ( -43.06159385541306506, -14.80920654474410547, 57.89999999999999147 ) ) ;
#47812 = CARTESIAN_POINT ( 'NONE',  ( -24.26647757246398740, -16.29234447064223446, 62.66499050339684374 ) ) ;
#47813 = EDGE_LOOP ( 'NONE', ( #24327, #6853, #13848, #22101, #9631 ) ) ;
#47814 = ORIENTED_EDGE ( 'NONE', *, *, #35041, .T. ) ;
#47815 = CARTESIAN_POINT ( 'NONE',  ( -16.06904454444675778, -7.890656075740461795, 63.67011029959335389 ) ) ;
#47816 = CARTESIAN_POINT ( 'NONE',  ( -21.86481658501223535, -9.328930240182819134, 66.75330195800948729 ) ) ;
#47817 = ORIENTED_EDGE ( 'NONE', *, *, #4620, .T. ) ;
#47819 = LINE ( 'NONE', #14056, #23433 ) ;
#47818 = FACE_OUTER_BOUND ( 'NONE', #10085, .T. ) ;
#47820 = CARTESIAN_POINT ( 'NONE',  ( -24.18314773428282649, -12.98801661480574410, 66.60246782464800219 ) ) ;
#47821 = AXIS2_PLACEMENT_3D ( 'NONE', #39215, #1543, #47094 ) ;
#47822 = CARTESIAN_POINT ( 'NONE',  ( -13.69310769661218252, -20.79108007429942617, 64.98628911427817911 ) ) ;
#47823 = VERTEX_POINT ( 'NONE', #40143 ) ;
#47824 = CARTESIAN_POINT ( 'NONE',  ( -42.92262326717776943, -14.80920654474412679, 59.01176470588234224 ) ) ;
#47825 = VECTOR ( 'NONE', #10757, 1000.000000000000114 ) ;
#47826 = CARTESIAN_POINT ( 'NONE',  ( -23.85820687874296908, -17.57049056139491583, 66.13284205629301482 ) ) ;
#47827 = CARTESIAN_POINT ( 'NONE',  ( -14.35043204381087101, -18.34698626059704551, 52.02966884056656482 ) ) ;
#47828 = FACE_OUTER_BOUND ( 'NONE', #13542, .T. ) ;
#47829 = ORIENTED_EDGE ( 'NONE', *, *, #20609, .T. ) ;
#47830 = DIRECTION ( 'NONE',  ( -3.071710424422018668E-17, 6.404604876783312462E-16, 1.000000000000000000 ) ) ;
#47831 = CARTESIAN_POINT ( 'NONE',  ( -11.60896167836250292, -10.15203476212633227, 71.10859753193520305 ) ) ;
#47832 = CARTESIAN_POINT ( 'NONE',  ( -17.89428206796744192, -21.84713016422586307, 65.43712271095169797 ) ) ;
#47833 = CARTESIAN_POINT ( 'NONE',  ( -50.42609385541305755, -14.80920654474424225, 70.97647058823527288 ) ) ;
#47834 =( BOUNDED_CURVE ( )  B_SPLINE_CURVE ( 3, ( #20577, #10217, #46907, #47156 ),
 .UNSPECIFIED., .F., .F. ) 
 B_SPLINE_CURVE_WITH_KNOTS ( ( 4, 4 ),
 ( 0.4074455897393638448, 0.5000000000000000000 ),
 .UNSPECIFIED. ) 
 CURVE ( )  GEOMETRIC_REPRESENTATION_ITEM ( )  RATIONAL_B_SPLINE_CURVE ( ( 0.6983129098260915102, 0.7760317562606922071, 0.8765941196519938527, 0.9999999999999927836 ) ) 
 REPRESENTATION_ITEM ( '' )  );
#47835 = EDGE_CURVE ( 'NONE', #48249, #3376, #47154, .T. ) ;
#47836 = DIRECTION ( 'NONE',  ( -3.071710424422018668E-17, 6.404604876783312462E-16, 1.000000000000000000 ) ) ;
#47837 = CARTESIAN_POINT ( 'NONE',  ( -19.90648311238531676, -10.83415612659008964, 52.02966884056656482 ) ) ;
#47838 = EDGE_LOOP ( 'NONE', ( #45003, #43265, #2912, #24996 ) ) ;
#47839 = ORIENTED_EDGE ( 'NONE', *, *, #40108, .F. ) ;
#47840 = CARTESIAN_POINT ( 'NONE',  ( -16.67409385541304445, -6.859212275519751323, 50.50378509014259265 ) ) ;
#47841 = ORIENTED_EDGE ( 'NONE', *, *, #41004, .T. ) ;
#47842 = CARTESIAN_POINT ( 'NONE',  ( -15.58034385759799001, -9.360768649639298999, 51.01397948905923130 ) ) ;
#47843 = CIRCLE ( 'NONE', #38373, 0.5000000000000004441 ) ;
#47844 = CARTESIAN_POINT ( 'NONE',  ( -19.10873388551254948, -7.551407109436953924, 67.08727174327995613 ) ) ;
#47845 = VECTOR ( 'NONE', #37453, 1000.000000000000114 ) ;
#47846 =( BOUNDED_SURFACE ( )  B_SPLINE_SURFACE ( 3, 1, ( 
 ( #15349, #16082 ),
 ( #12167, #598 ),
 ( #38246, #19066 ),
 ( #12649, #23989 ),
 ( #42707, #8969 ),
 ( #23759, #847 ),
 ( #15848, #30893 ) ),
 .UNSPECIFIED., .T., .F., .F. ) 
 B_SPLINE_SURFACE_WITH_KNOTS ( ( 4, 3, 4 ),
 ( 2, 2 ),
 ( 0.000000000000000000, 0.5000000000000000000, 1.000000000000000000 ),
 ( 0.000000000000000000, 1.000000000000000000 ),
 .UNSPECIFIED. ) 
 GEOMETRIC_REPRESENTATION_ITEM ( )  RATIONAL_B_SPLINE_SURFACE ( (
 ( 1.000000000000000000, 1.000000000000000000),
 ( 0.3333333333333335369, 0.3333333333333330373),
 ( 0.3333333333333335369, 0.3333333333333330373),
 ( 1.000000000000000000, 1.000000000000000000),
 ( 0.3333333333333333703, 0.3333333333333333703),
 ( 0.3333333333333333703, 0.3333333333333333703),
 ( 1.000000000000000000, 1.000000000000000000) ) ) 
 REPRESENTATION_ITEM ( '' )  SURFACE ( )  );
#47847 = VECTOR ( 'NONE', #19116, 1000.000000000000000 ) ;
#47848 = AXIS2_PLACEMENT_3D ( 'NONE', #40779, #45465, #22314 ) ;
#47849 = CARTESIAN_POINT ( 'NONE',  ( -20.13659385759799036, -8.995762431863214559, 51.38120296130585274 ) ) ;
#47850 = CARTESIAN_POINT ( 'NONE',  ( -15.53779737384271442, -7.601787063750024664, 70.77023165166117735 ) ) ;
#47851 = ORIENTED_EDGE ( 'NONE', *, *, #6876, .F. ) ;
#47852 = ADVANCED_FACE ( 'NONE', ( #6408 ), #6887, .F. ) ;
#47853 = LINE ( 'NONE', #47384, #10315 ) ;
#47854 = VECTOR ( 'NONE', #45655, 1000.000000000000000 ) ;
#47855 = CARTESIAN_POINT ( 'NONE',  ( -14.83720200468841810, -10.88702015217558206, 49.52966884056655772 ) ) ;
#47856 = EDGE_CURVE ( 'NONE', #42866, #10114, #44348, .T. ) ;
#47857 = ORIENTED_EDGE ( 'NONE', *, *, #42731, .T. ) ;
#47858 = LINE ( 'NONE', #48580, #15699 ) ;
#47859 =( BOUNDED_SURFACE ( )  B_SPLINE_SURFACE ( 3, 1, ( 
 ( #11703, #45447 ),
 ( #26732, #41750 ),
 ( #8038, #48387 ),
 ( #23044, #3576 ),
 ( #38032, #4323 ),
 ( #14623, #11224 ),
 ( #42482, #41991 ) ),
 .UNSPECIFIED., .T., .F., .F. ) 
 B_SPLINE_SURFACE_WITH_KNOTS ( ( 4, 3, 4 ),
 ( 2, 2 ),
 ( 0.000000000000000000, 0.5000000000000000000, 1.000000000000000000 ),
 ( 0.000000000000000000, 1.000000000000000000 ),
 .UNSPECIFIED. ) 
 GEOMETRIC_REPRESENTATION_ITEM ( )  RATIONAL_B_SPLINE_SURFACE ( (
 ( 1.000000000000000000, 1.000000000000000000),
 ( 0.3333333333333335369, 0.3333333333333330373),
 ( 0.3333333333333335369, 0.3333333333333330373),
 ( 1.000000000000000000, 1.000000000000000000),
 ( 0.3333333333333333703, 0.3333333333333333703),
 ( 0.3333333333333333703, 0.3333333333333333703),
 ( 1.000000000000000000, 1.000000000000000000) ) ) 
 REPRESENTATION_ITEM ( '' )  SURFACE ( )  );
#47860 = ORIENTED_EDGE ( 'NONE', *, *, #9424, .F. ) ;
#47861 = ADVANCED_FACE ( 'NONE', ( #36903 ), #18195, .F. ) ;
#47862 = CARTESIAN_POINT ( 'NONE',  ( -19.57699507595987143, -21.94144279212693860, 62.17998934563075153 ) ) ;
#47863 = CARTESIAN_POINT ( 'NONE',  ( -21.46381135070672386, -20.59674881067212127, 69.21017043924877044 ) ) ;
#47864 = DIRECTION ( 'NONE',  ( -3.071710424422018668E-17, 6.404604876783312462E-16, 1.000000000000000000 ) ) ;
#47865 = ORIENTED_EDGE ( 'NONE', *, *, #3052, .T. ) ;
#47866 = DIRECTION ( 'NONE',  ( 0.9687793358424821033, -0.2479245821708679909, 0.000000000000000000 ) ) ;
#47867 = FACE_OUTER_BOUND ( 'NONE', #43279, .T. ) ;
#47868 = EDGE_CURVE ( 'NONE', #33919, #26226, #24215, .T. ) ;
#47869 = CARTESIAN_POINT ( 'NONE',  ( -21.47456293661849713, -9.038556783377254433, 70.41660404402310292 ) ) ;
#47870 = LINE ( 'NONE', #33300, #12716 ) ;
#47871 = VERTEX_POINT ( 'NONE', #481 ) ;
#47872 = DIRECTION ( 'NONE',  ( 0.9687793358424819923, -0.2479245821708680464, 0.000000000000000000 ) ) ;
#47873 = CARTESIAN_POINT ( 'NONE',  ( -16.91478550490786859, -21.84108428878278119, 72.18015306840750611 ) ) ;
#47874 = CARTESIAN_POINT ( 'NONE',  ( -12.48216758013336936, -16.58117287899024817, 49.52966884056655772 ) ) ;
#47875 = CARTESIAN_POINT ( 'NONE',  ( -11.38784684563249527, -10.44144024994987774, 74.55229573521346254 ) ) ;
#47876 = AXIS2_PLACEMENT_3D ( 'NONE', #37426, #10144, #40899 ) ;
#47877 = CARTESIAN_POINT ( 'NONE',  ( -11.75774095458083046, -19.00383931511212765, 71.68685884783835149 ) ) ;
#47878 = DIRECTION ( 'NONE',  ( 0.9687793358424821033, -0.2479245821708677133, 0.000000000000000000 ) ) ;
#47879 = VERTEX_POINT ( 'NONE', #19423 ) ;
#47880 = CARTESIAN_POINT ( 'NONE',  ( -13.84722314507279961, -8.273888791401406095, 74.37671575878690078 ) ) ;
#47881 =( GEOMETRIC_REPRESENTATION_CONTEXT ( 3 ) GLOBAL_UNCERTAINTY_ASSIGNED_CONTEXT ( ( #28260 ) ) GLOBAL_UNIT_ASSIGNED_CONTEXT ( ( #8127, #34931, #4412 ) ) REPRESENTATION_CONTEXT ( 'NONE', 'WORKASPACE' ) );
#47882 = CARTESIAN_POINT ( 'NONE',  ( 10.57590614458695377, -0.1092432217106413528, 50.52422457691089619 ) ) ;
#47883 = CARTESIAN_POINT ( 'NONE',  ( -18.32882331211134286, -7.814473174497912566, 73.72575526123169709 ) ) ;
#47884 = VERTEX_POINT ( 'NONE', #963 ) ;
#47885 = DIRECTION ( 'NONE',  ( -3.534154189880001717E-15, 4.519331686442879103E-31, 1.000000000000000000 ) ) ;
#47886 = AXIS2_PLACEMENT_3D ( 'NONE', #42889, #16038, #38454 ) ;
#47887 = ORIENTED_EDGE ( 'NONE', *, *, #21135, .T. ) ;
#47888 = B_SPLINE_CURVE_WITH_KNOTS ( 'NONE', 3,
 ( #34256, #1255, #16260, #15537, #38437, #26900, #30597, #4728, #19750, #34505 ),
 .UNSPECIFIED., .F., .F.,
 ( 4, 2, 2, 2, 4 ),
 ( 0.000000000000000000, 0.2500000000000000000, 0.5000000000000000000, 0.7500000000000000000, 1.000000000000000000 ),
 .UNSPECIFIED. ) ;
#47889 = EDGE_LOOP ( 'NONE', ( #23676, #17179, #44520, #30456, #11800 ) ) ;
#47890 = ORIENTED_EDGE ( 'NONE', *, *, #46983, .F. ) ;
#47891 = B_SPLINE_CURVE_WITH_KNOTS ( 'NONE', 3,
 ( #23186, #19473, #1240, #30826, #46322, #18998, #15518, #22955, #16246, #23680 ),
 .UNSPECIFIED., .F., .F.,
 ( 4, 2, 2, 2, 4 ),
 ( 0.1272669073658369288, 0.2522669073488094105, 0.3772669073317819199, 0.5022669073147543184, 0.6272669072977268279 ),
 .UNSPECIFIED. ) ;
#47892 = FACE_OUTER_BOUND ( 'NONE', #43131, .T. ) ;
#47893 = VECTOR ( 'NONE', #35628, 1000.000000000000114 ) ;
#47894 = CARTESIAN_POINT ( 'NONE',  ( -14.30826163110301685, -8.540783165273367672, 70.72957638424304605 ) ) ;
#47895 = EDGE_CURVE ( 'NONE', #28162, #15877, #21336, .T. ) ;
#47896 = DIRECTION ( 'NONE',  ( 0.7621627669932626858, -0.6473854467078885566, 3.680865982637999709E-08 ) ) ;
#47897 = CARTESIAN_POINT ( 'NONE',  ( -45.92409385541306222, -17.80920654474411435, 71.75000000000001421 ) ) ;
#47898 = EDGE_LOOP ( 'NONE', ( #48129, #20919 ) ) ;
#47899 = ORIENTED_EDGE ( 'NONE', *, *, #20716, .T. ) ;
#47900 = CARTESIAN_POINT ( 'NONE',  ( -19.68659385650551386, -9.302874398569244363, 51.68646062012417985 ) ) ;
#47901 = PLANE ( 'NONE',  #30756 ) ;
#47902 = CARTESIAN_POINT ( 'NONE',  ( -19.06784385650551528, -6.428312510596451368, 51.20221977374900035 ) ) ;
#47903 = B_SPLINE_CURVE_WITH_KNOTS ( 'NONE', 3,
 ( #26330, #46023, #30285, #45306, #37639, #23369, #33687, #15466, #38128, #12043 ),
 .UNSPECIFIED., .F., .F.,
 ( 4, 2, 2, 2, 4 ),
 ( 0.000000000000000000, 0.2500000000000000000, 0.5000000000000000000, 0.7500000000000000000, 1.000000000000000000 ),
 .UNSPECIFIED. ) ;
#47904 = B_SPLINE_CURVE_WITH_KNOTS ( 'NONE', 3,
 ( #44697, #33084, #22519, #18825, #44950, #14365, #29419, #44451, #15113, #10954 ),
 .UNSPECIFIED., .F., .F.,
 ( 4, 2, 2, 2, 4 ),
 ( 0.1272669073658505845, 0.2522669073463317257, 0.3772669073268128948, 0.5022669073072940638, 0.6272669072877752328 ),
 .UNSPECIFIED. ) ;
#47905 = ADVANCED_FACE ( 'NONE', ( #30043 ), #32946, .T. ) ;
#47906 = ORIENTED_EDGE ( 'NONE', *, *, #48116, .F. ) ;
#47907 = DIRECTION ( 'NONE',  ( -3.549360974554993999E-17, 6.371834667797928663E-18, 1.000000000000000000 ) ) ;
#47908 = EDGE_CURVE ( 'NONE', #30479, #41134, #15226, .T. ) ;
#47909 = CIRCLE ( 'NONE', #36883, 2.000000000000000444 ) ;
#47910 = FACE_OUTER_BOUND ( 'NONE', #47111, .T. ) ;
#47911 = ORIENTED_EDGE ( 'NONE', *, *, #17378, .T. ) ;
#47912 = CARTESIAN_POINT ( 'NONE',  ( -11.28069628694023940, -11.45046166655791886, 67.72937716582121936 ) ) ;
#47913 = AXIS2_PLACEMENT_3D ( 'NONE', #35635, #31716, #43039 ) ;
#47914 = CIRCLE ( 'NONE', #14075, 4.686499999999998778 ) ;
#47915 = VERTEX_POINT ( 'NONE', #721 ) ;
#47916 = EDGE_CURVE ( 'NONE', #45931, #36781, #47903, .T. ) ;
#47917 = DIRECTION ( 'NONE',  ( -0.9789991564299000970, -0.2038642972899922245, 4.410747590293501912E-08 ) ) ;
#47918 = FACE_OUTER_BOUND ( 'NONE', #8102, .T. ) ;
#47919 = CARTESIAN_POINT ( 'NONE',  ( -10.40417500068134160, -12.31441648348895868, 57.43519039097821377 ) ) ;
#47920 = ORIENTED_EDGE ( 'NONE', *, *, #18667, .T. ) ;
#47921 = CIRCLE ( 'NONE', #21989, 2.000000000000000888 ) ;
#47922 = DIRECTION ( 'NONE',  ( 1.198821491151391801E-05, -1.588017923178218046E-05, 0.9999999998020513425 ) ) ;
#47923 = ADVANCED_FACE ( 'NONE', ( #11553 ), #39304, .T. ) ;
#47924 = DIRECTION ( 'NONE',  ( 0.000000000000000000, 0.000000000000000000, 1.000000000000000000 ) ) ;
#47925 = CARTESIAN_POINT ( 'NONE',  ( -22.29619887594318328, -17.36118473213641167, 53.49899999999994549 ) ) ;
#47926 = ORIENTED_EDGE ( 'NONE', *, *, #46494, .T. ) ;
#47927 = DIRECTION ( 'NONE',  ( -2.866981220435666553E-17, 1.000000000000000000, 1.190614954331866791E-16 ) ) ;
#47928 = CARTESIAN_POINT ( 'NONE',  ( -10.42431062902801386, -14.74026950914408829, 71.62782695461453386 ) ) ;
#47929 = CARTESIAN_POINT ( 'NONE',  ( -18.83428564917659287, -7.493810079819247072, 70.62713979963420741 ) ) ;
#47930 = ORIENTED_EDGE ( 'NONE', *, *, #13193, .F. ) ;
#47931 = CARTESIAN_POINT ( 'NONE',  ( -11.81178692268928643, -10.62566621335946770, 74.43885052268630886 ) ) ;
#47932 = ORIENTED_EDGE ( 'NONE', *, *, #33907, .T. ) ;
#47933 = CARTESIAN_POINT ( 'NONE',  ( -10.80730693270912468, -17.26544268483686650, 57.84327589213576459 ) ) ;
#47934 = CARTESIAN_POINT ( 'NONE',  ( -13.61031878520947913, -20.67920105661088215, 61.51646270097772629 ) ) ;
#47935 = DIRECTION ( 'NONE',  ( 1.674255585786183705E-21, -0.9999746924698832418, -0.007114381193220357599 ) ) ;
#47936 = CARTESIAN_POINT ( 'NONE',  ( -14.60479643987598841, -7.913168514039711887, 60.50491717424539218 ) ) ;
#47937 = ORIENTED_EDGE ( 'NONE', *, *, #48211, .F. ) ;
#47938 = DIRECTION ( 'NONE',  ( -3.071710424422018668E-17, 6.404604876783312462E-16, 1.000000000000000000 ) ) ;
#47939 = CARTESIAN_POINT ( 'NONE',  ( -23.85748962928175132, -11.92509172808648543, 59.49707787073156595 ) ) ;
#47941 = EDGE_CURVE ( 'NONE', #47436, #28192, #26829, .T. ) ;
#47940 = DIRECTION ( 'NONE',  ( -0.1240347345892086200, 1.145860353393066553E-16, -0.9922778767136676281 ) ) ;
#47942 = VERTEX_POINT ( 'NONE', #33720 ) ;
#47943 = CARTESIAN_POINT ( 'NONE',  ( -10.38360249164154325, -14.43747963625415487, 67.87272197508832505 ) ) ;
#47944 = EDGE_CURVE ( 'NONE', #32426, #15477, #34190, .T. ) ;
#47945 = EDGE_CURVE ( 'NONE', #28201, #29749, #27660, .T. ) ;
#47946 = ORIENTED_EDGE ( 'NONE', *, *, #20799, .F. ) ;
#47947 = ORIENTED_EDGE ( 'NONE', *, *, #13142, .F. ) ;
#47948 = CARTESIAN_POINT ( 'NONE',  ( -35.32409385541306079, -6.359206544744109735, 48.79999999999998295 ) ) ;
#47950 = LINE ( 'NONE', #9573, #23359 ) ;
#47949 = VECTOR ( 'NONE', #10317, 1000.000000000000000 ) ;
#47951 = CARTESIAN_POINT ( 'NONE',  ( -11.56806251476610115, -18.73522173559940995, 65.03234934376791898 ) ) ;
#47952 = CARTESIAN_POINT ( 'NONE',  ( -23.96159466281891071, -11.23502865522796768, 70.07866094266108803 ) ) ;
#47953 = CARTESIAN_POINT ( 'NONE',  ( -23.34299683607928699, -18.64475395501998278, 73.17857113406003577 ) ) ;
#47954 = CARTESIAN_POINT ( 'NONE',  ( -13.03190793544029091, -9.358637495099101145, 67.57045887702402354 ) ) ;
#47955 = VECTOR ( 'NONE', #30661, 1000.000000000000000 ) ;
#47956 = ORIENTED_EDGE ( 'NONE', *, *, #12735, .T. ) ;
#47957 = EDGE_LOOP ( 'NONE', ( #44900, #9842, #24079, #47649 ) ) ;
#47958 = CARTESIAN_POINT ( 'NONE',  ( -24.35026726019748011, -16.14395875459130281, 59.33152169323236791 ) ) ;
#47959 = CARTESIAN_POINT ( 'NONE',  ( -21.55460084640030161, -9.091360965714955000, 73.90129052096925477 ) ) ;
#47960 = DIRECTION ( 'NONE',  ( 4.556087729312554466E-06, -5.696494005668992306E-06, 0.9999999999733959477 ) ) ;
#47961 = CIRCLE ( 'NONE', #47191, 0.7499999999999998890 ) ;
#47962 = PLANE ( 'NONE',  #28799 ) ;
#47963 = CARTESIAN_POINT ( 'NONE',  ( -24.43113031232903865, -15.58634216689856977, 73.30303748141028564 ) ) ;
#47964 = EDGE_LOOP ( 'NONE', ( #11478, #17880, #15164, #17487 ) ) ;
#47965 = CARTESIAN_POINT ( 'NONE',  ( -18.41784385650552736, -9.790100578890868377, 49.79778022625163203 ) ) ;
#47966 = VERTEX_POINT ( 'NONE', #24097 ) ;
#47967 = DIRECTION ( 'NONE',  ( 8.719004453613161891E-07, -8.513143893533137515E-07, 0.9999999999992574828 ) ) ;
#47968 = CYLINDRICAL_SURFACE ( 'NONE', #26086, 0.1500000000000037970 ) ;
#47969 = VECTOR ( 'NONE', #41583, 1000.000000000000000 ) ;
#47970 = CARTESIAN_POINT ( 'NONE',  ( -21.98892968875003717, -15.92178434430670642, 49.52966884056655772 ) ) ;
#47971 = CARTESIAN_POINT ( 'NONE',  ( -10.41569439578338496, -15.57669382292980131, 61.05261153187079515 ) ) ;
#47972 = VERTEX_POINT ( 'NONE', #31727 ) ;
#47973 = EDGE_CURVE ( 'NONE', #38441, #22495, #8596, .T. ) ;
#47974 = CARTESIAN_POINT ( 'NONE',  ( -27.42409385541305511, -27.10920654474410796, 81.99999999999998579 ) ) ;
#47975 = CARTESIAN_POINT ( 'NONE',  ( -17.42409385541299471, -14.80920654474435771, 49.52966884056655772 ) ) ;
#47976 = DIRECTION ( 'NONE',  ( -1.000000000000000000, -1.669677910507523057E-21, -6.493791346278465266E-22 ) ) ;
#47977 = AXIS2_PLACEMENT_3D ( 'NONE', #20974, #43143, #13795 ) ;
#47978 = B_SPLINE_CURVE_WITH_KNOTS ( 'NONE', 1,
 ( #12202, #16612 ),
 .UNSPECIFIED., .F., .F.,
 ( 2, 2 ),
 ( 0.000000000000000000, 1.000000000000000000 ),
 .UNSPECIFIED. ) ;
#47979 =( BOUNDED_SURFACE ( )  B_SPLINE_SURFACE ( 3, 1, ( 
 ( #23729, #43149 ),
 ( #9423, #12619 ),
 ( #24447, #16784 ),
 ( #9180, #38720 ),
 ( #5005, #20015 ),
 ( #24196, #31580 ),
 ( #35018, #1283 ) ),
 .UNSPECIFIED., .T., .F., .F. ) 
 B_SPLINE_SURFACE_WITH_KNOTS ( ( 4, 3, 4 ),
 ( 2, 2 ),
 ( 0.000000000000000000, 0.5000000000000000000, 1.000000000000000000 ),
 ( 0.000000000000000000, 1.000000000000000000 ),
 .UNSPECIFIED. ) 
 GEOMETRIC_REPRESENTATION_ITEM ( )  RATIONAL_B_SPLINE_SURFACE ( (
 ( 1.000000000000000000, 1.000000000000000000),
 ( 0.3333333333333335369, 0.3333333333333330373),
 ( 0.3333333333333335369, 0.3333333333333330373),
 ( 1.000000000000000000, 1.000000000000000000),
 ( 0.3333333333333333703, 0.3333333333333333703),
 ( 0.3333333333333333703, 0.3333333333333333703),
 ( 1.000000000000000000, 1.000000000000000000) ) ) 
 REPRESENTATION_ITEM ( '' )  SURFACE ( )  );
#47980 = CARTESIAN_POINT ( 'NONE',  ( -24.10584592916820057, -12.56049825913868823, 73.24225570139947195 ) ) ;
#47981 = VERTEX_POINT ( 'NONE', #35409 ) ;
#47982 = DIRECTION ( 'NONE',  ( -0.9687793358424819923, 0.2479245821708680464, 0.000000000000000000 ) ) ;
#47983 = VECTOR ( 'NONE', #39701, 1000.000000000000000 ) ;
#47984 = EDGE_LOOP ( 'NONE', ( #13007, #21297, #27744, #9550, #22370 ) ) ;
#47985 = DIRECTION ( 'NONE',  ( 3.071710424422018668E-17, -6.404604876783312462E-16, -1.000000000000000000 ) ) ;
#47986 = CARTESIAN_POINT ( 'NONE',  ( -11.57425499491753307, -18.65360305739656610, 64.74707076836355668 ) ) ;
#47987 = ORIENTED_EDGE ( 'NONE', *, *, #14006, .T. ) ;
#47988 = CARTESIAN_POINT ( 'NONE',  ( -22.37985683132060188, -19.82347751554591397, 69.47417989525710880 ) ) ;
#47989 = CARTESIAN_POINT ( 'NONE',  ( -11.64902330566212463, -10.02396254413167753, 47.99999999999994316 ) ) ;
#47990 = ORIENTED_EDGE ( 'NONE', *, *, #39003, .F. ) ;
#47991 = CARTESIAN_POINT ( 'NONE',  ( -22.14090652532222236, -20.04928072148792495, 62.51967078134249078 ) ) ;
#47992 = CARTESIAN_POINT ( 'NONE',  ( -19.55442184481404766, -21.52995072282663358, 65.47958309245051112 ) ) ;
#47993 = CARTESIAN_POINT ( 'NONE',  ( -24.86363034504136138, -14.41430157806603773, 66.28269108591972270 ) ) ;
#47994 = ORIENTED_EDGE ( 'NONE', *, *, #44583, .T. ) ;
#47995 = PLANE ( 'NONE',  #25494 ) ;
#47996 =( BOUNDED_SURFACE ( )  B_SPLINE_SURFACE ( 3, 1, ( 
 ( #5558, #20574 ),
 ( #35570, #16846 ),
 ( #31885, #46902 ),
 ( #19462, #33735 ),
 ( #27096, #285 ),
 ( #30327, #15017 ),
 ( #30080, #42122 ) ),
 .UNSPECIFIED., .T., .F., .F. ) 
 B_SPLINE_SURFACE_WITH_KNOTS ( ( 4, 3, 4 ),
 ( 2, 2 ),
 ( 0.000000000000000000, 0.5000000000000000000, 1.000000000000000000 ),
 ( 0.000000000000000000, 1.000000000000000000 ),
 .UNSPECIFIED. ) 
 GEOMETRIC_REPRESENTATION_ITEM ( )  RATIONAL_B_SPLINE_SURFACE ( (
 ( 1.000000000000000000, 1.000000000000000000),
 ( 0.3333333333333335369, 0.3333333333333330373),
 ( 0.3333333333333335369, 0.3333333333333330373),
 ( 1.000000000000000000, 1.000000000000000000),
 ( 0.3333333333333333703, 0.3333333333333333703),
 ( 0.3333333333333333703, 0.3333333333333333703),
 ( 1.000000000000000000, 1.000000000000000000) ) ) 
 REPRESENTATION_ITEM ( '' )  SURFACE ( )  );
#47997 = EDGE_CURVE ( 'NONE', #15944, #22030, #27782, .T. ) ;
#47998 = CARTESIAN_POINT ( 'NONE',  ( -11.38014877795855995, -11.27757159305587464, 60.97885732570401274 ) ) ;
#47999 = FACE_OUTER_BOUND ( 'NONE', #6156, .T. ) ;
#48000 = EDGE_CURVE ( 'NONE', #27537, #1629, #1187, .T. ) ;
#48001 = EDGE_CURVE ( 'NONE', #31485, #16726, #17160, .T. ) ;
#48002 = ORIENTED_EDGE ( 'NONE', *, *, #39529, .F. ) ;
#48003 = VERTEX_POINT ( 'NONE', #20407 ) ;
#48004 = LINE ( 'NONE', #32957, #29049 ) ;
#48005 = CARTESIAN_POINT ( 'NONE',  ( -16.96573618372038794, -7.824106395124359459, 73.96018256200346741 ) ) ;
#48006 = CARTESIAN_POINT ( 'NONE',  ( -20.70192761744073806, -8.118982583651908058, 63.50395666093379532 ) ) ;
#48007 = CARTESIAN_POINT ( 'NONE',  ( -13.44284385759799605, -7.587656875400194068, 49.25157356644813689 ) ) ;
#48008 = CARTESIAN_POINT ( 'NONE',  ( -23.21283114448125673, -10.11939864774917908, 63.25681283445349123 ) ) ;
#48009 = CARTESIAN_POINT ( 'NONE',  ( -16.82990565096947577, -21.78406541307506217, 68.69560622315208320 ) ) ;
#48010 = DIRECTION ( 'NONE',  ( -3.071710424422018668E-17, 6.404604876783312462E-16, 1.000000000000000000 ) ) ;
#48011 = DIRECTION ( 'NONE',  ( -3.395770065602591412E-06, -1.105252671792169116E-06, 0.9999999999936236561 ) ) ;
#48012 = ORIENTED_EDGE ( 'NONE', *, *, #33783, .F. ) ;
#48013 = DIRECTION ( 'NONE',  ( 2.200805972648249745E-07, 3.006001593475220059E-06, 0.9999999999954577445 ) ) ;
#48014 = CARTESIAN_POINT ( 'NONE',  ( -14.04013919049901560, -8.171999524408169790, 70.77311711151845941 ) ) ;
#48015 = VECTOR ( 'NONE', #33358, 1000.000000000000000 ) ;
#48016 = DIRECTION ( 'NONE',  ( -0.7107718805962432995, -0.7034225854731134264, -7.722840056494081040E-09 ) ) ;
#48017 = FACE_OUTER_BOUND ( 'NONE', #2818, .T. ) ;
#48018 = ORIENTED_EDGE ( 'NONE', *, *, #47262, .F. ) ;
#48019 = ORIENTED_EDGE ( 'NONE', *, *, #14215, .T. ) ;
#48020 = ADVANCED_FACE ( 'NONE', ( #9085 ), #28272, .T. ) ;
#48021 = CARTESIAN_POINT ( 'NONE',  ( -17.00739772171234776, -7.370819460300548798, 74.15356576969422520 ) ) ;
#48022 = CARTESIAN_POINT ( 'NONE',  ( -19.61601346313181082, -21.50980264518277707, 65.46486213821819433 ) ) ;
#48023 = CARTESIAN_POINT ( 'NONE',  ( -23.29918339618657086, -19.39037464299967439, 58.99915238703562181 ) ) ;
#48024 = CARTESIAN_POINT ( 'NONE',  ( -11.55820670847359821, -18.73429759261662397, 71.83119032172525920 ) ) ;
#48025 = AXIS2_PLACEMENT_3D ( 'NONE', #24054, #20105, #5338 ) ;
#48026 = EDGE_LOOP ( 'NONE', ( #39210, #47524, #6006, #31243, #26995 ) ) ;
#48027 = FACE_OUTER_BOUND ( 'NONE', #35478, .T. ) ;
#48028 = CARTESIAN_POINT ( 'NONE',  ( -13.82689732469268407, -20.87277619789260186, 68.47097268802275494 ) ) ;
#48029 = ORIENTED_EDGE ( 'NONE', *, *, #11497, .F. ) ;
#48030 = CARTESIAN_POINT ( 'NONE',  ( -22.38400238879419391, -20.36826089713532895, 62.41934470639706944 ) ) ;
#48031 = CARTESIAN_POINT ( 'NONE',  ( -24.87286266620955288, -14.66952948351439190, 62.96942391020206742 ) ) ;
#48032 = CARTESIAN_POINT ( 'NONE',  ( -22.79947183316497217, -19.38307604245925475, 59.02843669344121480 ) ) ;
#48033 = VERTEX_POINT ( 'NONE', #1189 ) ;
#48034 = DIRECTION ( 'NONE',  ( 1.000000000000000000, 2.866981220435666553E-17, 0.000000000000000000 ) ) ;
#48035 = VERTEX_POINT ( 'NONE', #20884 ) ;
#48036 = CARTESIAN_POINT ( 'NONE',  ( -10.49862800246030936, -15.82799116930659622, 64.50771590054291948 ) ) ;
#48038 = PLANE ( 'NONE',  #47799 ) ;
#48037 = AXIS2_PLACEMENT_3D ( 'NONE', #41065, #7345, #7585 ) ;
#48039 = VERTEX_POINT ( 'NONE', #2160 ) ;
#48040 = DIRECTION ( 'NONE',  ( -0.000000000000000000, 1.000000000000000000, -0.000000000000000000 ) ) ;
#48041 = CARTESIAN_POINT ( 'NONE',  ( -24.12651600458584511, -12.62191667979047160, 73.25697658996381278 ) ) ;
#48042 = LINE ( 'NONE', #21226, #2189 ) ;
#48043 = CARTESIAN_POINT ( 'NONE',  ( -14.41059836940365635, -8.490934564906170934, 67.25975084671087245 ) ) ;
#48044 = CARTESIAN_POINT ( 'NONE',  ( -10.04821600842096174, -15.85811274820897410, 64.62276192103250594 ) ) ;
#48045 = FACE_OUTER_BOUND ( 'NONE', #33043, .T. ) ;
#48046 = LINE ( 'NONE', #29336, #6186 ) ;
#48047 = ORIENTED_EDGE ( 'NONE', *, *, #13151, .F. ) ;
#48048 = AXIS2_PLACEMENT_3D ( 'NONE', #33059, #21034, #13625 ) ;
#48049 = CARTESIAN_POINT ( 'NONE',  ( -9.972618654632643853, -13.80886736810690962, 54.02312124697527906 ) ) ;
#48050 = CARTESIAN_POINT ( 'NONE',  ( -24.09792875595538320, -17.08130417324981920, 72.88336032035921619 ) ) ;
#48051 = CARTESIAN_POINT ( 'NONE',  ( -19.86520892150080897, -18.82374422416847182, 52.02966884056656482 ) ) ;
#48052 = CARTESIAN_POINT ( 'NONE',  ( -13.19046691777508329, -20.93951881724979813, 58.16837286248604499 ) ) ;
#48053 = CARTESIAN_POINT ( 'NONE',  ( -10.77303304197945621, -12.62668734528506853, 61.09853568451838868 ) ) ;
#48054 = CARTESIAN_POINT ( 'NONE',  ( -14.36784385650551599, -6.428312510596451368, 51.20221977374900035 ) ) ;
#48055 = EDGE_CURVE ( 'NONE', #5540, #1406, #38475, .T. ) ;
#48056 = ORIENTED_EDGE ( 'NONE', *, *, #44651, .F. ) ;
#48057 = EDGE_LOOP ( 'NONE', ( #37620, #45008 ) ) ;
#48058 = CARTESIAN_POINT ( 'NONE',  ( -11.46028008028683942, -18.56947564720590194, 61.56238700194530367 ) ) ;
#48059 = CARTESIAN_POINT ( 'NONE',  ( -9.975583804105555785, -14.65598652642324673, 71.44287259100559595 ) ) ;
#48060 = ORIENTED_EDGE ( 'NONE', *, *, #12273, .F. ) ;
#48062 = CARTESIAN_POINT ( 'NONE',  ( -17.42409385541299471, -14.80920654474435594, 52.02966884056656482 ) ) ;
#48061 = CARTESIAN_POINT ( 'NONE',  ( -12.96596438542217555, -9.347743257243967818, 70.99925352873879092 ) ) ;
#48063 = AXIS2_PLACEMENT_3D ( 'NONE', #1450, #15976, #1707 ) ;
#48064 = DIRECTION ( 'NONE',  ( 0.000000000000000000, -0.9999954153791273948, -0.003028072113819838245 ) ) ;
#48065 = CARTESIAN_POINT ( 'NONE',  ( -12.47631340003800915, -9.857337130378009959, 57.08935527210383754 ) ) ;
#48066 = CARTESIAN_POINT ( 'NONE',  ( -14.41791765924166135, -21.19496194411871315, 58.31050579099508724 ) ) ;
#48067 = CARTESIAN_POINT ( 'NONE',  ( -22.23733845922741637, -19.96043711175405733, 66.00421731380804147 ) ) ;
#48068 = CARTESIAN_POINT ( 'NONE',  ( -24.66730449611544529, -13.06573935865489844, 62.94768786448354092 ) ) ;
#48069 = CARTESIAN_POINT ( 'NONE',  ( -13.02884944951828494, -13.18282747993466764, 52.02966884056656482 ) ) ;
#48070 = EDGE_CURVE ( 'NONE', #47594, #37972, #5662, .T. ) ;
#48071 = EDGE_CURVE ( 'NONE', #39181, #1086, #29237, .T. ) ;
#48072 = CARTESIAN_POINT ( 'NONE',  ( -14.80624636014071172, -8.317144122717282428, 60.61996281969079803 ) ) ;
#48073 = ORIENTED_EDGE ( 'NONE', *, *, #6552, .F. ) ;
#48074 = AXIS2_PLACEMENT_3D ( 'NONE', #25693, #15086, #22753 ) ;
#48075 = CARTESIAN_POINT ( 'NONE',  ( -12.14425528403576493, -10.13739698163135117, 64.02914326607979945 ) ) ;
#48076 = EDGE_CURVE ( 'NONE', #21561, #20725, #23235, .T. ) ;
#48077 = CARTESIAN_POINT ( 'NONE',  ( -16.64476583608805882, -21.82402065185451079, 72.30976097999173646 ) ) ;
#48078 = EDGE_CURVE ( 'NONE', #7144, #40267, #23864, .T. ) ;
#48079 = DIRECTION ( 'NONE',  ( -0.8875028193683940358, -0.4608022847308269609, 4.020963237607658939E-08 ) ) ;
#48080 = DIRECTION ( 'NONE',  ( -1.616182858256118783E-16, -0.003028072113822189229, 0.9999954153791275058 ) ) ;
#48081 = FACE_OUTER_BOUND ( 'NONE', #13832, .T. ) ;
#48082 = CARTESIAN_POINT ( 'NONE',  ( -16.55445462874940077, -21.75508803775454325, 65.52564429725259743 ) ) ;
#48083 = ORIENTED_EDGE ( 'NONE', *, *, #36767, .F. ) ;
#48084 = VERTEX_POINT ( 'NONE', #31480 ) ;
#48085 = CARTESIAN_POINT ( 'NONE',  ( -15.94284385541304161, -7.587656875400192291, 49.25157356644813689 ) ) ;
#48086 = VECTOR ( 'NONE', #141, 1000.000000000000000 ) ;
#48087 = ORIENTED_EDGE ( 'NONE', *, *, #18893, .F. ) ;
#48088 = EDGE_CURVE ( 'NONE', #45046, #34652, #17907, .T. ) ;
#48089 = CYLINDRICAL_SURFACE ( 'NONE', #14594, 0.1499999999999962752 ) ;
#48090 = CARTESIAN_POINT ( 'NONE',  ( -17.39761456938454742, -7.809256627251312644, 67.32039592144390383 ) ) ;
#48091 = DIRECTION ( 'NONE',  ( 0.9687793358424821033, -0.2479245821708680464, 0.000000000000000000 ) ) ;
#48092 = CARTESIAN_POINT ( 'NONE',  ( -9.975093131592752016, -14.93635113986534257, 74.98274190467411415 ) ) ;
#48093 = ORIENTED_EDGE ( 'NONE', *, *, #1866, .T. ) ;
#48094 = CARTESIAN_POINT ( 'NONE',  ( -23.09478622540421000, -9.977449189158523524, 66.74171034086974430 ) ) ;
#48095 = CIRCLE ( 'NONE', #8022, 5.249999999999998224 ) ;
#48096 = CARTESIAN_POINT ( 'NONE',  ( -22.91296630721855720, -15.15889098507616950, 53.49899999999994549 ) ) ;
#48097 = ORIENTED_EDGE ( 'NONE', *, *, #45851, .F. ) ;
#48098 = CARTESIAN_POINT ( 'NONE',  ( -15.77151528785019430, -19.20744933288474954, 49.52966884056656482 ) ) ;
#48099 = CARTESIAN_POINT ( 'NONE',  ( -12.35132619472584459, -19.70513314325878795, 61.39678631839771583 ) ) ;
#48100 = ORIENTED_EDGE ( 'NONE', *, *, #45501, .T. ) ;
#48101 = CARTESIAN_POINT ( 'NONE',  ( -10.77962265614084814, -17.18953632050836333, 68.24154640182683806 ) ) ;
#48102 = CARTESIAN_POINT ( 'NONE',  ( -12.74836358285320159, -20.08597126951521261, 71.82125749157572159 ) ) ;
#48103 = CARTESIAN_POINT ( 'NONE',  ( -23.38410522734749009, -10.33907873996118276, 59.71708144416061970 ) ) ;
#48104 = ORIENTED_EDGE ( 'NONE', *, *, #47317, .T. ) ;
#48105 = LINE ( 'NONE', #14336, #20697 ) ;
#48106 = AXIS2_PLACEMENT_3D ( 'NONE', #10143, #22432, #14041 ) ;
#48107 = EDGE_CURVE ( 'NONE', #1105, #26632, #37713, .T. ) ;
#48108 = CARTESIAN_POINT ( 'NONE',  ( -24.69822986944709697, -13.19963441799314197, 59.54763197719577761 ) ) ;
#48109 = PLANE ( 'NONE',  #16643 ) ;
#48110 = ORIENTED_EDGE ( 'NONE', *, *, #6171, .T. ) ;
#48111 = PLANE ( 'NONE',  #8552 ) ;
#48112 = DIRECTION ( 'NONE',  ( -0.8037372918934696520, 0.5949843406508664723, 7.322964617522835370E-08 ) ) ;
#48113 = CARTESIAN_POINT ( 'NONE',  ( -23.62338436797153918, -18.94230004192412409, 69.48027381658378943 ) ) ;
#48114 = AXIS2_PLACEMENT_3D ( 'NONE', #23097, #42042, #46471 ) ;
#48115 = CARTESIAN_POINT ( 'NONE',  ( -22.18659385650551741, -9.302874398569244363, 51.68646062012417985 ) ) ;
#48116 = EDGE_CURVE ( 'NONE', #23907, #5540, #26354, .T. ) ;
#48117 = AXIS2_PLACEMENT_3D ( 'NONE', #24658, #17716, #1757 ) ;
#48118 = CARTESIAN_POINT ( 'NONE',  ( -17.79084088774826000, -7.768752266068899459, 60.08060768310445354 ) ) ;
#48119 = CARTESIAN_POINT ( 'NONE',  ( -24.35831120643470982, -13.52022779156689936, 59.77756816219774549 ) ) ;
#48120 = VERTEX_POINT ( 'NONE', #48185 ) ;
#48121 = CARTESIAN_POINT ( 'NONE',  ( -24.72409385541305582, -14.80920654474422271, 68.96470588235293064 ) ) ;
#48122 = CARTESIAN_POINT ( 'NONE',  ( -15.50784526261009511, -8.076599967007890513, 74.37985659287807039 ) ) ;
#48123 = CARTESIAN_POINT ( 'NONE',  ( -11.71629718011842414, -10.02134023935637686, 67.69908070314710358 ) ) ;
#48124 =( BOUNDED_CURVE ( )  B_SPLINE_CURVE ( 3, ( #3628, #14929, #26045, #29001 ),
 .UNSPECIFIED., .F., .F. ) 
 B_SPLINE_CURVE_WITH_KNOTS ( ( 4, 4 ),
 ( 0.9074455897393621795, 1.000000000000000000 ),
 .UNSPECIFIED. ) 
 CURVE ( )  GEOMETRIC_REPRESENTATION_ITEM ( )  RATIONAL_B_SPLINE_CURVE ( ( 0.6983129098260769663, 0.7760317562606844355, 0.8765941196519920764, 1.000000000000000000 ) ) 
 REPRESENTATION_ITEM ( '' )  );
#48125 = ORIENTED_EDGE ( 'NONE', *, *, #32461, .T. ) ;
#48126 = CARTESIAN_POINT ( 'NONE',  ( -10.04719910712313968, -15.85120016064457360, 64.68584367229796328 ) ) ;
#48127 = VERTEX_POINT ( 'NONE', #47702 ) ;
#48128 = VERTEX_POINT ( 'NONE', #28990 ) ;
#48129 = ORIENTED_EDGE ( 'NONE', *, *, #13860, .T. ) ;
#48130 = ADVANCED_FACE ( 'NONE', ( #29238 ), #29517, .T. ) ;
#48131 = EDGE_CURVE ( 'NONE', #3170, #11147, #14027, .T. ) ;
#48132 = CARTESIAN_POINT ( 'NONE',  ( -23.47900403436495154, -10.35238886157799953, 53.76227901944321275 ) ) ;
#48133 = CARTESIAN_POINT ( 'NONE',  ( -16.03798070992811731, -7.947690103083033364, 63.97010977124031683 ) ) ;
#48134 = CARTESIAN_POINT ( 'NONE',  ( -12.73947787985187574, -9.016276410220392279, 71.10571287364943771 ) ) ;
#48135 =( BOUNDED_SURFACE ( )  B_SPLINE_SURFACE ( 3, 1, ( 
 ( #21180, #20696 ),
 ( #10090, #13522 ),
 ( #36172, #13757 ),
 ( #44089, #25115 ),
 ( #47523, #29041 ),
 ( #40134, #1969 ),
 ( #6638, #36644 ) ),
 .UNSPECIFIED., .T., .F., .F. ) 
 B_SPLINE_SURFACE_WITH_KNOTS ( ( 4, 3, 4 ),
 ( 2, 2 ),
 ( 0.000000000000000000, 0.5000000000000000000, 1.000000000000000000 ),
 ( 0.000000000000000000, 1.000000000000000000 ),
 .UNSPECIFIED. ) 
 GEOMETRIC_REPRESENTATION_ITEM ( )  RATIONAL_B_SPLINE_SURFACE ( (
 ( 1.000000000000000000, 1.000000000000000000),
 ( 0.3333333333333335369, 0.3333333333333330373),
 ( 0.3333333333333335369, 0.3333333333333330373),
 ( 1.000000000000000000, 1.000000000000000000),
 ( 0.3333333333333333703, 0.3333333333333333703),
 ( 0.3333333333333333703, 0.3333333333333333703),
 ( 1.000000000000000000, 1.000000000000000000) ) ) 
 REPRESENTATION_ITEM ( '' )  SURFACE ( )  );
#48136 = VERTEX_POINT ( 'NONE', #44275 ) ;
#48137 = ORIENTED_EDGE ( 'NONE', *, *, #27251, .T. ) ;
#48138 = ADVANCED_FACE ( 'NONE', ( #13941 ), #25309, .T. ) ;
#48139 = CARTESIAN_POINT ( 'NONE',  ( -16.70534385650551457, -8.801233750844183135, 48.81488406609782515 ) ) ;
#48140 = DIRECTION ( 'NONE',  ( 1.927470528863119295E-16, 0.000000000000000000, -1.000000000000000000 ) ) ;
#48141 = CARTESIAN_POINT ( 'NONE',  ( -23.56138519289638822, -11.33989039198723248, 69.89210750373884196 ) ) ;
#48142 = EDGE_CURVE ( 'NONE', #37234, #27864, #6100, .T. ) ;
#48143 = CARTESIAN_POINT ( 'NONE',  ( -18.16784385650552025, -6.428312510596451368, 51.20221977374900035 ) ) ;
#48144 =( BOUNDED_CURVE ( )  B_SPLINE_CURVE ( 3, ( #34381, #3887, #19376, #668 ),
 .UNSPECIFIED., .F., .F. ) 
 B_SPLINE_CURVE_WITH_KNOTS ( ( 4, 4 ),
 ( 1.570796326794896780, 1.780235837034217283 ),
 .UNSPECIFIED. ) 
 CURVE ( )  GEOMETRIC_REPRESENTATION_ITEM ( )  RATIONAL_B_SPLINE_CURVE ( ( 1.000000000000000000, 0.9963479302455154896, 0.9963479302455154896, 1.000000000000000000 ) ) 
 REPRESENTATION_ITEM ( '' )  );
#48145 = ORIENTED_EDGE ( 'NONE', *, *, #40278, .F. ) ;
#48146 = CARTESIAN_POINT ( 'NONE',  ( -24.36731093625853717, -15.69948419576056331, 69.81842082024948581 ) ) ;
#48147 = DIRECTION ( 'NONE',  ( 1.000000000000000000, -6.517531090241554163E-16, 3.534154189880001717E-15 ) ) ;
#48148 = CARTESIAN_POINT ( 'NONE',  ( -23.53718199026597802, -11.39867937719236757, 70.19210781355312179 ) ) ;
#48149 = ORIENTED_EDGE ( 'NONE', *, *, #16823, .F. ) ;
#48150 = CARTESIAN_POINT ( 'NONE',  ( -22.66727079836811853, -10.09628861529951216, 70.16178520457069112 ) ) ;
#48151 = ORIENTED_EDGE ( 'NONE', *, *, #45028, .T. ) ;
#48152 = CARTESIAN_POINT ( 'NONE',  ( -17.42409385541300182, -14.80920654474440745, 53.27966884056655061 ) ) ;
#48153 = PLANE ( 'NONE',  #28123 ) ;
#48154 = FACE_OUTER_BOUND ( 'NONE', #43567, .T. ) ;
#48155 = CARTESIAN_POINT ( 'NONE',  ( -13.56961256462628818, -20.71652534470609908, 58.25469809373281294 ) ) ;
#48156 = ORIENTED_EDGE ( 'NONE', *, *, #34370, .T. ) ;
#48157 = CARTESIAN_POINT ( 'NONE',  ( -14.78576678908972397, -7.841836775542373239, 57.01033387128751428 ) ) ;
#48158 = CARTESIAN_POINT ( 'NONE',  ( -15.31138759918230186, -21.95353881034377963, 72.18542105808592169 ) ) ;
#48159 = EDGE_CURVE ( 'NONE', #39922, #24620, #6590, .T. ) ;
#48160 = LINE ( 'NONE', #10984, #32897 ) ;
#48161 = DIRECTION ( 'NONE',  ( -1.000000000000000000, 0.000000000000000000, 0.000000000000000000 ) ) ;
#48162 = ORIENTED_EDGE ( 'NONE', *, *, #26517, .F. ) ;
#48163 = DIRECTION ( 'NONE',  ( 0.3478314405900309603, 0.9375570856950864451, -9.567072274253696421E-17 ) ) ;
#48164 = CARTESIAN_POINT ( 'NONE',  ( -21.49004948369781687, -9.049640773346018463, 70.42572721234685673 ) ) ;
#48165 = ORIENTED_EDGE ( 'NONE', *, *, #47541, .T. ) ;
#48166 = FACE_BOUND ( 'NONE', #40119, .T. ) ;
#48167 = EDGE_LOOP ( 'NONE', ( #44091, #15950, #29507, #11795 ) ) ;
#48168 = CARTESIAN_POINT ( 'NONE',  ( 18.46573386768564973, 1.644457370994424572, 49.30478444670940519 ) ) ;
#48169 = CARTESIAN_POINT ( 'NONE',  ( -24.90891992605694227, -15.28604896337863472, 47.99999999999994316 ) ) ;
#48170 = CARTESIAN_POINT ( 'NONE',  ( -16.80428239998583351, -12.38725820513820253, 54.27966884056655061 ) ) ;
#48171 = CARTESIAN_POINT ( 'NONE',  ( -21.22463635358858269, -21.21689783003811769, 65.78442715983884170 ) ) ;
#48172 = ORIENTED_EDGE ( 'NONE', *, *, #3137, .T. ) ;
#48173 = CARTESIAN_POINT ( 'NONE',  ( -50.42409385541305511, -14.80920654474410547, 56.99999999999998579 ) ) ;
#48174 = EDGE_LOOP ( 'NONE', ( #40687, #23537 ) ) ;
#48175 = CARTESIAN_POINT ( 'NONE',  ( -24.72409385541305582, -14.90920654474428630, 74.09999999999998010 ) ) ;
#48176 = CARTESIAN_POINT ( 'NONE',  ( -20.89331258220900978, -11.64059849529350643, 52.02966884056656482 ) ) ;
#48177 = ORIENTED_EDGE ( 'NONE', *, *, #46463, .F. ) ;
#48178 = DIRECTION ( 'NONE',  ( 0.9687793358424821033, -0.2479245821708677133, 0.000000000000000000 ) ) ;
#48179 = CARTESIAN_POINT ( 'NONE',  ( -24.72409385541305582, -15.80920654474410725, 65.99999999999998579 ) ) ;
#48180 = ORIENTED_EDGE ( 'NONE', *, *, #31239, .T. ) ;
#48181 = ORIENTED_EDGE ( 'NONE', *, *, #5551, .F. ) ;
#48182 = CARTESIAN_POINT ( 'NONE',  ( -14.05371499411349667, -21.00138273984457982, 72.22607703579409133 ) ) ;
#48183 = ADVANCED_FACE ( 'NONE', ( #21610 ), #17884, .T. ) ;
#48184 = CARTESIAN_POINT ( 'NONE',  ( -13.06884191565359643, -20.85448943349606665, 58.23305466536662323 ) ) ;
#48185 = CARTESIAN_POINT ( 'NONE',  ( -16.80428239998583351, -12.38725820513820253, 53.27966884056655061 ) ) ;
#48186 = EDGE_CURVE ( 'NONE', #25382, #18791, #17176, .T. ) ;
#48187 = CARTESIAN_POINT ( 'NONE',  ( -16.57554779340669882, -22.21081089906203943, 65.41059674993448425 ) ) ;
#48188 = CARTESIAN_POINT ( 'NONE',  ( -23.77395946432122997, -18.70572718374853594, 73.02014183918953449 ) ) ;
#48189 = DIRECTION ( 'NONE',  ( -0.02400335114476204179, 0.9997118780597844534, 1.529429979384368011E-10 ) ) ;
#48190 = CARTESIAN_POINT ( 'NONE',  ( -20.55988796755815073, -8.491641294495202885, 67.19592733635545301 ) ) ;
#48191 = ORIENTED_EDGE ( 'NONE', *, *, #15323, .T. ) ;
#48192 = ORIENTED_EDGE ( 'NONE', *, *, #15673, .T. ) ;
#48193 = EDGE_CURVE ( 'NONE', #15624, #24088, #15524, .T. ) ;
#48194 = DIRECTION ( 'NONE',  ( -3.071710424422018668E-17, 6.404604876783312462E-16, 1.000000000000000000 ) ) ;
#48195 = CARTESIAN_POINT ( 'NONE',  ( -19.91921166743625093, -8.268929485741445262, 73.73599093592051190 ) ) ;
#48196 = CARTESIAN_POINT ( 'NONE',  ( -22.96484330895583881, -19.08706763331013434, 59.18410642315183878 ) ) ;
#48197 = CARTESIAN_POINT ( 'NONE',  ( -18.99339082800039691, -7.526352757794455783, 67.00048145165719404 ) ) ;
#48198 = EDGE_CURVE ( 'NONE', #40354, #34898, #18498, .T. ) ;
#48199 = CARTESIAN_POINT ( 'NONE',  ( -18.56804848150531484, -7.447508036923572661, 73.94726072066615075 ) ) ;
#48200 = ORIENTED_EDGE ( 'NONE', *, *, #8291, .F. ) ;
#48201 = CARTESIAN_POINT ( 'NONE',  ( -19.59909385650551883, -8.114302828567740988, 52.18300498402516041 ) ) ;
#48202 = VERTEX_POINT ( 'NONE', #19127 ) ;
#48203 = CARTESIAN_POINT ( 'NONE',  ( -16.75112815133339694, -21.83074212251240453, 72.46543312350107158 ) ) ;
#48204 = DIRECTION ( 'NONE',  ( -1.616182858256118536E-16, -0.003028072113822188795, 0.9999954153791273948 ) ) ;
#48205 = CARTESIAN_POINT ( 'NONE',  ( -24.46479344177693349, -14.44719919422189491, 66.18292729247950490 ) ) ;
#48206 = DIRECTION ( 'NONE',  ( 0.9687793358424821033, -0.2479245821708678243, 0.000000000000000000 ) ) ;
#48207 = EDGE_CURVE ( 'NONE', #29387, #17516, #29674, .T. ) ;
#48208 = ORIENTED_EDGE ( 'NONE', *, *, #28663, .T. ) ;
#48209 = EDGE_CURVE ( 'NONE', #42340, #7278, #37865, .T. ) ;
#48210 = CARTESIAN_POINT ( 'NONE',  ( -18.85724798917316392, -7.906108138700305155, 67.18599644112759961 ) ) ;
#48211 = EDGE_CURVE ( 'NONE', #10231, #12237, #24365, .T. ) ;
#48212 = CARTESIAN_POINT ( 'NONE',  ( -14.76782893607791891, -8.332635497213580322, 60.31996286260869056 ) ) ;
#48213 = VERTEX_POINT ( 'NONE', #19362 ) ;
#48214 = DIRECTION ( 'NONE',  ( -0.06306825763707681054, 0.9980092158285027715, 2.415158932891090531E-08 ) ) ;
#48215 = CARTESIAN_POINT ( 'NONE',  ( -10.13258936719380898, -16.33817337277914561, 71.63245765104117879 ) ) ;
#48216 = ORIENTED_EDGE ( 'NONE', *, *, #36272, .F. ) ;
#48217 = DIRECTION ( 'NONE',  ( -3.071710424422018668E-17, 6.404604876783312462E-16, 1.000000000000000000 ) ) ;
#48218 = EDGE_LOOP ( 'NONE', ( #43817, #33227, #19471, #5195 ) ) ;
#48219 = CARTESIAN_POINT ( 'NONE',  ( -28.42409385541305511, -6.359206544744109735, 47.99999999999997868 ) ) ;
#48220 = CARTESIAN_POINT ( 'NONE',  ( -17.57479954835421765, -7.360677901809306256, 63.74331195988233389 ) ) ;
#48221 = ORIENTED_EDGE ( 'NONE', *, *, #11208, .T. ) ;
#48222 = CARTESIAN_POINT ( 'NONE',  ( -18.36938390176548808, -21.74637740388497775, 72.35681286596320660 ) ) ;
#48223 = ORIENTED_EDGE ( 'NONE', *, *, #4136, .F. ) ;
#48224 = CARTESIAN_POINT ( 'NONE',  ( -50.42609385541305755, -14.80920654474419074, 65.04705882352939739 ) ) ;
#48225 = CARTESIAN_POINT ( 'NONE',  ( -22.56207008003183745, -19.63703213565221617, 72.92928497383269359 ) ) ;
#48226 = CARTESIAN_POINT ( 'NONE',  ( -21.44055400477819973, -12.39439182751215718, 52.02966884056656482 ) ) ;
#48227 = ORIENTED_EDGE ( 'NONE', *, *, #4418, .F. ) ;
#48228 = CARTESIAN_POINT ( 'NONE',  ( -22.10679845867080928, -14.99777973644470919, 49.52966884056655772 ) ) ;
#48229 = DIRECTION ( 'NONE',  ( -3.071710424422018668E-17, 6.404604876783312462E-16, 1.000000000000000000 ) ) ;
#48230 = CARTESIAN_POINT ( 'NONE',  ( -23.72594254189621310, -11.64830526502516328, 63.24658506625491583 ) ) ;
#48231 = AXIS2_PLACEMENT_3D ( 'NONE', #43885, #39927, #10138 ) ;
#48232 = VERTEX_POINT ( 'NONE', #26516 ) ;
#48233 = EDGE_LOOP ( 'NONE', ( #17684, #22737 ) ) ;
#48234 = CARTESIAN_POINT ( 'NONE',  ( -12.91576191806997365, -9.388722997169709927, 71.13453240065665284 ) ) ;
#48235 = CARTESIAN_POINT ( 'NONE',  ( -11.83951967486316192, -10.58871707758600600, 71.07779090859834525 ) ) ;
#48236 = DIRECTION ( 'NONE',  ( -0.05957303659011964347, -0.9982239494779874267, 2.515684304538401319E-08 ) ) ;
#48237 = CARTESIAN_POINT ( 'NONE',  ( -15.91784385759799392, -6.860780111191487229, 51.02154966934377711 ) ) ;
#48238 = CARTESIAN_POINT ( 'NONE',  ( -13.85393650630732054, -8.270265118416840977, 74.38450092284953996 ) ) ;
#48239 = DIRECTION ( 'NONE',  ( -3.071710424422018668E-17, 6.404604876783312462E-16, 1.000000000000000000 ) ) ;
#48240 = LINE ( 'NONE', #18435, #46769 ) ;
#48241 = DIRECTION ( 'NONE',  ( -0.3037135924646502394, 0.9527633776296274837, 2.170275161112374562E-08 ) ) ;
#48242 = ORIENTED_EDGE ( 'NONE', *, *, #9822, .F. ) ;
#48243 = EDGE_CURVE ( 'NONE', #31795, #23182, #2022, .T. ) ;
#48244 = DIRECTION ( 'NONE',  ( -0.003782665018460030538, -0.9999928456970870183, -9.532993539451315208E-09 ) ) ;
#48245 = EDGE_CURVE ( 'NONE', #22914, #26590, #659, .T. ) ;
#48246 = CARTESIAN_POINT ( 'NONE',  ( -18.40115675053315059, -19.96748611248585448, 50.77966884056656482 ) ) ;
#48247 = CARTESIAN_POINT ( 'NONE',  ( -13.59121668485792789, -8.949893101123375772, 60.62877463978671244 ) ) ;
#48248 =( BOUNDED_CURVE ( )  B_SPLINE_CURVE ( 3, ( #20469, #27603, #23923, #46577 ),
 .UNSPECIFIED., .F., .F. ) 
 B_SPLINE_CURVE_WITH_KNOTS ( ( 4, 4 ),
 ( 0.9074455897393665094, 1.000000000000000000 ),
 .UNSPECIFIED. ) 
 CURVE ( )  GEOMETRIC_REPRESENTATION_ITEM ( )  RATIONAL_B_SPLINE_CURVE ( ( 0.6983129098261009471, 0.7760317562607050856, 0.8765941196520047329, 1.000000000000000000 ) ) 
 REPRESENTATION_ITEM ( '' )  );
#48249 = VERTEX_POINT ( 'NONE', #15658 ) ;
#48250 = ORIENTED_EDGE ( 'NONE', *, *, #34366, .T. ) ;
#48251 = FACE_OUTER_BOUND ( 'NONE', #20450, .T. ) ;
#48252 = DIRECTION ( 'NONE',  ( 5.468526108419875108E-08, 8.832527038290525275E-06, -0.9999999999609916479 ) ) ;
#48253 = CARTESIAN_POINT ( 'NONE',  ( -11.73296596577226936, -10.64774513788296417, 74.72412863062541533 ) ) ;
#48254 = CARTESIAN_POINT ( 'NONE',  ( -36.42409385541304800, -8.109206544743658540, 50.50000000000030553 ) ) ;
#48255 =( BOUNDED_CURVE ( )  B_SPLINE_CURVE ( 3, ( #17209, #47277, #9849, #6390 ),
 .UNSPECIFIED., .F., .F. ) 
 B_SPLINE_CURVE_WITH_KNOTS ( ( 4, 4 ),
 ( 0.4074455897393672310, 0.5000000000000000000 ),
 .UNSPECIFIED. ) 
 CURVE ( )  GEOMETRIC_REPRESENTATION_ITEM ( )  RATIONAL_B_SPLINE_CURVE ( ( 0.6983129098261091627, 0.7760317562607090824, 0.8765941196520052880, 0.9999999999999952260 ) ) 
 REPRESENTATION_ITEM ( '' )  );
#48256 = ORIENTED_EDGE ( 'NONE', *, *, #19853, .T. ) ;
#48257 = EDGE_CURVE ( 'NONE', #22984, #15971, #11503, .T. ) ;
#48258 = CARTESIAN_POINT ( 'NONE',  ( -24.47131905756960890, -12.39240217952595913, 73.36412813348363215 ) ) ;
#48259 = CIRCLE ( 'NONE', #14523, 4.686499999999997890 ) ;
#48260 = CARTESIAN_POINT ( 'NONE',  ( -12.58002129225892674, -9.148929240056048684, 74.43427715830415536 ) ) ;
#48261 = EDGE_CURVE ( 'NONE', #38529, #39895, #45510, .T. ) ;
#48262 = EDGE_CURVE ( 'NONE', #29740, #39283, #45571, .T. ) ;
#48263 = EDGE_CURVE ( 'NONE', #42051, #35450, #43135, .T. ) ;
#48264 = VECTOR ( 'NONE', #14580, 1000.000000000000000 ) ;
#48265 = VERTEX_POINT ( 'NONE', #38300 ) ;
#48266 = DIRECTION ( 'NONE',  ( 1.000000000000000000, 2.866981220435666553E-17, 0.000000000000000000 ) ) ;
#48267 = CARTESIAN_POINT ( 'NONE',  ( -17.72634068467203505, -21.85272461955047874, 58.70553378267868538 ) ) ;
#48268 = CARTESIAN_POINT ( 'NONE',  ( -14.76026690907102790, -8.277937858068607824, 57.05820006608990269 ) ) ;
#48269 = ORIENTED_EDGE ( 'NONE', *, *, #7584, .T. ) ;
#48270 = LINE ( 'NONE', #6191, #32242 ) ;
#48271 =( BOUNDED_SURFACE ( )  B_SPLINE_SURFACE ( 3, 1, ( 
 ( #43834, #47518 ),
 ( #18180, #33428 ),
 ( #29520, #13986 ),
 ( #10805, #40129 ),
 ( #14702, #21650 ),
 ( #36637, #17694 ),
 ( #32721, #44802 ) ),
 .UNSPECIFIED., .T., .F., .F. ) 
 B_SPLINE_SURFACE_WITH_KNOTS ( ( 4, 3, 4 ),
 ( 2, 2 ),
 ( 0.000000000000000000, 0.5000000000000000000, 1.000000000000000000 ),
 ( 0.000000000000000000, 1.000000000000000000 ),
 .UNSPECIFIED. ) 
 GEOMETRIC_REPRESENTATION_ITEM ( )  RATIONAL_B_SPLINE_SURFACE ( (
 ( 1.000000000000000000, 1.000000000000000000),
 ( 0.3333333333333335369, 0.3333333333333330373),
 ( 0.3333333333333335369, 0.3333333333333330373),
 ( 1.000000000000000000, 1.000000000000000000),
 ( 0.3333333333333333703, 0.3333333333333333703),
 ( 0.3333333333333333703, 0.3333333333333333703),
 ( 1.000000000000000000, 1.000000000000000000) ) ) 
 REPRESENTATION_ITEM ( '' )  SURFACE ( )  );
#48272 = ORIENTED_EDGE ( 'NONE', *, *, #25302, .F. ) ;
#48273 = CARTESIAN_POINT ( 'NONE',  ( -19.10745041116545906, -21.66349580942223341, 62.13936675129127707 ) ) ;
#48274 = LINE ( 'NONE', #25624, #39158 ) ;
#48275 = EDGE_LOOP ( 'NONE', ( #46189, #43024, #12450, #26212, #10270 ) ) ;
#48276 = CARTESIAN_POINT ( 'NONE',  ( -12.36794899618824140, -19.72224014812425352, 61.69678633597965955 ) ) ;
#48277 = CARTESIAN_POINT ( 'NONE',  ( -10.45859239952313224, -15.89938452881993847, 64.79299464097340433 ) ) ;
#48278 = CARTESIAN_POINT ( 'NONE',  ( -19.57409385650551670, -9.792211528768504536, 50.49490371617623197 ) ) ;
#48279 = CARTESIAN_POINT ( 'NONE',  ( -18.11396590982544197, -21.77512906430638040, 65.64532159443497505 ) ) ;
#48280 = CARTESIAN_POINT ( 'NONE',  ( -23.80175822008580866, -17.82088921309938812, 62.88849600917846061 ) ) ;
#48281 = DIRECTION ( 'NONE',  ( -0.3478314405900309603, -0.9375570856950864451, 9.567072274253696421E-17 ) ) ;
#48282 = FACE_OUTER_BOUND ( 'NONE', #5076, .T. ) ;
#48283 = VERTEX_POINT ( 'NONE', #14656 ) ;
#48284 = CARTESIAN_POINT ( 'NONE',  ( -20.37299714182665866, -8.405577154986387356, 67.08104082189564110 ) ) ;
#48285 = DIRECTION ( 'NONE',  ( -5.828394480008251615E-08, 1.590814170208496341E-07, 0.9999999999999855671 ) ) ;
#48286 = CARTESIAN_POINT ( 'NONE',  ( -14.49278865106054504, -7.959940993718208624, 63.95125321502179361 ) ) ;
#48287 = DIRECTION ( 'NONE',  ( 0.8447509909909737269, -0.5351595679979644915, 3.339321029457338869E-17 ) ) ;
#48288 = CARTESIAN_POINT ( 'NONE',  ( -17.15999057916966208, -7.814067853132777408, 70.49035844391949013 ) ) ;
#48289 = ADVANCED_FACE ( 'NONE', ( #4594 ), #17570, .T. ) ;
#48290 = ORIENTED_EDGE ( 'NONE', *, *, #16286, .F. ) ;
#48291 = ORIENTED_EDGE ( 'NONE', *, *, #3819, .T. ) ;
#48292 = CARTESIAN_POINT ( 'NONE',  ( -16.94342272711102027, -21.79279426035641976, 72.46543237156552664 ) ) ;
#48293 = CARTESIAN_POINT ( 'NONE',  ( -9.975448439439539072, -14.66457030764845193, 71.52120984734268916 ) ) ;
#48294 = ORIENTED_EDGE ( 'NONE', *, *, #7514, .T. ) ;
#48295 = CARTESIAN_POINT ( 'NONE',  ( -13.22529448846758982, -9.145569705956512863, 64.19474388871357462 ) ) ;
#48296 = CARTESIAN_POINT ( 'NONE',  ( -11.29272648115082589, -18.18986258437042736, 57.91787737795063862 ) ) ;
#48297 = DIRECTION ( 'NONE',  ( 0.000000000000000000, 0.000000000000000000, 1.000000000000000000 ) ) ;
#48298 = CARTESIAN_POINT ( 'NONE',  ( -13.83484324388145303, -17.82260368047347399, 49.52966884056656482 ) ) ;
#48299 = CARTESIAN_POINT ( 'NONE',  ( -24.75425692978680559, -16.14426119111164937, 62.70673273743753384 ) ) ;
#48300 = DIRECTION ( 'NONE',  ( -5.551115123125782702E-17, -1.232595164407830946E-32, -1.000000000000000000 ) ) ;
#48301 = DIRECTION ( 'NONE',  ( -3.071710424422018668E-17, 6.404604876783312462E-16, 1.000000000000000000 ) ) ;
#48302 = AXIS2_PLACEMENT_3D ( 'NONE', #1306, #8964, #5026 ) ;
#48303 = CARTESIAN_POINT ( 'NONE',  ( -16.26184114368905043, -7.855670183028919062, 60.20028478909662084 ) ) ;
#48304 = VERTEX_POINT ( 'NONE', #45961 ) ;
#48305 = CIRCLE ( 'NONE', #32603, 5.249999999999998224 ) ;
#48306 = LINE ( 'NONE', #4001, #40813 ) ;
#48307 = PLANE ( 'NONE',  #40768 ) ;
#48308 = EDGE_CURVE ( 'NONE', #1846, #1214, #30949, .T. ) ;
#48309 = CARTESIAN_POINT ( 'NONE',  ( -17.02409385541306008, -14.80920654474411080, 75.49999999999998579 ) ) ;
#48310 = CARTESIAN_POINT ( 'NONE',  ( -24.28250243997646152, -13.40622297325496959, 59.37884623336672973 ) ) ;
#48311 = CARTESIAN_POINT ( 'NONE',  ( -24.59706363142188934, -12.79617847886399140, 66.48742024426742603 ) ) ;
#48312 = CARTESIAN_POINT ( 'NONE',  ( -11.85858129499141178, -10.56289031856201710, 74.45501804502151799 ) ) ;
#48313 = CARTESIAN_POINT ( 'NONE',  ( -17.20139284005516700, -7.812749994621428051, 70.79035839633094440 ) ) ;
#48314 = VERTEX_POINT ( 'NONE', #16135 ) ;
#48315 = ORIENTED_EDGE ( 'NONE', *, *, #15512, .T. ) ;
#48316 = CARTESIAN_POINT ( 'NONE',  ( -14.42409385541304090, -9.359200813967568422, 50.49621490985803263 ) ) ;
#48317 = VERTEX_POINT ( 'NONE', #21010 ) ;
#48318 = MANIFOLD_SOLID_BREP ( 'Stock-MAS-175-1', #10259 ) ;
#48319 = DIRECTION ( 'NONE',  ( 1.000000000000000000, -4.164305804376849172E-17, 1.614929280266638808E-16 ) ) ;
#48320 = DIRECTION ( 'NONE',  ( -0.5097212845717549179, 0.8603395911234820170, 0.000000000000000000 ) ) ;
#48321 = EDGE_CURVE ( 'NONE', #42340, #45965, #34255, .T. ) ;
#48322 = EDGE_CURVE ( 'NONE', #37303, #3283, #47308, .T. ) ;
#48323 = CARTESIAN_POINT ( 'NONE',  ( -9.974235501303020612, -14.86645057852294016, 75.05424837986554110 ) ) ;
#48324 = VERTEX_POINT ( 'NONE', #5762 ) ;
#48325 = CARTESIAN_POINT ( 'NONE',  ( -23.10889842201686761, -9.994063388419718308, 66.74193459406681939 ) ) ;
#48326 = FACE_OUTER_BOUND ( 'NONE', #18200, .T. ) ;
#48327 = VERTEX_POINT ( 'NONE', #47368 ) ;
#48328 = DIRECTION ( 'NONE',  ( 1.000000000000000000, -1.224646799147353207E-16, 4.267285103686821372E-17 ) ) ;
#48329 = DIRECTION ( 'NONE',  ( 1.927470528863119542E-16, 0.000000000000000000, -1.000000000000000000 ) ) ;
#48330 = AXIS2_PLACEMENT_3D ( 'NONE', #43026, #20630, #9790 ) ;
#48331 = ORIENTED_EDGE ( 'NONE', *, *, #18386, .F. ) ;
#48332 = EDGE_CURVE ( 'NONE', #48324, #2071, #6238, .T. ) ;
#48333 = EDGE_CURVE ( 'NONE', #2842, #23748, #26080, .T. ) ;
#48334 = B_SPLINE_CURVE_WITH_KNOTS ( 'NONE', 3,
 ( #10393, #34, #36458, #25631, #29088, #21701, #26367, #37179, #36942, #18233 ),
 .UNSPECIFIED., .F., .F.,
 ( 4, 2, 2, 2, 4 ),
 ( 0.000000000000000000, 0.2500000000000000000, 0.5000000000000000000, 0.7500000000000000000, 1.000000000000000000 ),
 .UNSPECIFIED. ) ;
#48335 = CARTESIAN_POINT ( 'NONE',  ( -17.76160456433342461, -7.366686981516495258, 60.24094141105150868 ) ) ;
#48336 = CARTESIAN_POINT ( 'NONE',  ( -15.02609155194205037, -8.232647636148229253, 56.84999999999993037 ) ) ;
#48337 = CARTESIAN_POINT ( 'NONE',  ( -18.41784385541318159, -6.860780111190566188, 51.02154966934286762 ) ) ;
#48338 = ORIENTED_EDGE ( 'NONE', *, *, #20435, .F. ) ;
#48339 = CARTESIAN_POINT ( 'NONE',  ( -11.05034076241727625, -11.79557573020262318, 71.37388789199357575 ) ) ;
#48340 = AXIS2_PLACEMENT_3D ( 'NONE', #20207, #31781, #28077 ) ;
#48341 = CARTESIAN_POINT ( 'NONE',  ( -24.71300512064630794, -13.26796065199660113, 59.61913874400077873 ) ) ;
#48342 = CARTESIAN_POINT ( 'NONE',  ( -23.94283526169594722, -17.36006291627137088, 66.22891933742413073 ) ) ;
#48343 = VERTEX_POINT ( 'NONE', #32094 ) ;
#48344 = CARTESIAN_POINT ( 'NONE',  ( -10.96921284960095555, -11.97350354382807680, 74.84368195529052059 ) ) ;
#48345 = CARTESIAN_POINT ( 'NONE',  ( -17.42409385541299471, -14.80920654474434883, 62.02966884056656482 ) ) ;
#48346 = CARTESIAN_POINT ( 'NONE',  ( -15.35564964753334394, -21.49796208608013259, 72.27405351148586021 ) ) ;
#48347 = CARTESIAN_POINT ( 'NONE',  ( -16.16748626245079379, -22.20318634978239203, 53.49999999999994316 ) ) ;
#48348 = DIRECTION ( 'NONE',  ( -0.4251432040024066272, -0.9051260995521939190, -1.185120001106687566E-09 ) ) ;
#48349 = EDGE_CURVE ( 'NONE', #4839, #28413, #9929, .T. ) ;
#48350 = EDGE_LOOP ( 'NONE', ( #29175, #39565, #16119, #994, #6770 ) ) ;
#48351 = CARTESIAN_POINT ( 'NONE',  ( -16.19792114999740562, -7.866354181730329742, 60.48556343814865954 ) ) ;
#48352 = CARTESIAN_POINT ( 'NONE',  ( -45.37196614242555626, -14.20920654474410760, 70.56550563755274652 ) ) ;
#48353 = ORIENTED_EDGE ( 'NONE', *, *, #37081, .F. ) ;
#48354 = CARTESIAN_POINT ( 'NONE',  ( -18.48323135481441426, -7.889672941340453605, 74.14064351459154523 ) ) ;
#48355 =( BOUNDED_CURVE ( )  B_SPLINE_CURVE ( 3, ( #2955, #25383, #40161, #40393 ),
 .UNSPECIFIED., .F., .F. ) 
 B_SPLINE_CURVE_WITH_KNOTS ( ( 4, 4 ),
 ( 0.5000000000000000000, 0.9074455897393605142 ),
 .UNSPECIFIED. ) 
 CURVE ( )  GEOMETRIC_REPRESENTATION_ITEM ( )  RATIONAL_B_SPLINE_CURVE ( ( 0.9999999999999961142, 0.4567392136813419601, 0.3561768502900365396, 0.6983129098260758560 ) ) 
 REPRESENTATION_ITEM ( '' )  );
#48356 = FACE_OUTER_BOUND ( 'NONE', #48167, .T. ) ;
#48357 = LINE ( 'NONE', #44688, #10857 ) ;
#48358 = ORIENTED_EDGE ( 'NONE', *, *, #24775, .F. ) ;
#48359 = CARTESIAN_POINT ( 'NONE',  ( -19.85889901765038346, -21.37233916515964438, 69.21353063550283480 ) ) ;
#48360 = CARTESIAN_POINT ( 'NONE',  ( -20.60942684424193416, -21.09890871138989965, 58.65947248567252359 ) ) ;
#48361 = ORIENTED_EDGE ( 'NONE', *, *, #29316, .F. ) ;
#48362 = ORIENTED_EDGE ( 'NONE', *, *, #35322, .F. ) ;
#48363 = ORIENTED_EDGE ( 'NONE', *, *, #25759, .F. ) ;
#48364 = CARTESIAN_POINT ( 'NONE',  ( -13.52409385650551599, -6.426201560718813433, 50.50509628382439331 ) ) ;
#48365 = DIRECTION ( 'NONE',  ( 3.071710424422018668E-17, -6.404604876783312462E-16, -1.000000000000000000 ) ) ;
#48366 = LINE ( 'NONE', #15350, #8042 ) ;
#48367 = CARTESIAN_POINT ( 'NONE',  ( -21.99178428503401861, -9.439038574390064440, 60.02171213140443484 ) ) ;
#48368 = CARTESIAN_POINT ( 'NONE',  ( -21.93659385759799108, -8.995762431863214559, 51.38120296130585274 ) ) ;
#48369 = EDGE_LOOP ( 'NONE', ( #4248, #21019, #25614, #25925, #37825 ) ) ;
#48370 = ORIENTED_EDGE ( 'NONE', *, *, #20604, .T. ) ;
#48371 = CIRCLE ( 'NONE', #41310, 4.686499999999998778 ) ;
#48372 = CARTESIAN_POINT ( 'NONE',  ( -16.14284385650552167, -8.811426318492348031, 52.18089403414751359 ) ) ;
#48373 = AXIS2_PLACEMENT_3D ( 'NONE', #2273, #21954, #39702 ) ;
#48374 = CARTESIAN_POINT ( 'NONE',  ( -11.46723045859082468, -10.33494501157577972, 74.63223394389621035 ) ) ;
#48375 = CARTESIAN_POINT ( 'NONE',  ( -12.81450527785482052, -9.474959380418823685, 74.61923006088066757 ) ) ;
#48376 = CARTESIAN_POINT ( 'NONE',  ( -16.59284385650551741, -7.406986770994973490, 48.81910596585309747 ) ) ;
#48377 = ORIENTED_EDGE ( 'NONE', *, *, #19853, .F. ) ;
#48378 = ADVANCED_FACE ( 'NONE', ( #1131 ), #32572, .T. ) ;
#48379 = CARTESIAN_POINT ( 'NONE',  ( -10.78978129071826686, -12.42417052737942917, 57.32857332104949677 ) ) ;
#48380 = CARTESIAN_POINT ( 'NONE',  ( -36.42409385541304800, -8.109206544743658540, 50.50000000000030553 ) ) ;
#48381 = CARTESIAN_POINT ( 'NONE',  ( -23.51785719624223958, -11.36449344406884343, 70.19210750610864125 ) ) ;
#48382 = VERTEX_POINT ( 'NONE', #6236 ) ;
#48383 = DIRECTION ( 'NONE',  ( -0.2196488028684550897, -0.9755790093059856227, 7.835600157697874713E-08 ) ) ;
#48384 = ORIENTED_EDGE ( 'NONE', *, *, #23366, .T. ) ;
#48385 = EDGE_CURVE ( 'NONE', #35067, #41098, #29635, .T. ) ;
#48386 = B_SPLINE_CURVE_WITH_KNOTS ( 'NONE', 3,
 ( #27620, #4736, #34513, #12117, #8918, #46094, #38699, #42409, #42658, #19499 ),
 .UNSPECIFIED., .F., .F.,
 ( 4, 2, 2, 2, 4 ),
 ( 0.1272669073658555250, 0.2522669073463344458, 0.3772669073268133388, 0.5022669073072922874, 0.6272669072877712360 ),
 .UNSPECIFIED. ) ;
#48387 = CARTESIAN_POINT ( 'NONE',  ( -22.22492895683646807, -9.112220634607178127, 59.76525293062090327 ) ) ;
#48388 = DIRECTION ( 'NONE',  ( -3.413470714839332458E-33, 1.190614954331866791E-16, -1.000000000000000000 ) ) ;
#48389 = CARTESIAN_POINT ( 'NONE',  ( -24.42401643431037073, -14.84212902100172293, 59.54300237020546405 ) ) ;
#48390 = CARTESIAN_POINT ( 'NONE',  ( -10.41803450628629157, -12.27586432466274502, 57.42883078543415110 ) ) ;
#48391 = EDGE_CURVE ( 'NONE', #3423, #12981, #41175, .T. ) ;
#48392 = EDGE_LOOP ( 'NONE', ( #370, #48272, #26923, #47275 ) ) ;
#48393 = CARTESIAN_POINT ( 'NONE',  ( -11.09928078071809487, -10.87206734048183243, 57.33090417946287687 ) ) ;
#48394 = CARTESIAN_POINT ( 'NONE',  ( -46.92409385541305511, -17.80920654474410370, 62.75000000000000000 ) ) ;
#48395 = EDGE_CURVE ( 'NONE', #27032, #39770, #4613, .T. ) ;
#48396 = B_SPLINE_CURVE_WITH_KNOTS ( 'NONE', 3,
 ( #3053, #18812, #44939, #41218, #26446, #25962, #18305, #41462, #33316, #48122 ),
 .UNSPECIFIED., .F., .F.,
 ( 4, 2, 2, 2, 4 ),
 ( 0.000000000000000000, 0.2500000000000000000, 0.5000000000000000000, 0.7500000000000000000, 1.000000000000000000 ),
 .UNSPECIFIED. ) ;
#48397 =( BOUNDED_CURVE ( )  B_SPLINE_CURVE ( 3, ( #11446, #26470, #41485, #22794 ),
 .UNSPECIFIED., .F., .F. ) 
 B_SPLINE_CURVE_WITH_KNOTS ( ( 4, 4 ),
 ( 0.5000000000000000000, 0.9074455897393707282 ),
 .UNSPECIFIED. ) 
 CURVE ( )  GEOMETRIC_REPRESENTATION_ITEM ( )  RATIONAL_B_SPLINE_CURVE ( ( 0.9999999999999903411, 0.4567392136813203107, 0.3561768502900325983, 0.6983129098261168233 ) ) 
 REPRESENTATION_ITEM ( '' )  );
#48398 = CARTESIAN_POINT ( 'NONE',  ( -19.36811171093278006, -7.617188704462286353, 60.08280224782789958 ) ) ;
#48399 = DIRECTION ( 'NONE',  ( -2.866981220435666553E-17, 1.000000000000000000, 1.190614954331866791E-16 ) ) ;
#48400 = EDGE_LOOP ( 'NONE', ( #7048, #10594 ) ) ;
#48401 = CARTESIAN_POINT ( 'NONE',  ( -10.54259038139361770, -17.66360020425462451, 68.19698326179320702 ) ) ;
#48402 = CARTESIAN_POINT ( 'NONE',  ( -14.62876365129575795, -8.337020046287406672, 63.78978836832918375 ) ) ;
#48403 = CARTESIAN_POINT ( 'NONE',  ( -18.79049830835916524, -7.892586073225762000, 70.38540174208183942 ) ) ;
#48404 = ORIENTED_EDGE ( 'NONE', *, *, #13541, .T. ) ;
#48405 = CIRCLE ( 'NONE', #32660, 1.500000000000001332 ) ;
#48406 = FACE_BOUND ( 'NONE', #22176, .T. ) ;
#48407 = ORIENTED_EDGE ( 'NONE', *, *, #41946, .F. ) ;
#48408 = CARTESIAN_POINT ( 'NONE',  ( 18.46573386768564973, 2.144455078683989768, 49.30629848276630156 ) ) ;
#48409 = CARTESIAN_POINT ( 'NONE',  ( -13.68917838456570024, -20.72961559785960617, 61.58934264708406658 ) ) ;
#48410 = DIRECTION ( 'NONE',  ( 0.000000000000000000, 0.000000000000000000, 1.000000000000000000 ) ) ;
#48411 = DIRECTION ( 'NONE',  ( -0.000000000000000000, -1.000000000000000000, -0.000000000000000000 ) ) ;
#48412 = EDGE_LOOP ( 'NONE', ( #35595, #33061, #33711, #40173 ) ) ;
#48413 = CARTESIAN_POINT ( 'NONE',  ( -24.45201636468676298, -14.25170757634699470, 69.95275273439749242 ) ) ;
#48414 = ORIENTED_EDGE ( 'NONE', *, *, #15245, .F. ) ;
#48415 = DIRECTION ( 'NONE',  ( -0.4780674886490097197, 0.8783231047267436864, 5.292596395488306339E-08 ) ) ;
#48416 = CARTESIAN_POINT ( 'NONE',  ( -15.35027142736847239, -7.653576728715946409, 74.26480947788739684 ) ) ;
#48417 = B_SPLINE_CURVE_WITH_KNOTS ( 'NONE', 1,
 ( #4043, #42437 ),
 .UNSPECIFIED., .F., .F.,
 ( 2, 2 ),
 ( 0.000000000000000000, 1.000000000000000000 ),
 .UNSPECIFIED. ) ;
#48418 = EDGE_LOOP ( 'NONE', ( #30827, #19306, #1011, #26245 ) ) ;
#48419 = CARTESIAN_POINT ( 'NONE',  ( -10.81484442788029376, -17.11524687497682251, 61.45743118925498294 ) ) ;
#48420 =( BOUNDED_CURVE ( )  B_SPLINE_CURVE ( 3, ( #9202, #24222, #39229, #43173 ),
 .UNSPECIFIED., .F., .F. ) 
 B_SPLINE_CURVE_WITH_KNOTS ( ( 4, 4 ),
 ( 0.5000000000000000000, 0.9074455897393625126 ),
 .UNSPECIFIED. ) 
 CURVE ( )  GEOMETRIC_REPRESENTATION_ITEM ( )  RATIONAL_B_SPLINE_CURVE ( ( 1.000000000000000666, 0.4567392136813430703, 0.3561768502900337641, 0.6983129098260736356 ) ) 
 REPRESENTATION_ITEM ( '' )  );
#48421 = CARTESIAN_POINT ( 'NONE',  ( -33.42409385541304800, -9.159201730891741278, 50.49682052428079970 ) ) ;
#48422 = VERTEX_POINT ( 'NONE', #14540 ) ;
#48423 = EDGE_LOOP ( 'NONE', ( #47035, #33313, #37862, #39687, #5116 ) ) ;
#48424 = CARTESIAN_POINT ( 'NONE',  ( -15.62268239484049026, -8.044906604745516887, 70.62492222724996793 ) ) ;
#48425 = DIRECTION ( 'NONE',  ( 1.081321489472432593E-05, 7.211308816928991536E-06, -0.9999999999155356756 ) ) ;
#48426 = CARTESIAN_POINT ( 'NONE',  ( -19.32828448179457581, -22.01175803993288227, 58.62533143847836214 ) ) ;
#48427 = CARTESIAN_POINT ( 'NONE',  ( -10.59838446366035924, -13.25112969284905695, 74.90647544603520203 ) ) ;
#48428 = DIRECTION ( 'NONE',  ( 1.000000000000000000, 0.000000000000000000, -2.406186529621654018E-16 ) ) ;
#48429 = DIRECTION ( 'NONE',  ( 1.198821491151391801E-05, -1.588017923178218046E-05, 0.9999999998020513425 ) ) ;
#48430 = CARTESIAN_POINT ( 'NONE',  ( -20.67761229128902656, -8.545853924536821467, 66.92536870251414882 ) ) ;
#48431 = ORIENTED_EDGE ( 'NONE', *, *, #17044, .F. ) ;
#48432 = ORIENTED_EDGE ( 'NONE', *, *, #21964, .F. ) ;
#48433 = FACE_OUTER_BOUND ( 'NONE', #14197, .T. ) ;
#48434 = CARTESIAN_POINT ( 'NONE',  ( -23.07906183844443859, -9.958936969296642516, 66.72677665813928627 ) ) ;
#48435 = CARTESIAN_POINT ( 'NONE',  ( -21.91379008343609769, -9.437005872758499336, 63.26324041012450294 ) ) ;
#48436 = CARTESIAN_POINT ( 'NONE',  ( -17.91451193640577344, -22.24313339626381847, 61.99040498927033127 ) ) ;
#48437 = ORIENTED_EDGE ( 'NONE', *, *, #44528, .T. ) ;
#48438 = EDGE_CURVE ( 'NONE', #43420, #34242, #16273, .T. ) ;
#48439 = CARTESIAN_POINT ( 'NONE',  ( -19.65534385650552451, -7.417179338643134834, 52.18511593390279302 ) ) ;
#48440 = AXIS2_PLACEMENT_3D ( 'NONE', #29499, #41312, #18646 ) ;
#48441 = AXIS2_PLACEMENT_3D ( 'NONE', #31248, #47242, #39603 ) ;
#48442 = ORIENTED_EDGE ( 'NONE', *, *, #36386, .T. ) ;
#48443 = CARTESIAN_POINT ( 'NONE',  ( -24.35706380436459995, -15.77560588608014136, 69.83307488757523629 ) ) ;
#48444 = CARTESIAN_POINT ( 'NONE',  ( 18.57590614458706924, 1.636933384339416264, 51.78951792648781804 ) ) ;
#48445 = CARTESIAN_POINT ( 'NONE',  ( -10.03884236986523604, -13.82852981289494210, 57.70470977341523167 ) ) ;
#48446 = ORIENTED_EDGE ( 'NONE', *, *, #4845, .F. ) ;
#48447 = CARTESIAN_POINT ( 'NONE',  ( -10.39044952859546278, -14.32866914145539994, 64.68803851576602426 ) ) ;
#48448 = CARTESIAN_POINT ( 'NONE',  ( -10.85841931818429629, -17.37798394237199062, 64.91267318220633342 ) ) ;
#48449 = EDGE_CURVE ( 'NONE', #21669, #35366, #24424, .T. ) ;
#48450 = ORIENTED_EDGE ( 'NONE', *, *, #6911, .F. ) ;
#48451 = FACE_OUTER_BOUND ( 'NONE', #756, .T. ) ;
#48452 = EDGE_CURVE ( 'NONE', #25220, #45934, #11140, .T. ) ;
#48453 = CARTESIAN_POINT ( 'NONE',  ( -46.29409385541305255, -14.20920654474410760, 69.94787228701220272 ) ) ;
#48454 = EDGE_LOOP ( 'NONE', ( #15664, #35015, #38636, #38618, #48477 ) ) ;
#48455 = CARTESIAN_POINT ( 'NONE',  ( -24.68275054790482770, -16.48720572190336853, 59.23837039904986312 ) ) ;
#48456 = VERTEX_POINT ( 'NONE', #14069 ) ;
#48457 = CARTESIAN_POINT ( 'NONE',  ( -10.32795594944829176, -17.07800752666445021, 57.88749324818159891 ) ) ;
#48458 = CARTESIAN_POINT ( 'NONE',  ( -17.65279228434817327, -7.362550528378125847, 63.71203517750778644 ) ) ;
#48459 = EDGE_CURVE ( 'NONE', #26800, #18999, #2766, .T. ) ;
#48460 = VERTEX_POINT ( 'NONE', #33769 ) ;
#48461 = CARTESIAN_POINT ( 'NONE',  ( -22.02798021202036693, -12.28596846334092163, 52.02966884056656482 ) ) ;
#48462 = CARTESIAN_POINT ( 'NONE',  ( -11.44359845021116939, -10.36664799652857738, 74.53861401861469460 ) ) ;
#48463 = EDGE_LOOP ( 'NONE', ( #47926, #19654 ) ) ;
#48464 = ADVANCED_BREP_SHAPE_REPRESENTATION ( '', ( #31971, #29031 ), #23534 ) ;
#48465 = CYLINDRICAL_SURFACE ( 'NONE', #44140, 6.899999999999999467 ) ;
#48466 = EDGE_CURVE ( 'NONE', #46554, #4981, #14312, .T. ) ;
#48467 = CARTESIAN_POINT ( 'NONE',  ( -21.99649211598757859, -13.72812852161587038, 52.02966884056656482 ) ) ;
#48468 = FACE_OUTER_BOUND ( 'NONE', #41180, .T. ) ;
#48469 = VERTEX_POINT ( 'NONE', #40675 ) ;
#48470 = CARTESIAN_POINT ( 'NONE',  ( -19.92825877560272474, -21.82574164115814241, 69.13493675705122143 ) ) ;
#48471 = EDGE_CURVE ( 'NONE', #6656, #11955, #36969, .T. ) ;
#48472 = VECTOR ( 'NONE', #6643, 1000.000000000000000 ) ;
#48473 = CIRCLE ( 'NONE', #42971, 4.686499999999998778 ) ;
#48474 = CARTESIAN_POINT ( 'NONE',  ( -23.33822317206753638, -19.33980969897947944, 59.07684782711321958 ) ) ;
#48475 = CARTESIAN_POINT ( 'NONE',  ( -23.07906183844443859, -9.958936969296642516, 66.72677665813928627 ) ) ;
#48476 = ORIENTED_EDGE ( 'NONE', *, *, #32711, .T. ) ;
#48477 = ORIENTED_EDGE ( 'NONE', *, *, #32110, .F. ) ;
#48478 = DIRECTION ( 'NONE',  ( -1.295331064632368052E-06, 6.890485867068654572E-07, 0.9999999999989236388 ) ) ;
#48479 = CARTESIAN_POINT ( 'NONE',  ( -24.71393967724174345, -16.34927462137609311, 59.23677039840046632 ) ) ;
#48480 = CARTESIAN_POINT ( 'NONE',  ( -15.58034385759798823, -9.360768649639302552, 51.01397948905922419 ) ) ;
#48481 = CARTESIAN_POINT ( 'NONE',  ( -17.42409385541299471, -14.80920654474435771, 49.52966884056655772 ) ) ;
#48482 = CARTESIAN_POINT ( 'NONE',  ( 18.57590614458706924, 1.890747609047893185, 50.53028072113869484 ) ) ;
#48483 = CARTESIAN_POINT ( 'NONE',  ( -13.40955617598886995, -17.25032161083215954, 49.52966884056655772 ) ) ;
#48484 = CARTESIAN_POINT ( 'NONE',  ( -16.49051187235095384, -22.20064845604942150, 65.38710926064737805 ) ) ;
#48485 = VERTEX_POINT ( 'NONE', #7459 ) ;
#48486 = PLANE ( 'NONE',  #31256 ) ;
#48487 = B_SPLINE_CURVE_WITH_KNOTS ( 'NONE', 1,
 ( #16206, #5154 ),
 .UNSPECIFIED., .F., .F.,
 ( 2, 2 ),
 ( 0.000000000000000000, 1.000000000000000000 ),
 .UNSPECIFIED. ) ;
#48488 = DIRECTION ( 'NONE',  ( -1.568615307090388417E-06, -3.599470258889626763E-09, 0.9999999999987696508 ) ) ;
#48489 = CARTESIAN_POINT ( 'NONE',  ( -21.57657733182563931, -11.59682721189465049, 49.52966884056655772 ) ) ;
#48490 = CARTESIAN_POINT ( 'NONE',  ( -15.03931914688375571, -19.48631565075837457, 49.52966884056656482 ) ) ;
#48491 = B_SPLINE_CURVE_WITH_KNOTS ( 'NONE', 3,
 ( #3534, #41210, #33809, #44677, #26438, #6755, #33304, #33552, #10934, #11182 ),
 .UNSPECIFIED., .F., .F.,
 ( 4, 2, 2, 2, 4 ),
 ( 0.000000000000000000, 0.2500000000000000000, 0.5000000000000000000, 0.7500000000000000000, 1.000000000000000000 ),
 .UNSPECIFIED. ) ;
#48492 = ADVANCED_FACE ( 'NONE', ( #3745 ), #48307, .T. ) ;
#48493 = VERTEX_POINT ( 'NONE', #21973 ) ;
#48494 = EDGE_LOOP ( 'NONE', ( #39669, #8816, #27342, #43835 ) ) ;
#48495 = CARTESIAN_POINT ( 'NONE',  ( -17.01596769717176372, -7.370308014455987156, 74.07522855441366971 ) ) ;
#48496 = CARTESIAN_POINT ( 'NONE',  ( -11.70172770812943774, -10.03875808374572287, 67.59873243498492457 ) ) ;
#48497 = CARTESIAN_POINT ( 'NONE',  ( -10.18728111218540811, -13.03902853868809331, 71.36975128029325788 ) ) ;
#48498 = ORIENTED_EDGE ( 'NONE', *, *, #32782, .T. ) ;
#48499 = B_SPLINE_CURVE_WITH_KNOTS ( 'NONE', 1,
 ( #11786, #34904 ),
 .UNSPECIFIED., .F., .F.,
 ( 2, 2 ),
 ( 0.000000000000000000, 1.000000000000000000 ),
 .UNSPECIFIED. ) ;
#48500 = ADVANCED_FACE ( 'NONE', ( #45131 ), #47777, .T. ) ;
#48501 = CARTESIAN_POINT ( 'NONE',  ( -23.57581499062783337, -11.46896930558791183, 66.70749160231869723 ) ) ;
#48502 = VECTOR ( 'NONE', #40855, 1000.000000000000000 ) ;
#48503 = AXIS2_PLACEMENT_3D ( 'NONE', #11674, #8006, #38744 ) ;
#48504 = CARTESIAN_POINT ( 'NONE',  ( -17.98584164848810474, -22.23808382151284491, 62.06031347038508983 ) ) ;
#48505 = VERTEX_POINT ( 'NONE', #26396 ) ;
#48506 = CARTESIAN_POINT ( 'NONE',  ( -22.01672489606083616, -9.455592232943528685, 63.28333892425339258 ) ) ;
#48507 = AXIS2_PLACEMENT_3D ( 'NONE', #16360, #17077, #13140 ) ;
#48508 = FACE_OUTER_BOUND ( 'NONE', #24544, .T. ) ;
#48509 = CARTESIAN_POINT ( 'NONE',  ( -10.82872617761508316, -17.15944594640560794, 64.73812395600515401 ) ) ;
#48510 = ORIENTED_EDGE ( 'NONE', *, *, #31556, .F. ) ;
#48511 = CARTESIAN_POINT ( 'NONE',  ( -21.71715633306545357, -9.279672604503980793, 66.67766661933269745 ) ) ;
#48512 = EDGE_LOOP ( 'NONE', ( #32955, #23739 ) ) ;
#48513 = DIRECTION ( 'NONE',  ( -0.9687793358424821033, 0.2479245821708679909, 0.000000000000000000 ) ) ;
#48514 = EDGE_CURVE ( 'NONE', #39816, #24743, #35565, .T. ) ;
#48515 = CARTESIAN_POINT ( 'NONE',  ( -17.26457240846633923, -7.760713630915982542, 70.50507891880883449 ) ) ;
#48516 = ORIENTED_EDGE ( 'NONE', *, *, #11882, .F. ) ;
#48517 = CARTESIAN_POINT ( 'NONE',  ( -24.45201643071094111, -14.25170847814747077, 69.65275273439885950 ) ) ;
#48518 = CARTESIAN_POINT ( 'NONE',  ( -11.96181431063714484, -19.87549516500596525, 58.11177798925346139 ) ) ;
#48519 = CARTESIAN_POINT ( 'NONE',  ( -20.19284385650551528, -7.406986770994972602, 48.81910596585309747 ) ) ;
#48520 = EDGE_CURVE ( 'NONE', #39727, #47438, #42151, .T. ) ;
#48521 = CARTESIAN_POINT ( 'NONE',  ( -14.32641747624960260, -8.531847389937860626, 67.33263202729305874 ) ) ;
#48522 = EDGE_CURVE ( 'NONE', #42196, #6295, #19553, .T. ) ;
#48523 = CARTESIAN_POINT ( 'NONE',  ( -24.46812100523181499, -14.51191712007779522, 66.19764790277996269 ) ) ;
#48524 = CYLINDRICAL_SURFACE ( 'NONE', #39464, 0.1500000000000015210 ) ;
#48525 = ORIENTED_EDGE ( 'NONE', *, *, #15006, .F. ) ;
#48526 = CARTESIAN_POINT ( 'NONE',  ( -12.27729947935473298, -9.991218615320079266, 60.85918086709605745 ) ) ;
#48527 = DIRECTION ( 'NONE',  ( -0.8949343913984795229, -0.4461977533473618918, 4.967883834297468681E-17 ) ) ;
#48528 = PLANE ( 'NONE',  #35332 ) ;
#48529 = B_SPLINE_CURVE_WITH_KNOTS ( 'NONE', 3,
 ( #43728, #13415, #11136, #28465, #32398, #26159, #39772, #9512, #36308, #6535 ),
 .UNSPECIFIED., .F., .F.,
 ( 4, 2, 2, 2, 4 ),
 ( 0.6272669072877752328, 0.7522669073072940638, 0.8772669073268128948, 1.002266907346331726, 1.127266907365850557 ),
 .UNSPECIFIED. ) ;
#48530 = FACE_OUTER_BOUND ( 'NONE', #32033, .T. ) ;
#48531 = CARTESIAN_POINT ( 'NONE',  ( -15.86788899160417721, -21.69347836327019863, 58.43018749706013182 ) ) ;
#48532 = CARTESIAN_POINT ( 'NONE',  ( -14.05371499411349667, -21.00138273984457982, 72.22607703579407712 ) ) ;
#48533 = ORIENTED_EDGE ( 'NONE', *, *, #26174, .F. ) ;
#48534 = EDGE_LOOP ( 'NONE', ( #12525, #23183, #40573, #27238, #35392 ) ) ;
#48535 = CARTESIAN_POINT ( 'NONE',  ( -11.03038783319414939, -18.63467225643333336, 61.46366213062071182 ) ) ;
#48536 = CARTESIAN_POINT ( 'NONE',  ( -21.86726817259849298, -9.330790031404522011, 66.96150205274950906 ) ) ;
#48537 = ORIENTED_EDGE ( 'NONE', *, *, #4365, .F. ) ;
#48538 = CARTESIAN_POINT ( 'NONE',  ( -24.02580441457500982, -11.35651424597849690, 66.67860437913579119 ) ) ;
#48539 = DIRECTION ( 'NONE',  ( 3.071710424422018668E-17, -6.404604876783312462E-16, -1.000000000000000000 ) ) ;
#48540 = DIRECTION ( 'NONE',  ( -0.9950649908465213356, -0.09922531930717198856, 4.894557008102619459E-08 ) ) ;
#48541 = LINE ( 'NONE', #14780, #19629 ) ;
#48542 =( BOUNDED_SURFACE ( )  B_SPLINE_SURFACE ( 3, 1, ( 
 ( #36003, #2756 ),
 ( #17290, #44162 ),
 ( #10411, #13587 ),
 ( #28633, #11130 ),
 ( #3248, #41401 ),
 ( #37198, #22708 ),
 ( #6705, #26152 ) ),
 .UNSPECIFIED., .T., .F., .F. ) 
 B_SPLINE_SURFACE_WITH_KNOTS ( ( 4, 3, 4 ),
 ( 2, 2 ),
 ( 0.000000000000000000, 0.5000000000000000000, 1.000000000000000000 ),
 ( 0.000000000000000000, 1.000000000000000000 ),
 .UNSPECIFIED. ) 
 GEOMETRIC_REPRESENTATION_ITEM ( )  RATIONAL_B_SPLINE_SURFACE ( (
 ( 1.000000000000000000, 1.000000000000000000),
 ( 0.3333333333333335369, 0.3333333333333330373),
 ( 0.3333333333333335369, 0.3333333333333330373),
 ( 1.000000000000000000, 1.000000000000000000),
 ( 0.3333333333333333703, 0.3333333333333333703),
 ( 0.3333333333333333703, 0.3333333333333333703),
 ( 1.000000000000000000, 1.000000000000000000) ) ) 
 REPRESENTATION_ITEM ( '' )  SURFACE ( )  );
#48543 = ADVANCED_FACE ( 'NONE', ( #4725 ), #19981, .T. ) ;
#48544 = CARTESIAN_POINT ( 'NONE',  ( -24.39228834030809878, -14.13809067987688195, 73.13888153319147989 ) ) ;
#48545 = CARTESIAN_POINT ( 'NONE',  ( -11.45298274964035556, -19.26444193807122929, 71.87960014491380889 ) ) ;
#48546 = EDGE_CURVE ( 'NONE', #34669, #14458, #1253, .T. ) ;
#48547 = AXIS2_PLACEMENT_3D ( 'NONE', #25129, #6892, #47766 ) ;
#48548 = DIRECTION ( 'NONE',  ( -0.7915359335728472390, -0.6111226275167354061, -5.146443701300863982E-08 ) ) ;
#48549 = AXIS2_PLACEMENT_3D ( 'NONE', #31261, #24373, #8868 ) ;
#48550 = CARTESIAN_POINT ( 'NONE',  ( 18.57590614458695200, 3.149984814396855182, 50.78409494584673922 ) ) ;
#48551 = EDGE_CURVE ( 'NONE', #13129, #12455, #26619, .T. ) ;
#48552 = EDGE_CURVE ( 'NONE', #1420, #10544, #19747, .T. ) ;
#48553 = ORIENTED_EDGE ( 'NONE', *, *, #45557, .F. ) ;
#48554 = DIRECTION ( 'NONE',  ( 3.549360974551883545E-17, -6.371834667872732552E-18, -1.000000000000000000 ) ) ;
#48555 = CARTESIAN_POINT ( 'NONE',  ( -11.54096866439503266, -18.60258178517703698, 61.50384087359334728 ) ) ;
#48556 = CARTESIAN_POINT ( 'NONE',  ( -19.85909577874797449, -21.37257635846961890, 72.46322212860958700 ) ) ;
#48557 = AXIS2_PLACEMENT_3D ( 'NONE', #19524, #31334, #46364 ) ;
#48558 = FACE_OUTER_BOUND ( 'NONE', #218, .T. ) ;
#48559 = CARTESIAN_POINT ( 'NONE',  ( -12.18719842096713180, -10.08886484896570934, 64.04386393395434141 ) ) ;
#48560 = CARTESIAN_POINT ( 'NONE',  ( -11.90143170752337731, -10.50540531864507798, 74.62812341533918925 ) ) ;
#48561 =( BOUNDED_SURFACE ( )  B_SPLINE_SURFACE ( 3, 1, ( 
 ( #37542, #22809 ),
 ( #30924, #15138 ),
 ( #30440, #45707 ),
 ( #26241, #38040 ),
 ( #11965, #37801 ),
 ( #45217, #41020 ),
 ( #3582, #392 ) ),
 .UNSPECIFIED., .T., .F., .F. ) 
 B_SPLINE_SURFACE_WITH_KNOTS ( ( 4, 3, 4 ),
 ( 2, 2 ),
 ( 0.000000000000000000, 0.5000000000000000000, 1.000000000000000000 ),
 ( 0.000000000000000000, 1.000000000000000000 ),
 .UNSPECIFIED. ) 
 GEOMETRIC_REPRESENTATION_ITEM ( )  RATIONAL_B_SPLINE_SURFACE ( (
 ( 1.000000000000000000, 1.000000000000000000),
 ( 0.3333333333333335369, 0.3333333333333330373),
 ( 0.3333333333333335369, 0.3333333333333330373),
 ( 1.000000000000000000, 1.000000000000000000),
 ( 0.3333333333333333703, 0.3333333333333333703),
 ( 0.3333333333333333703, 0.3333333333333333703),
 ( 1.000000000000000000, 1.000000000000000000) ) ) 
 REPRESENTATION_ITEM ( '' )  SURFACE ( )  );
#48562 = DIRECTION ( 'NONE',  ( 1.000000000000000000, 2.866981220435666553E-17, 0.000000000000000000 ) ) ;
#48563 =( BOUNDED_CURVE ( )  B_SPLINE_CURVE ( 3, ( #44573, #30056, #40387, #29064 ),
 .UNSPECIFIED., .F., .F. ) 
 B_SPLINE_CURVE_WITH_KNOTS ( ( 4, 4 ),
 ( 0.4074455897393656767, 0.5000000000000000000 ),
 .UNSPECIFIED. ) 
 CURVE ( )  GEOMETRIC_REPRESENTATION_ITEM ( )  RATIONAL_B_SPLINE_CURVE ( ( 0.6983129098260969503, 0.7760317562607026431, 0.8765941196520038448, 1.000000000000001554 ) ) 
 REPRESENTATION_ITEM ( '' )  );
#48564 = VERTEX_POINT ( 'NONE', #30839 ) ;
#48565 = ORIENTED_EDGE ( 'NONE', *, *, #1036, .T. ) ;
#48566 = CARTESIAN_POINT ( 'NONE',  ( -13.37522125781897664, -8.785794273635769258, 49.36370281465616472 ) ) ;
#48567 = ORIENTED_EDGE ( 'NONE', *, *, #23804, .F. ) ;
#48568 = CARTESIAN_POINT ( 'NONE',  ( -23.58184859397294630, -19.00269516279415072, 66.01663558220315053 ) ) ;
#48569 = MANIFOLD_SOLID_BREP ( 'Stock-MAS-175-1', #11842 ) ;
#48570 = LINE ( 'NONE', #11630, #18165 ) ;
#48571 =( BOUNDED_CURVE ( )  B_SPLINE_CURVE ( 3, ( #33056, #48099, #14330, #10673 ),
 .UNSPECIFIED., .F., .F. ) 
 B_SPLINE_CURVE_WITH_KNOTS ( ( 4, 4 ),
 ( 0.4074455897393634562, 0.5000000000000000000 ),
 .UNSPECIFIED. ) 
 CURVE ( )  GEOMETRIC_REPRESENTATION_ITEM ( )  RATIONAL_B_SPLINE_CURVE ( ( 0.6983129098261003920, 0.7760317562606982023, 0.8765941196519960732, 0.9999999999999898970 ) ) 
 REPRESENTATION_ITEM ( '' )  );
#48572 = ADVANCED_FACE ( 'NONE', ( #34016 ), #11870, .T. ) ;
#48573 = CARTESIAN_POINT ( 'NONE',  ( -16.40075914357782949, -21.78757426832101274, 58.17096681542334835 ) ) ;
#48574 = VERTEX_POINT ( 'NONE', #46333 ) ;
#48575 = CARTESIAN_POINT ( 'NONE',  ( -24.37710623504210972, -15.61986118777976351, 73.30303784451751881 ) ) ;
#48576 = CIRCLE ( 'NONE', #27353, 1.999999999999998668 ) ;
#48577 = FACE_OUTER_BOUND ( 'NONE', #33670, .T. ) ;
#48578 = ORIENTED_EDGE ( 'NONE', *, *, #15150, .T. ) ;
#48579 = CARTESIAN_POINT ( 'NONE',  ( -18.73034385759799036, -6.857644439848019857, 49.98602051094138687 ) ) ;
#48580 = CARTESIAN_POINT ( 'NONE',  ( -22.02798021202036693, -12.28596846334092163, 50.77966884056655772 ) ) ;
#48581 = AXIS2_PLACEMENT_3D ( 'NONE', #6624, #32709, #43822 ) ;
#48582 = AXIS2_PLACEMENT_3D ( 'NONE', #32062, #35259, #39689 ) ;
#48583 = ORIENTED_EDGE ( 'NONE', *, *, #38661, .F. ) ;
#48584 = CARTESIAN_POINT ( 'NONE',  ( -17.42409385541299471, -14.80920654474435594, 52.02966884056656482 ) ) ;
#48585 = EDGE_CURVE ( 'NONE', #35502, #20596, #615, .T. ) ;
#48586 = EDGE_LOOP ( 'NONE', ( #9348, #15117, #30947, #47058, #14751 ) ) ;
#48587 = CARTESIAN_POINT ( 'NONE',  ( -20.16576726592704816, -7.882025747994209297, 73.92107795202292664 ) ) ;
#48588 = CARTESIAN_POINT ( 'NONE',  ( -7.424093855413048892, -25.10920654474410441, 77.00000000000000000 ) ) ;
#48589 = AXIS2_PLACEMENT_3D ( 'NONE', #16552, #31592, #13575 ) ;
#48590 = DIRECTION ( 'NONE',  ( -3.071710424422018668E-17, 6.404604876783312462E-16, 1.000000000000000000 ) ) ;
#48591 = ORIENTED_EDGE ( 'NONE', *, *, #3192, .F. ) ;
#48592 = CARTESIAN_POINT ( 'NONE',  ( -11.49911252271374273, -19.32675654123934095, 71.80030491464860631 ) ) ;
#48593 = CARTESIAN_POINT ( 'NONE',  ( -24.31482381427648676, -13.31912605980313558, 59.36267924676593566 ) ) ;
#48594 = CYLINDRICAL_SURFACE ( 'NONE', #34917, 0.1499999999999956923 ) ;
#48595 = FACE_OUTER_BOUND ( 'NONE', #812, .T. ) ;
#48596 = CARTESIAN_POINT ( 'NONE',  ( -21.34284385650552096, -8.811426318492348031, 52.18089403414751359 ) ) ;
#48597 = VERTEX_POINT ( 'NONE', #1026 ) ;
#48598 = CARTESIAN_POINT ( 'NONE',  ( -17.56543669569624200, -7.757010706903894715, 60.28880713344695153 ) ) ;
#48599 = CARTESIAN_POINT ( 'NONE',  ( -21.20534385759799179, -7.595227055684746986, 51.75156210489594599 ) ) ;
#48600 = ORIENTED_EDGE ( 'NONE', *, *, #44963, .F. ) ;
#48601 = DIRECTION ( 'NONE',  ( 2.866981220435666553E-17, -1.000000000000000000, -1.190614954331866791E-16 ) ) ;
#48602 = CARTESIAN_POINT ( 'NONE',  ( -15.31139031680343265, -21.53908972589017523, 65.10596667083625277 ) ) ;
#48603 = CARTESIAN_POINT ( 'NONE',  ( -11.73750174563382842, -9.995990130843292576, 67.62179972804649708 ) ) ;
#48604 = ORIENTED_EDGE ( 'NONE', *, *, #44461, .F. ) ;
#48605 = CARTESIAN_POINT ( 'NONE',  ( -27.51331730537552289, -17.63476259924578926, 53.49999999999995026 ) ) ;
#48606 = EDGE_CURVE ( 'NONE', #41721, #19733, #22716, .T. ) ;
#48607 = CARTESIAN_POINT ( 'NONE',  ( -10.69617304350202325, -12.87194201418225425, 67.96662265532526703 ) ) ;
#48608 = B_SPLINE_CURVE_WITH_KNOTS ( 'NONE', 1,
 ( #35796, #36510 ),
 .UNSPECIFIED., .F., .F.,
 ( 2, 2 ),
 ( 0.000000000000000000, 1.000000000000000000 ),
 .UNSPECIFIED. ) ;
#48609 = EDGE_CURVE ( 'NONE', #21691, #15253, #44938, .T. ) ;
#48610 = EDGE_CURVE ( 'NONE', #29613, #42423, #27365, .T. ) ;
#48611 = EDGE_LOOP ( 'NONE', ( #28986, #326, #43892, #48432 ) ) ;
#48612 = ORIENTED_EDGE ( 'NONE', *, *, #25159, .T. ) ;
#48613 = CARTESIAN_POINT ( 'NONE',  ( -14.31159385650551741, -6.922745924619793101, 51.69366785382590024 ) ) ;
#48614 = VECTOR ( 'NONE', #22423, 1000.000000000000000 ) ;
#48615 = CARTESIAN_POINT ( 'NONE',  ( -14.27319436148695431, -8.558459998996717388, 71.02957628730779049 ) ) ;
#48616 = AXIS2_PLACEMENT_3D ( 'NONE', #30648, #590, #27178 ) ;
#48617 = CARTESIAN_POINT ( 'NONE',  ( -22.36602013069261119, -13.03724021049843174, 50.77966884056655772 ) ) ;
#48618 = CARTESIAN_POINT ( 'NONE',  ( -13.49267557974227394, -8.956801037788498121, 60.45422421514565059 ) ) ;
#48619 = VECTOR ( 'NONE', #26809, 1000.000000000000114 ) ;
#48620 = ORIENTED_EDGE ( 'NONE', *, *, #22571, .F. ) ;
#48621 = ORIENTED_EDGE ( 'NONE', *, *, #28138, .F. ) ;
#48622 = EDGE_CURVE ( 'NONE', #30719, #14265, #19703, .T. ) ;
#48623 = EDGE_CURVE ( 'NONE', #19435, #34717, #36404, .T. ) ;
#48624 = CARTESIAN_POINT ( 'NONE',  ( -13.94909385650551492, -8.104110260919579645, 48.81699501597546487 ) ) ;
#48625 = CARTESIAN_POINT ( 'NONE',  ( -22.17153284776674482, -17.05070671513899683, 52.02966884056656482 ) ) ;
#48626 = VECTOR ( 'NONE', #1108, 1000.000000000000000 ) ;
#48627 = CARTESIAN_POINT ( 'NONE',  ( -10.86565573107777283, -17.25601865228567533, 61.26629164091806246 ) ) ;
#48628 = CARTESIAN_POINT ( 'NONE',  ( -16.36784385650551954, -6.428312510596451368, 51.20221977374900035 ) ) ;
#48629 = ORIENTED_EDGE ( 'NONE', *, *, #20116, .F. ) ;
#48630 = ADVANCED_FACE ( 'NONE', ( #16513 ), #10680, .T. ) ;
#48631 = CARTESIAN_POINT ( 'NONE',  ( -13.89433361489564156, -8.703010632355098863, 74.08466061421664506 ) ) ;
#48632 = CARTESIAN_POINT ( 'NONE',  ( -24.76566745545338222, -16.07607805037886450, 66.31970875637813378 ) ) ;
#48633 = EDGE_LOOP ( 'NONE', ( #24220, #3827, #35798, #1585, #23677 ) ) ;
#48634 = CARTESIAN_POINT ( 'NONE',  ( -28.42409385541305511, -25.10920654474410441, 52.99999999999997158 ) ) ;
#48635 = VERTEX_POINT ( 'NONE', #2227 ) ;
#48636 = FACE_OUTER_BOUND ( 'NONE', #12532, .T. ) ;
#48637 = FACE_OUTER_BOUND ( 'NONE', #25416, .T. ) ;
#48638 = CARTESIAN_POINT ( 'NONE',  ( -24.32886716615087153, -16.23426984194678724, 62.60800820172418923 ) ) ;
#48639 = CARTESIAN_POINT ( 'NONE',  ( -13.38462506958126141, -20.58719851387657940, 58.04650077714654088 ) ) ;
#48640 = ORIENTED_EDGE ( 'NONE', *, *, #42830, .F. ) ;
#48641 = CARTESIAN_POINT ( 'NONE',  ( -17.42409385541299471, -14.80920654474438614, 2.029618040566568027 ) ) ;
#48642 = CARTESIAN_POINT ( 'NONE',  ( -24.10584550580111340, -12.56049697540380095, 73.54225570139644219 ) ) ;
#48643 =( BOUNDED_SURFACE ( )  B_SPLINE_SURFACE ( 3, 1, ( 
 ( #15442, #40836 ),
 ( #37617, #10798 ),
 ( #18662, #25818 ),
 ( #22138, #33671 ),
 ( #7615, #7122 ),
 ( #3916, #33935 ),
 ( #37122, #26554 ) ),
 .UNSPECIFIED., .T., .F., .F. ) 
 B_SPLINE_SURFACE_WITH_KNOTS ( ( 4, 3, 4 ),
 ( 2, 2 ),
 ( 0.000000000000000000, 0.5000000000000000000, 1.000000000000000000 ),
 ( 0.000000000000000000, 1.000000000000000000 ),
 .UNSPECIFIED. ) 
 GEOMETRIC_REPRESENTATION_ITEM ( )  RATIONAL_B_SPLINE_SURFACE ( (
 ( 1.000000000000000000, 1.000000000000000000),
 ( 0.3333333333333335369, 0.3333333333333330373),
 ( 0.3333333333333335369, 0.3333333333333330373),
 ( 1.000000000000000000, 1.000000000000000000),
 ( 0.3333333333333333703, 0.3333333333333333703),
 ( 0.3333333333333333703, 0.3333333333333333703),
 ( 1.000000000000000000, 1.000000000000000000) ) ) 
 REPRESENTATION_ITEM ( '' )  SURFACE ( )  );
#48644 =( GEOMETRIC_REPRESENTATION_CONTEXT ( 3 ) GLOBAL_UNCERTAINTY_ASSIGNED_CONTEXT ( ( #40067 ) ) GLOBAL_UNIT_ASSIGNED_CONTEXT ( ( #47112, #42516, #39966 ) ) REPRESENTATION_CONTEXT ( 'NONE', 'WORKASPACE' ) );
#48645 = CARTESIAN_POINT ( 'NONE',  ( -21.01123981933952223, -20.87838139577334573, 65.73453944496496604 ) ) ;
#48646 = CARTESIAN_POINT ( 'NONE',  ( -21.43863153483710349, -12.36809147865652925, 49.52966884056655772 ) ) ;
#48647 = ORIENTED_EDGE ( 'NONE', *, *, #30353, .T. ) ;
#48648 = CARTESIAN_POINT ( 'NONE',  ( -10.55699114952331996, -17.69848184886202702, 68.25755338999745447 ) ) ;
#48649 = CARTESIAN_POINT ( 'NONE',  ( -17.42409385541299471, -14.80920654474435594, 52.02966884056656482 ) ) ;
#48651 = CYLINDRICAL_SURFACE ( 'NONE', #1854, 1.249999999999998668 ) ;
#48650 = VECTOR ( 'NONE', #22177, 1000.000000000000227 ) ;
#48652 = FACE_BOUND ( 'NONE', #1896, .T. ) ;
#48653 = ORIENTED_EDGE ( 'NONE', *, *, #3829, .F. ) ;
#48654 = CARTESIAN_POINT ( 'NONE',  ( -10.29245896349820200, -16.96639176515380854, 57.87415878384224044 ) ) ;
#48655 = CARTESIAN_POINT ( 'NONE',  ( -10.53944108829644577, -16.08179026305252535, 71.51920757500701598 ) ) ;
#48656 = FACE_OUTER_BOUND ( 'NONE', #30254, .T. ) ;
#48657 = CARTESIAN_POINT ( 'NONE',  ( -16.39815193125092208, -7.826197509823805909, 63.81444203941759952 ) ) ;
#48658 = EDGE_LOOP ( 'NONE', ( #27927, #7271, #7577 ) ) ;
#48659 = DIRECTION ( 'NONE',  ( 3.071710424422018668E-17, -6.404604876783312462E-16, -1.000000000000000000 ) ) ;
#48660 = AXIS2_PLACEMENT_3D ( 'NONE', #4890, #3972, #43028 ) ;
#48661 = ORIENTED_EDGE ( 'NONE', *, *, #38916, .F. ) ;
#48662 = CARTESIAN_POINT ( 'NONE',  ( -12.27038842351949910, -10.07030034214893277, 64.10084541484442866 ) ) ;
#48663 = DIRECTION ( 'NONE',  ( -0.6380325334150322991, 0.7700094066334487453, 0.000000000000000000 ) ) ;
#48664 = CARTESIAN_POINT ( 'NONE',  ( -41.79100562011894482, -14.90920654474422058, 68.06470588235292496 ) ) ;
#48665 = VERTEX_POINT ( 'NONE', #28584 ) ;
#48666 = CARTESIAN_POINT ( 'NONE',  ( -16.11499574578559191, -22.14330172067997893, 58.38611333383489210 ) ) ;
#48667 = CARTESIAN_POINT ( 'NONE',  ( -18.32100859298913420, -22.20514637781060685, 68.93797822448765089 ) ) ;
#48668 = ORIENTED_EDGE ( 'NONE', *, *, #38515, .T. ) ;
#48669 = EDGE_CURVE ( 'NONE', #30823, #32996, #10288, .T. ) ;
#48670 = EDGE_LOOP ( 'NONE', ( #1659, #45284 ) ) ;
#48671 = ORIENTED_EDGE ( 'NONE', *, *, #25936, .F. ) ;
#48672 = CARTESIAN_POINT ( 'NONE',  ( -10.09291391017891115, -16.13494330055838333, 68.16263215882007387 ) ) ;
#48673 = CARTESIAN_POINT ( 'NONE',  ( -12.54422445394979135, -19.90840678475983694, 71.95086485943772914 ) ) ;
#48674 = DIRECTION ( 'NONE',  ( -0.9584484254710482487, -0.2852658684667118139, 3.516456354099036852E-08 ) ) ;
#48675 = CARTESIAN_POINT ( 'NONE',  ( -24.22092373047179947, -12.93688097883364208, 66.30246741375938768 ) ) ;
#48676 = CARTESIAN_POINT ( 'NONE',  ( -14.03871066829747249, -8.172719617054283958, 70.91452941929576070 ) ) ;
#48677 = CARTESIAN_POINT ( 'NONE',  ( -17.86146898453094423, -7.371889030502964957, 60.24207269745819104 ) ) ;
#48678 = EDGE_LOOP ( 'NONE', ( #25201, #23995, #11826, #39438, #8294 ) ) ;
#48679 = VERTEX_POINT ( 'NONE', #24165 ) ;
#48680 = ADVANCED_FACE ( 'NONE', ( #5701 ), #14801, .T. ) ;
#48681 = EDGE_CURVE ( 'NONE', #20147, #21395, #31392, .T. ) ;
#48682 = CARTESIAN_POINT ( 'NONE',  ( -16.59261295876471820, -7.800382739013279831, 60.34461612587266899 ) ) ;
#48683 = EDGE_CURVE ( 'NONE', #13759, #8796, #33688, .T. ) ;
#48684 = CARTESIAN_POINT ( 'NONE',  ( -13.92357616322991554, -8.232675698698610489, 74.32237735268643064 ) ) ;
#48685 = AXIS2_PLACEMENT_3D ( 'NONE', #29017, #34711, #24369 ) ;
#48686 = CYLINDRICAL_SURFACE ( 'NONE', #22093, 0.1500000000000050460 ) ;
#48687 = CARTESIAN_POINT ( 'NONE',  ( -18.55956930788366677, -7.446158750330262421, 74.02559786541287679 ) ) ;
#48688 = ADVANCED_FACE ( 'NONE', ( #2475 ), #32511, .T. ) ;
#48689 = AXIS2_PLACEMENT_3D ( 'NONE', #20418, #23872, #39362 ) ;
#48690 = ORIENTED_EDGE ( 'NONE', *, *, #23563, .F. ) ;
#48691 = CARTESIAN_POINT ( 'NONE',  ( -14.53659385650551705, -6.915538690918075382, 49.31353937987644542 ) ) ;
#48692 = AXIS2_PLACEMENT_3D ( 'NONE', #16857, #11194, #118 ) ;
#48693 = ORIENTED_EDGE ( 'NONE', *, *, #47178, .F. ) ;
#48694 = DIRECTION ( 'NONE',  ( -3.071710424422018668E-17, 6.404604876783312462E-16, 1.000000000000000000 ) ) ;
#48695 = EDGE_CURVE ( 'NONE', #48084, #42696, #10823, .T. ) ;
#48696 = FACE_OUTER_BOUND ( 'NONE', #38950, .T. ) ;
#48697 = LINE ( 'NONE', #14679, #4027 ) ;
#48698 = VECTOR ( 'NONE', #39947, 1000.000000000000114 ) ;
#48699 =( BOUNDED_SURFACE ( )  B_SPLINE_SURFACE ( 3, 1, ( 
 ( #29421, #10478 ),
 ( #40495, #14367 ),
 ( #10706, #22038 ),
 ( #37033, #3318 ),
 ( #18320, #33329 ),
 ( #44953, #34567 ),
 ( #11207, #3559 ) ),
 .UNSPECIFIED., .T., .F., .F. ) 
 B_SPLINE_SURFACE_WITH_KNOTS ( ( 4, 3, 4 ),
 ( 2, 2 ),
 ( 0.000000000000000000, 0.5000000000000000000, 1.000000000000000000 ),
 ( 0.000000000000000000, 1.000000000000000000 ),
 .UNSPECIFIED. ) 
 GEOMETRIC_REPRESENTATION_ITEM ( )  RATIONAL_B_SPLINE_SURFACE ( (
 ( 1.000000000000000000, 1.000000000000000000),
 ( 0.3333333333333335369, 0.3333333333333330373),
 ( 0.3333333333333335369, 0.3333333333333330373),
 ( 1.000000000000000000, 1.000000000000000000),
 ( 0.3333333333333333703, 0.3333333333333333703),
 ( 0.3333333333333333703, 0.3333333333333333703),
 ( 1.000000000000000000, 1.000000000000000000) ) ) 
 REPRESENTATION_ITEM ( '' )  SURFACE ( )  );
#48700 = ORIENTED_EDGE ( 'NONE', *, *, #31851, .T. ) ;
#48701 = DIRECTION ( 'NONE',  ( 6.374839753205895344E-22, 0.007114381193220357599, -0.9999746924698832418 ) ) ;
#48702 = LINE ( 'NONE', #12188, #36122 ) ;
#48703 = CARTESIAN_POINT ( 'NONE',  ( -35.42409385541304800, -9.359200813967566646, 50.49621490985803263 ) ) ;
#48704 = ORIENTED_EDGE ( 'NONE', *, *, #16820, .T. ) ;
#48705 = DIRECTION ( 'NONE',  ( -3.071710424422018668E-17, 6.404604876783312462E-16, 1.000000000000000000 ) ) ;
#48706 = CARTESIAN_POINT ( 'NONE',  ( -10.05839037049808127, -15.92727522337501611, 64.55125644017783770 ) ) ;
#48707 = ORIENTED_EDGE ( 'NONE', *, *, #45906, .T. ) ;
#48708 = CARTESIAN_POINT ( 'NONE',  ( -24.68835726793385987, -16.46241053826067358, 59.32343638323965962 ) ) ;
#48709 =( BOUNDED_SURFACE ( )  B_SPLINE_SURFACE ( 3, 1, ( 
 ( #22425, #38401 ),
 ( #37677, #14752 ),
 ( #3970, #42118 ),
 ( #30324, #18979 ),
 ( #23408, #33984 ),
 ( #38160, #15500 ),
 ( #41882, #37927 ) ),
 .UNSPECIFIED., .T., .F., .F. ) 
 B_SPLINE_SURFACE_WITH_KNOTS ( ( 4, 3, 4 ),
 ( 2, 2 ),
 ( 0.000000000000000000, 0.5000000000000000000, 1.000000000000000000 ),
 ( 0.000000000000000000, 1.000000000000000000 ),
 .UNSPECIFIED. ) 
 GEOMETRIC_REPRESENTATION_ITEM ( )  RATIONAL_B_SPLINE_SURFACE ( (
 ( 1.000000000000000000, 1.000000000000000000),
 ( 0.3333333333333335369, 0.3333333333333330373),
 ( 0.3333333333333335369, 0.3333333333333330373),
 ( 1.000000000000000000, 1.000000000000000000),
 ( 0.3333333333333333703, 0.3333333333333333703),
 ( 0.3333333333333333703, 0.3333333333333333703),
 ( 1.000000000000000000, 1.000000000000000000) ) ) 
 REPRESENTATION_ITEM ( '' )  SURFACE ( )  );
#48710 = ORIENTED_EDGE ( 'NONE', *, *, #6211, .F. ) ;
#48711 = CARTESIAN_POINT ( 'NONE',  ( -10.64242474325409304, -12.85371797616438272, 71.35261706278205907 ) ) ;
#48712 = DIRECTION ( 'NONE',  ( -1.000000000000000000, 3.159776991290051445E-16, -3.534154189880001717E-15 ) ) ;
#48713 = ORIENTED_EDGE ( 'NONE', *, *, #29543, .T. ) ;
#48714 = CARTESIAN_POINT ( 'NONE',  ( -10.37497031036790851, -14.69804325442274617, 71.47782692816423378 ) ) ;
#48715 = LINE ( 'NONE', #47989, #42280 ) ;
#48716 = AXIS2_PLACEMENT_3D ( 'NONE', #24738, #27929, #39259 ) ;
#48717 = VERTEX_POINT ( 'NONE', #17953 ) ;
#48718 = CARTESIAN_POINT ( 'NONE',  ( -22.11256825271130921, -9.019435748674359488, 63.38492064941936377 ) ) ;
#48719 = LINE ( 'NONE', #45065, #44674 ) ;
#48720 = ADVANCED_FACE ( 'NONE', ( #21671 ), #9401, .T. ) ;
#48721 = CARTESIAN_POINT ( 'NONE',  ( -50.42609385541305755, -14.90920654474415841, 62.92941176470587550 ) ) ;
#48722 = CARTESIAN_POINT ( 'NONE',  ( -14.46752719259218800, -19.14754880513559954, 49.52966884056656482 ) ) ;
#48723 = ORIENTED_EDGE ( 'NONE', *, *, #19122, .T. ) ;
#48724 = CARTESIAN_POINT ( 'NONE',  ( -15.01478382166781600, -8.183512691096048286, 56.85559764823393891 ) ) ;
#48725 = AXIS2_PLACEMENT_3D ( 'NONE', #18672, #23361, #15708 ) ;
#48726 = B_SPLINE_CURVE_WITH_KNOTS ( 'NONE', 3,
 ( #22521, #30172, #26218, #3558, #37774, #18319, #41473, #18827, #33328, #7276 ),
 .UNSPECIFIED., .F., .F.,
 ( 4, 2, 2, 2, 4 ),
 ( 0.1272669073658529160, 0.2522669073439766096, 0.3772669073221003311, 0.5022669073002239415, 0.6272669072783476629 ),
 .UNSPECIFIED. ) ;
#48727 = CARTESIAN_POINT ( 'NONE',  ( -21.79534323032677179, -8.776250307867684342, 70.25415672280243484 ) ) ;
#48728 = CARTESIAN_POINT ( 'NONE',  ( -17.42409385541299471, -14.80920654474435594, 52.02966884056656482 ) ) ;
#48729 = ADVANCED_FACE ( 'NONE', ( #25849 ), #2940, .T. ) ;
#48730 = ORIENTED_EDGE ( 'NONE', *, *, #18953, .T. ) ;
#48731 = EDGE_LOOP ( 'NONE', ( #43860, #40303, #47366, #622, #728 ) ) ;
#48732 = DIRECTION ( 'NONE',  ( 0.1847813031241906101, -0.9827796650397888634, 7.910442904995644076E-08 ) ) ;
#48733 = CARTESIAN_POINT ( 'NONE',  ( -10.40434556984383185, -14.15519790090335839, 61.21261492209757904 ) ) ;
#48734 = NEXT_ASSEMBLY_USAGE_OCCURRENCE ( 'NAUO1', ' ', ' ', #16839, #9649, $ ) ;
#48735 = NEXT_ASSEMBLY_USAGE_OCCURRENCE ( 'NAUO2', ' ', ' ', #16839, #35187, $ ) ;
#48736 = NEXT_ASSEMBLY_USAGE_OCCURRENCE ( 'NAUO3', ' ', ' ', #16839, #29471, $ ) ;
#48737 = NEXT_ASSEMBLY_USAGE_OCCURRENCE ( 'NAUO4', ' ', ' ', #16839, #42442, $ ) ;
#48738 = NEXT_ASSEMBLY_USAGE_OCCURRENCE ( 'NAUO5', ' ', ' ', #16839, #37283, $ ) ;
#48739 = NEXT_ASSEMBLY_USAGE_OCCURRENCE ( 'NAUO6', ' ', ' ', #16839, #18332, $ ) ;
#48740 = NEXT_ASSEMBLY_USAGE_OCCURRENCE ( 'NAUO7', ' ', ' ', #16839, #16217, $ ) ;
#48741 = NEXT_ASSEMBLY_USAGE_OCCURRENCE ( 'NAUO8', ' ', ' ', #16839, #9035, $ ) ;
#48742 = NEXT_ASSEMBLY_USAGE_OCCURRENCE ( 'NAUO9', ' ', ' ', #16839, #9649, $ ) ;
ENDSEC;
END-ISO-10303-21;
